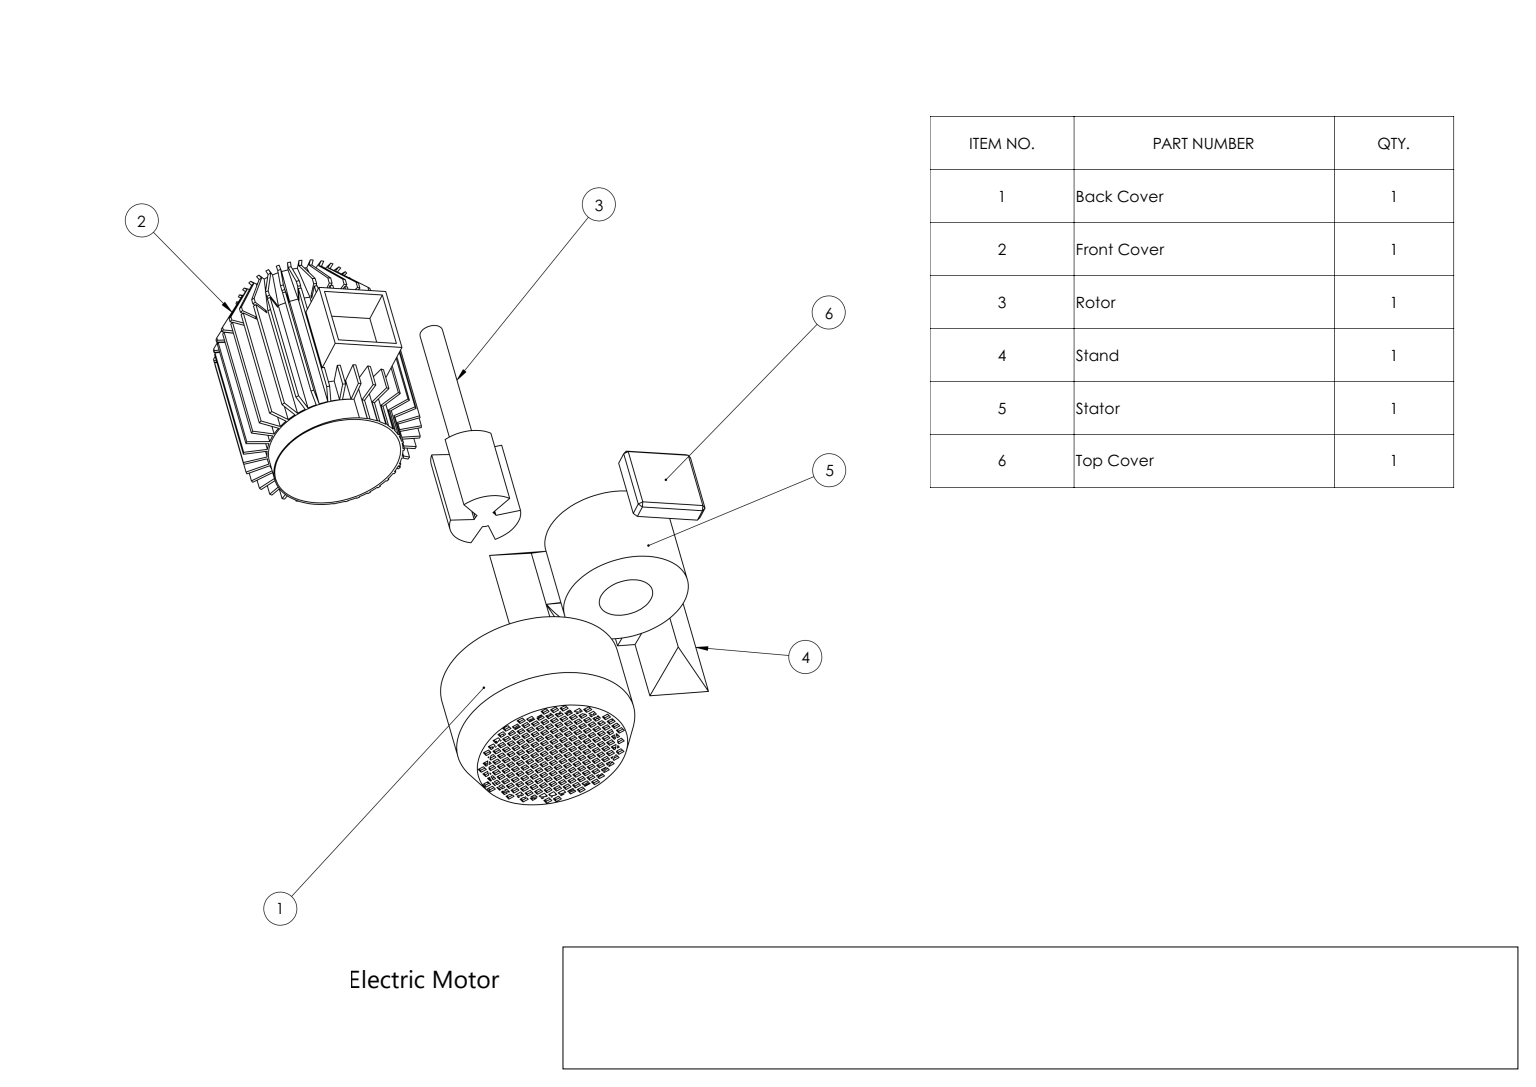
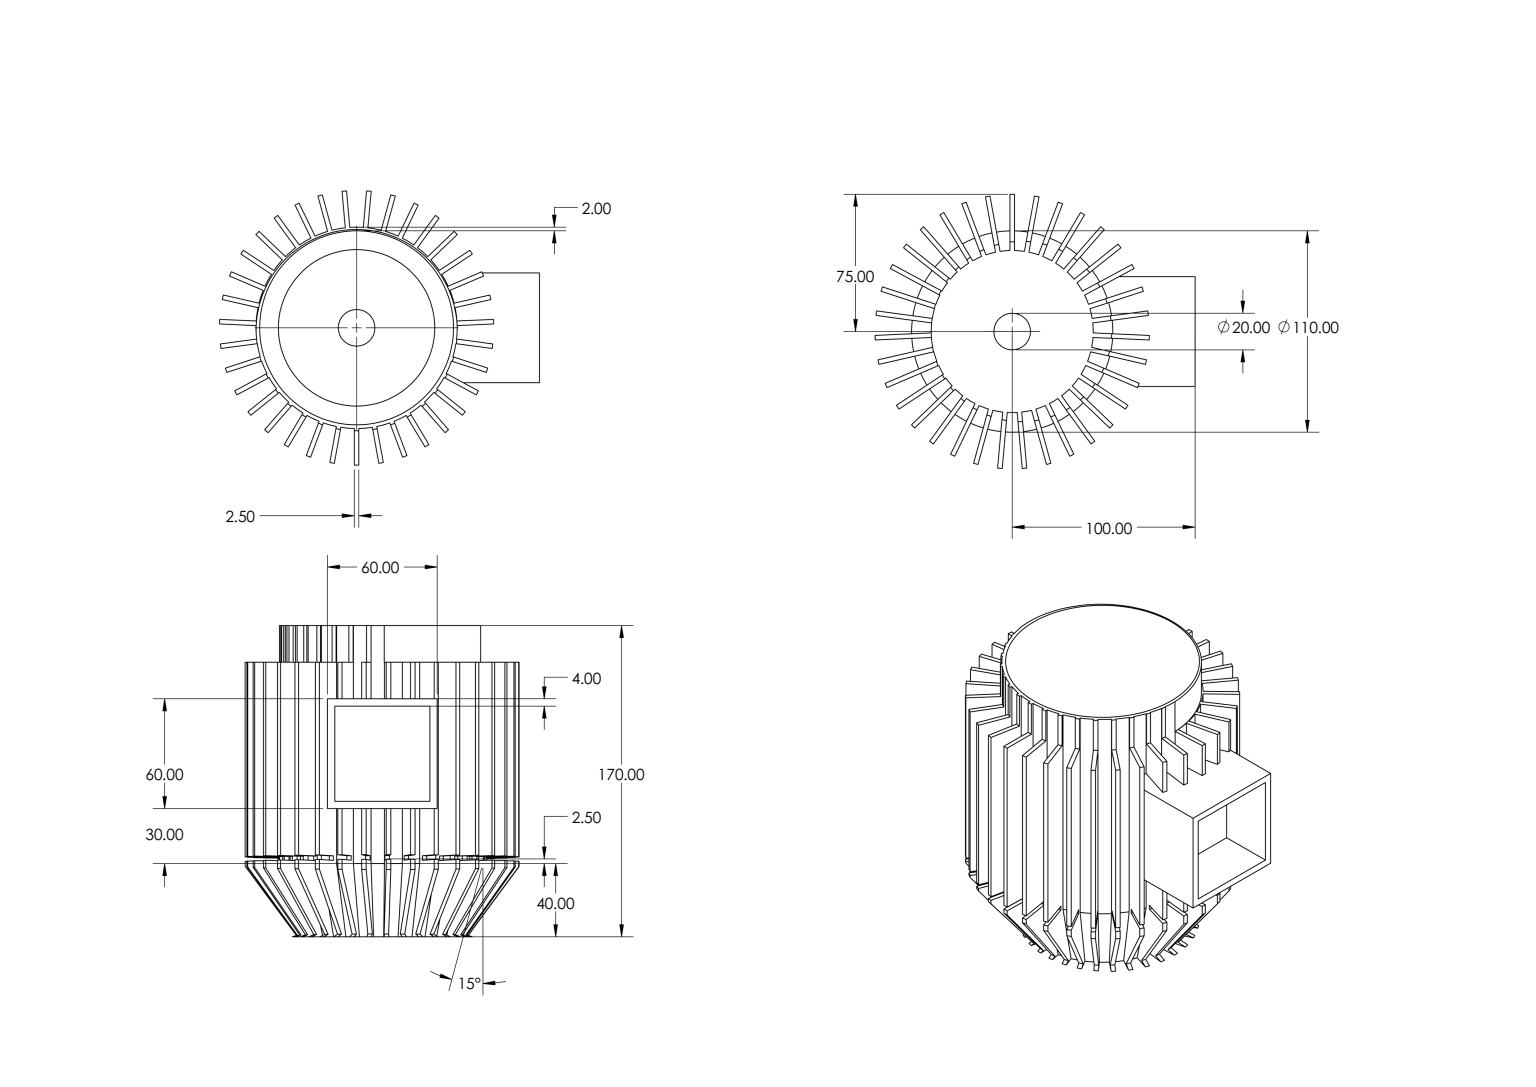
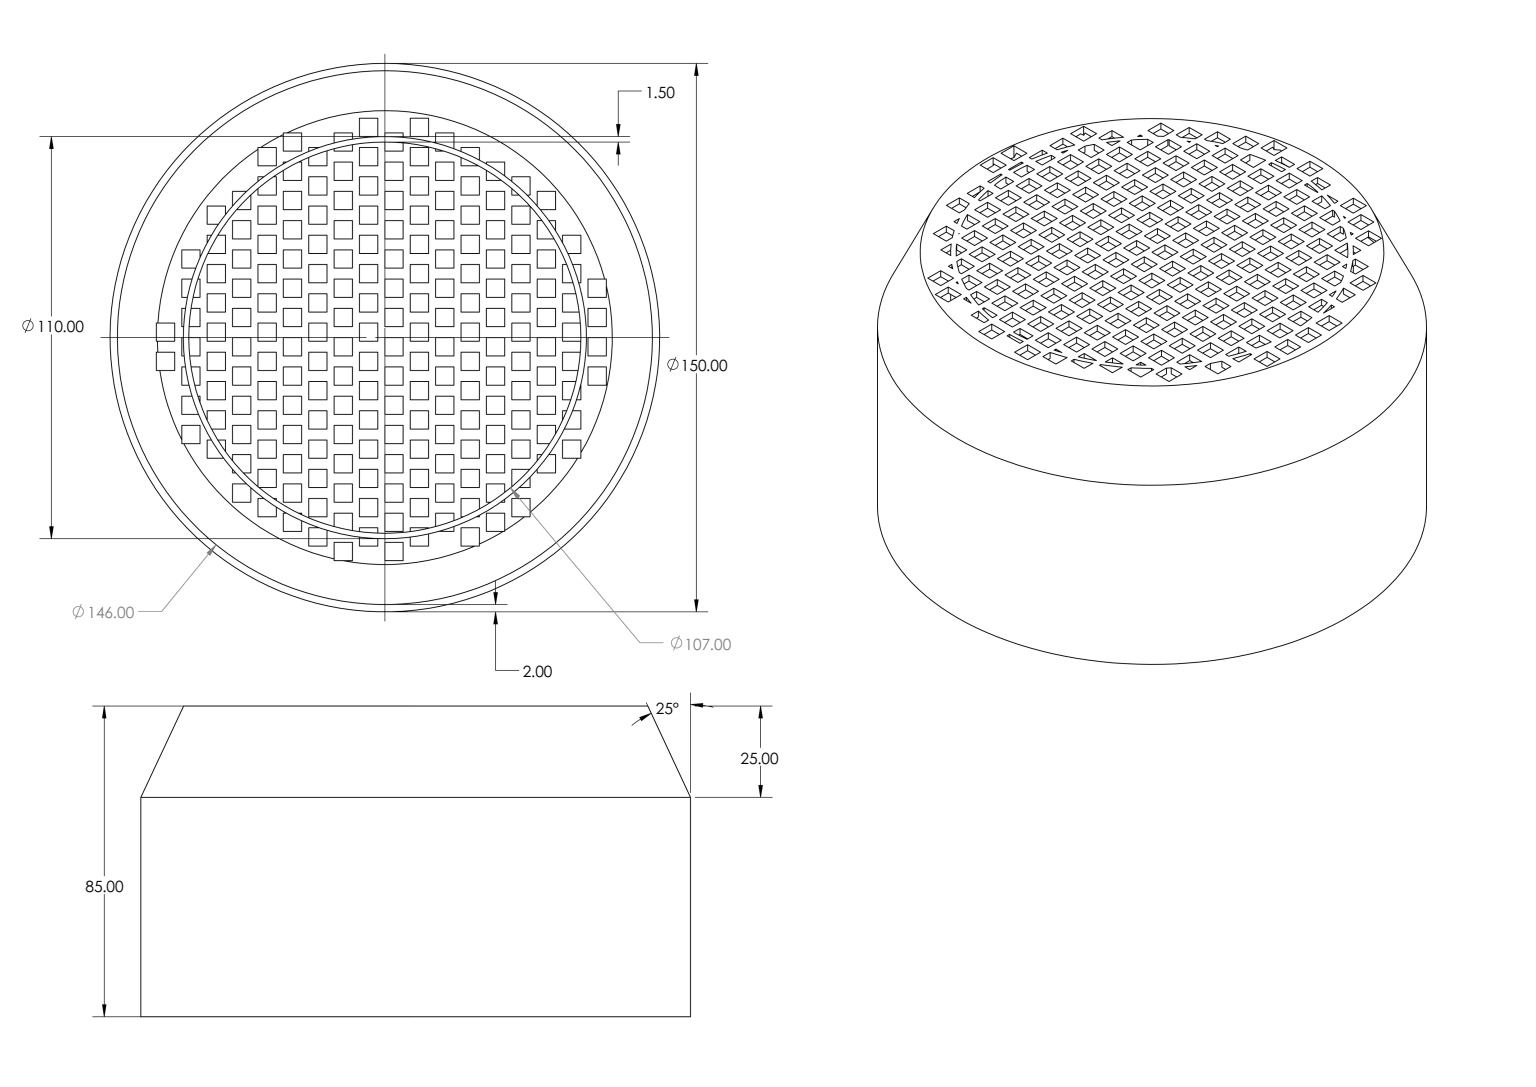
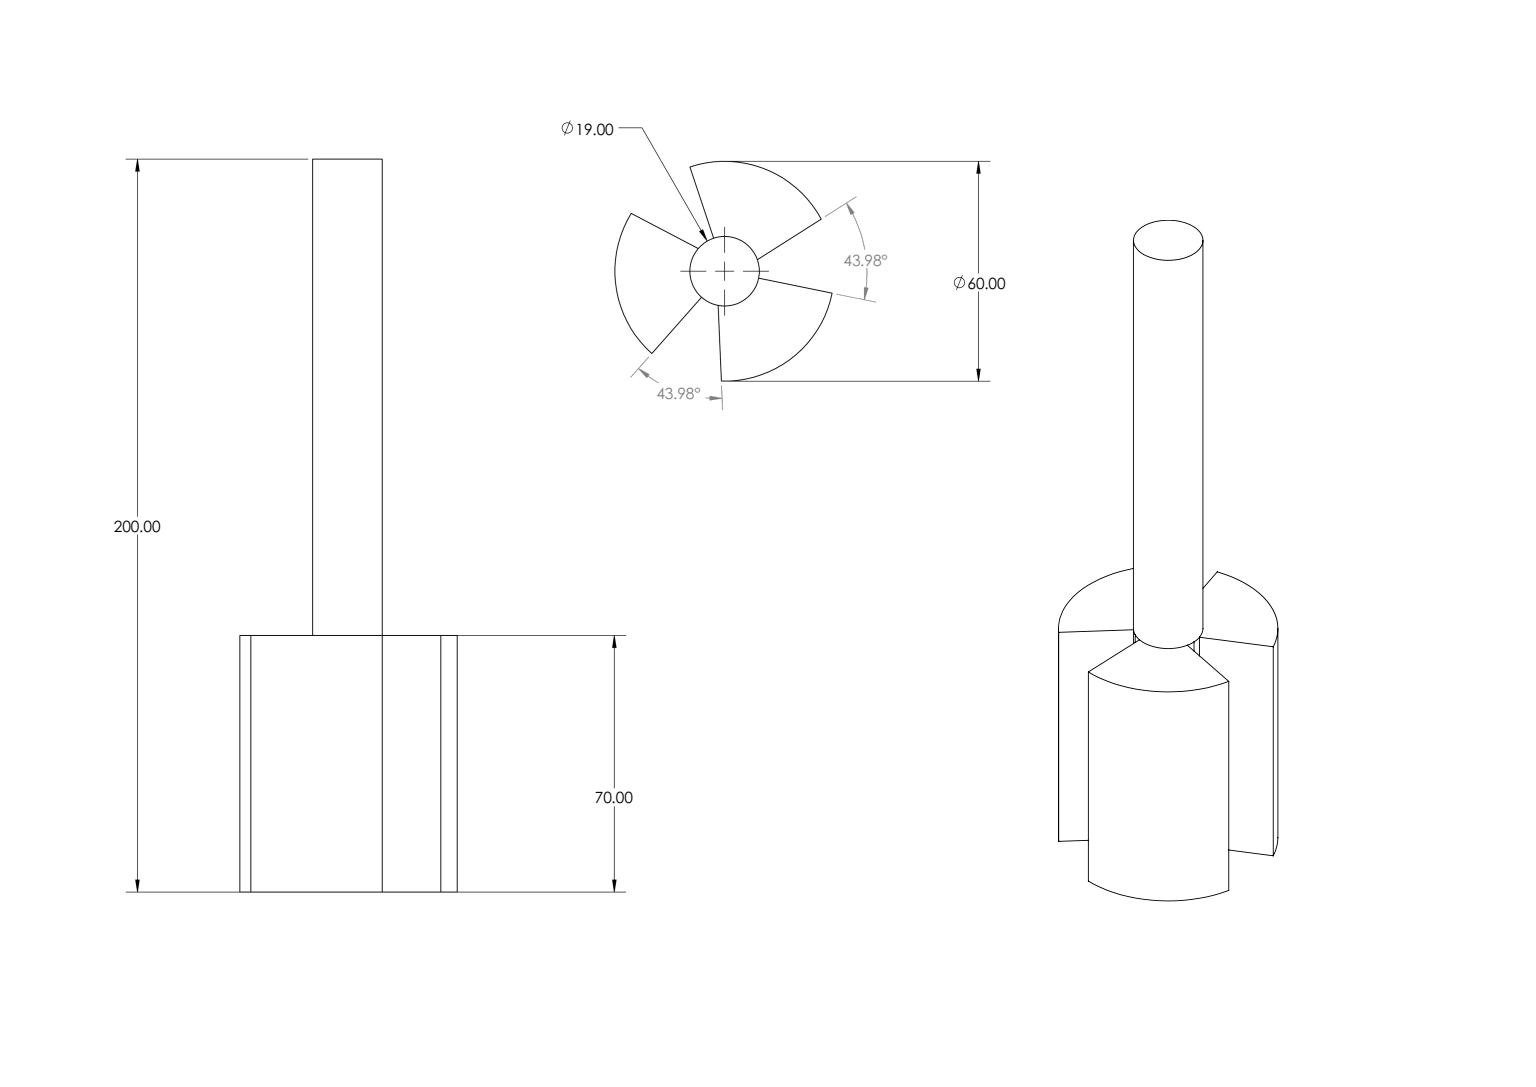
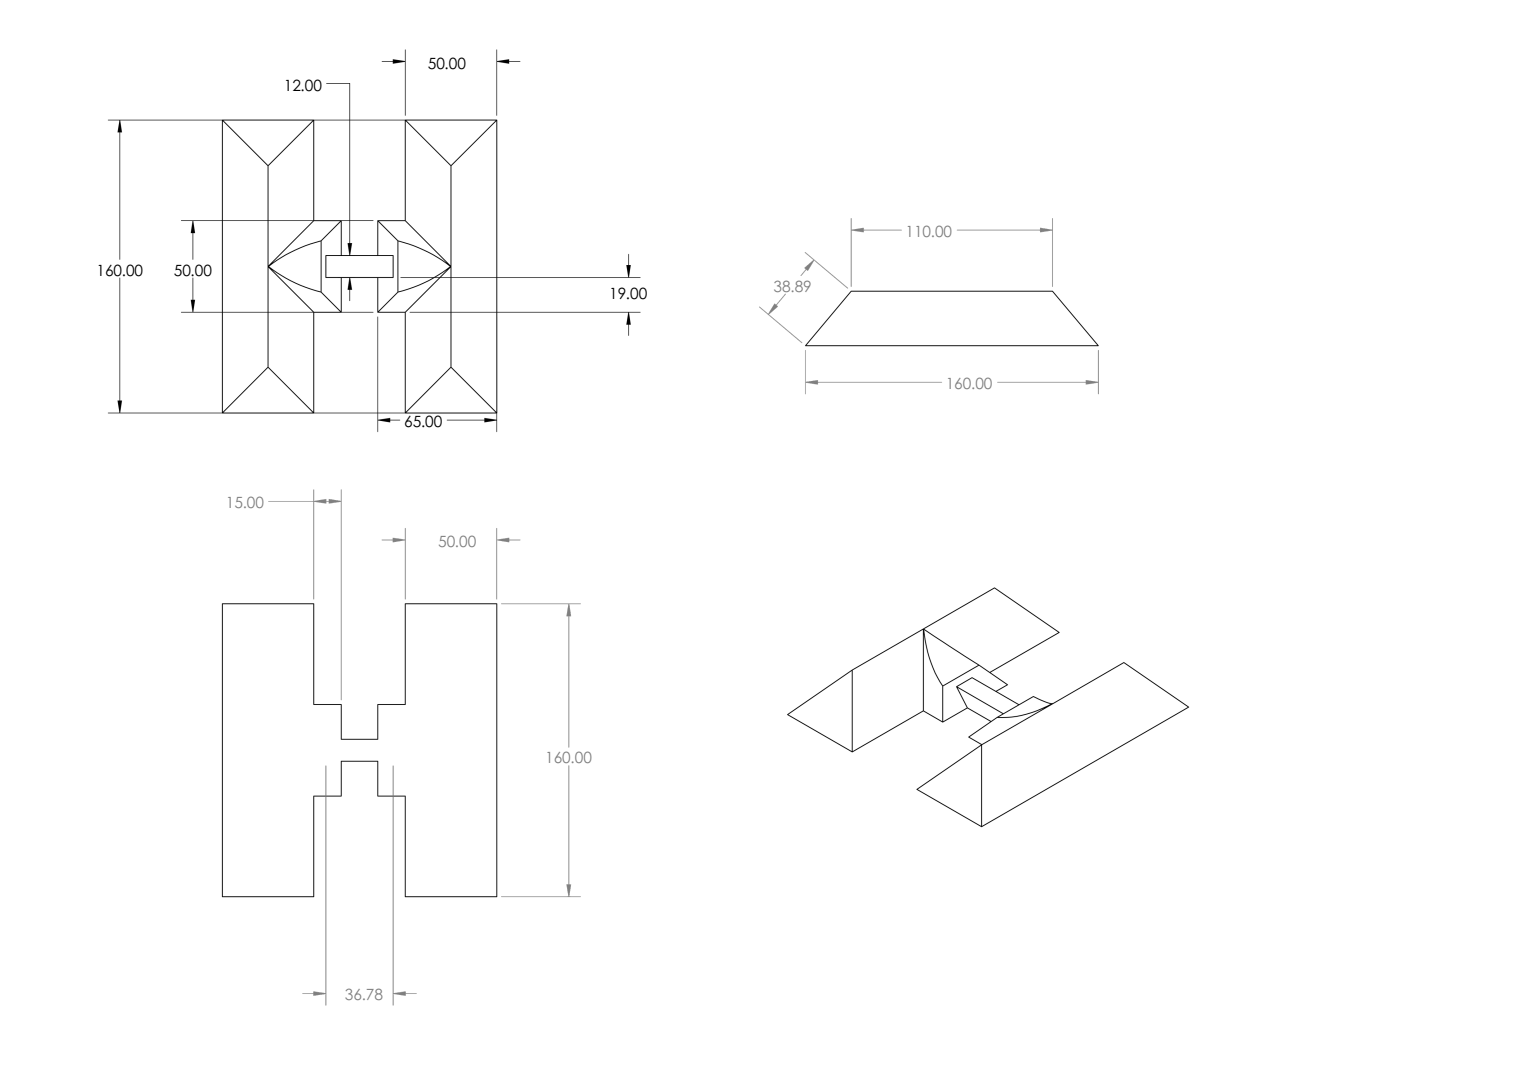
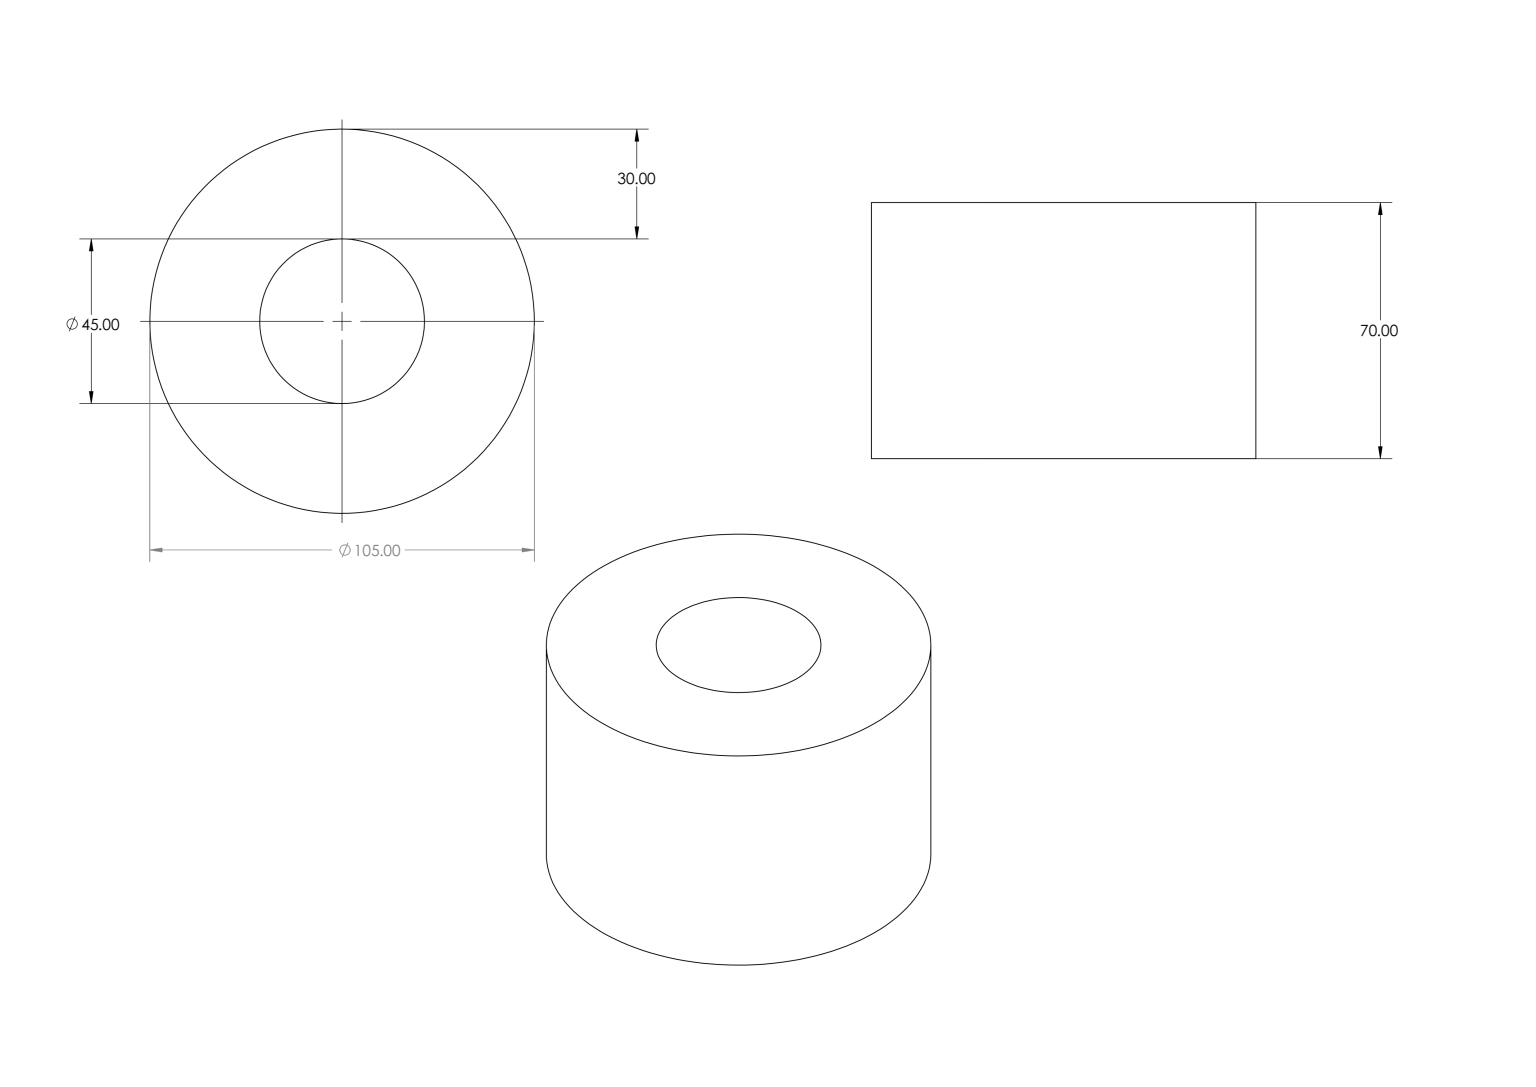
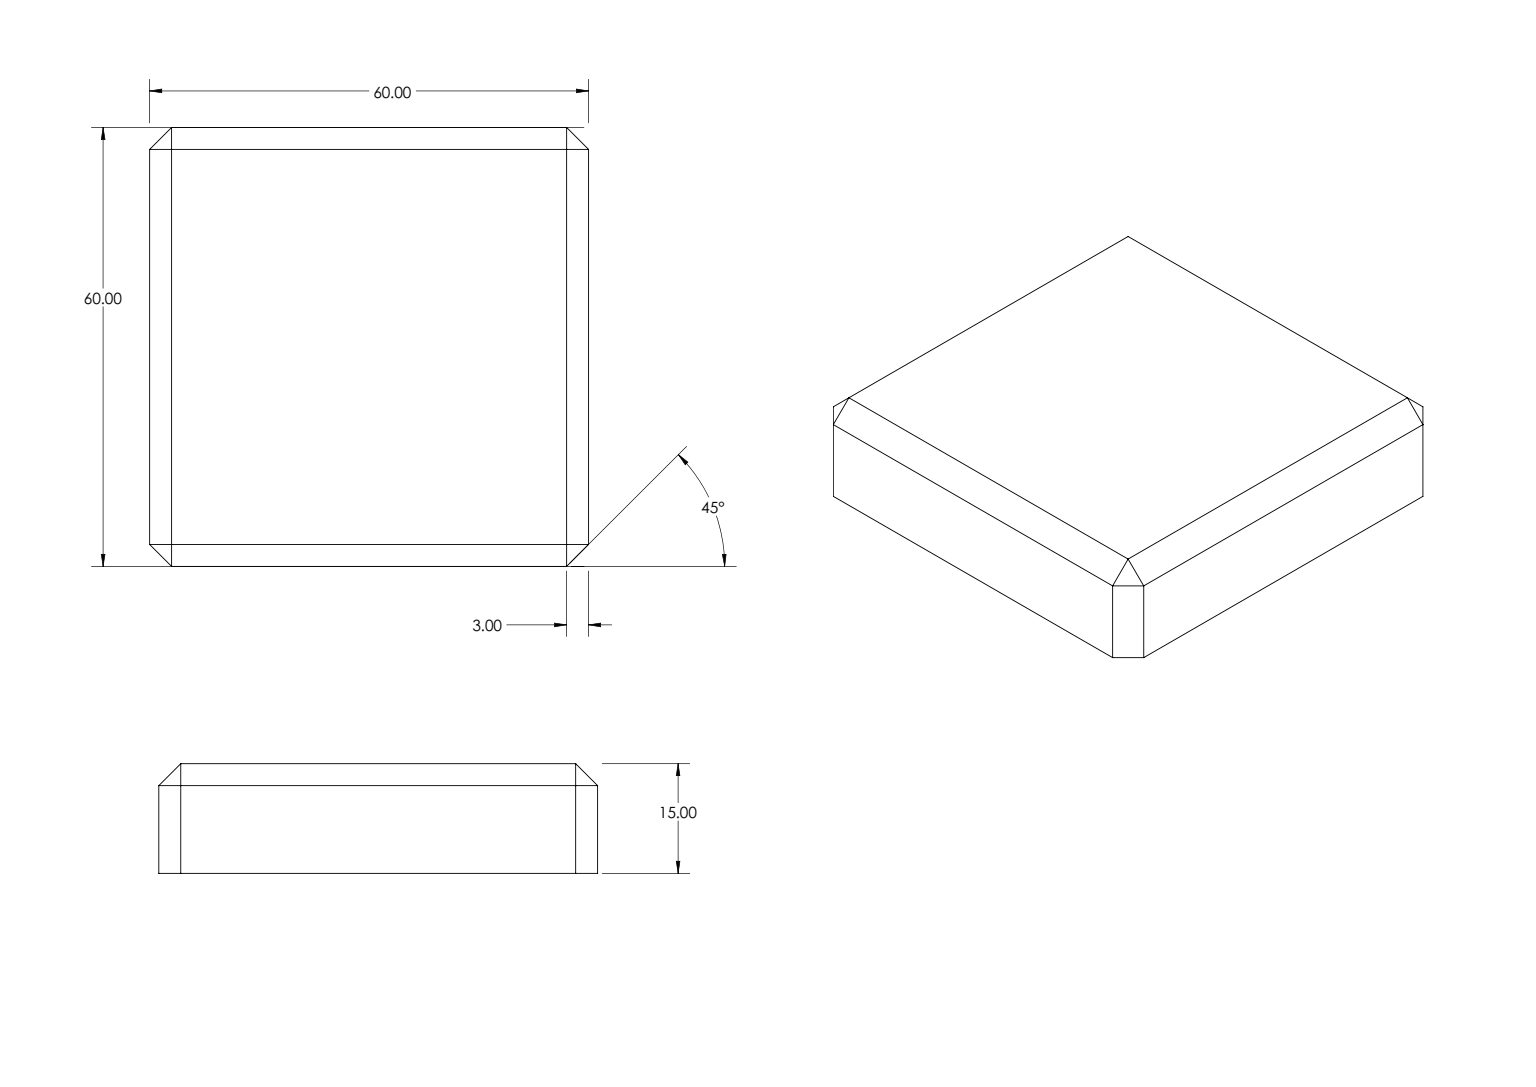
ISO-10303-21;
HEADER;
FILE_DESCRIPTION (('STEP AP214'),
    '1' );
FILE_NAME ('MAT-026',
    '2026-10-24T11:32:06',
    ( '' ),
    ( '' ),
    'SwSTEP 2.0',
    'SolidWorks 2025',
    '' );
FILE_SCHEMA (( 'AUTOMOTIVE_DESIGN' ));
ENDSEC;

DATA;
#1 = ORIENTED_EDGE ( 'NONE', *, *, #41545, .F. ) ;
#2 = DIRECTION ( 'NONE',  ( -0.000000000000000000, 1.000000000000000000, -0.000000000000000000 ) ) ;
#3 = DIRECTION ( 'NONE',  ( 0.5508969814521065267, -1.160734090543304660E-16, -0.8345732537212999791 ) ) ;
#4 = ORIENTED_EDGE ( 'NONE', *, *, #46916, .F. ) ;
#5 = FACE_OUTER_BOUND ( 'NONE', #37922, .T. ) ;
#6 = EDGE_CURVE ( 'NONE', #44322, #24123, #48534, .T. ) ;
#7 = EDGE_CURVE ( 'NONE', #12139, #21915, #4265, .T. ) ;
#8 = ORIENTED_EDGE ( 'NONE', *, *, #4272, .T. ) ;
#9 = ORIENTED_EDGE ( 'NONE', *, *, #40098, .F. ) ;
#10 = APPLICATION_PROTOCOL_DEFINITION ( 'draft international standard', 'automotive_design', 1998, #14403 ) ;
#11 = EDGE_CURVE ( 'NONE', #30195, #20299, #27750, .T. ) ;
#12 = EDGE_LOOP ( 'NONE', ( #15734, #18361, #15608, #13795, #3369 ) ) ;
#13 = LINE ( 'NONE', #35645, #41620 ) ;
#14 = AXIS2_PLACEMENT_3D ( 'NONE', #39527, #281, #16034 ) ;
#15 = LINE ( 'NONE', #8019, #14262 ) ;
#16 = VECTOR ( 'NONE', #2889, 39.37007874015748143 ) ;
#17 = DIRECTION ( 'NONE',  ( -1.000000000000000000, 0.000000000000000000, -0.000000000000000000 ) ) ;
#18 = CARTESIAN_POINT ( 'NONE',  ( -1.221295136473707243, 0.000000000000000000, 1.323086612934683215 ) ) ;
#19 = ORIENTED_EDGE ( 'NONE', *, *, #43886, .F. ) ;
#20 = ORIENTED_EDGE ( 'NONE', *, *, #36805, .T. ) ;
#21 = CARTESIAN_POINT ( 'NONE',  ( -1.985260859929297572, 0.000000000000000000, 0.9448818897637749625 ) ) ;
#22 = PLANE ( 'NONE',  #45699 ) ;
#23 = AXIS2_PLACEMENT_3D ( 'NONE', #45636, #18051, #42046 ) ;
#24 = VERTEX_POINT ( 'NONE', #23123 ) ;
#25 = CARTESIAN_POINT ( 'NONE',  ( 0.2727639067037610499, 0.000000000000000000, 1.417322834645662777 ) ) ;
#26 = DIRECTION ( 'NONE',  ( 1.000000000000000000, -0.000000000000000000, 0.000000000000000000 ) ) ;
#27 = EDGE_CURVE ( 'NONE', #10700, #41467, #27241, .T. ) ;
#28 = LINE ( 'NONE', #15774, #16810 ) ;
#29 = DIRECTION ( 'NONE',  ( 1.000000000000000000, 0.000000000000000000, 0.000000000000000000 ) ) ;
#30 = CARTESIAN_POINT ( 'NONE',  ( -1.091055626815042645, 3.346456692913386100, 1.889763779527550147 ) ) ;
#31 = ORIENTED_EDGE ( 'NONE', *, *, #29718, .F. ) ;
#32 = DIRECTION ( 'NONE',  ( -0.9998717552508122886, -0.01601477604151185785, 0.000000000000000000 ) ) ;
#34 = EDGE_CURVE ( 'NONE', #42119, #2129, #11002, .T. ) ;
#33 = DIRECTION ( 'NONE',  ( -0.2660368455666687892, 1.119010597708915320E-16, -0.9639628606958549062 ) ) ;
#35 = EDGE_CURVE ( 'NONE', #20944, #31120, #9767, .T. ) ;
#36 = EDGE_LOOP ( 'NONE', ( #12424, #14869, #12144, #2059, #5425, #21039 ) ) ;
#37 = ORIENTED_EDGE ( 'NONE', *, *, #50660, .F. ) ;
#38 = CARTESIAN_POINT ( 'NONE',  ( -0.3486774197067339376, 0.000000000000000000, 2.204724409448808764 ) ) ;
#39 = FACE_OUTER_BOUND ( 'NONE', #43225, .T. ) ;
#40 = DIRECTION ( 'NONE',  ( 0.8090169943749422332, -6.825848574540668760E-17, 0.5877852522924802425 ) ) ;
#41 = ORIENTED_EDGE ( 'NONE', *, *, #32145, .F. ) ;
#42 = VERTEX_POINT ( 'NONE', #46835 ) ;
#43 = FACE_OUTER_BOUND ( 'NONE', #749, .T. ) ;
#44 = ORIENTED_EDGE ( 'NONE', *, *, #47362, .F. ) ;
#45 = FACE_OUTER_BOUND ( 'NONE', #8156, .T. ) ;
#46 = ORIENTED_EDGE ( 'NONE', *, *, #11822, .F. ) ;
#47 = VECTOR ( 'NONE', #45929, 39.37007874015748143 ) ;
#48 = CARTESIAN_POINT ( 'NONE',  ( 0.08139965876239094178, 1.610780518492231694, 0.000000000000000000 ) ) ;
#49 = PLANE ( 'NONE',  #39583 ) ;
#50 = DIRECTION ( 'NONE',  ( 1.734723475976806848E-16, -0.000000000000000000, 1.000000000000000000 ) ) ;
#51 = VECTOR ( 'NONE', #38671, 39.37007874015748143 ) ;
#52 = ORIENTED_EDGE ( 'NONE', *, *, #36287, .T. ) ;
#53 = DIMENSIONAL_EXPONENTS ( 1.000000000000000000, 0.000000000000000000, 0.000000000000000000, 0.000000000000000000, 0.000000000000000000, 0.000000000000000000, 0.000000000000000000 ) ;
#54 = VERTEX_POINT ( 'NONE', #23369 ) ;
#55 = ORIENTED_EDGE ( 'NONE', *, *, #40975, .F. ) ;
#56 = DIRECTION ( 'NONE',  ( -6.104789737168205836E-17, 1.000000000000000000, 1.134460028949762747E-16 ) ) ;
#57 = PLANE ( 'NONE',  #9017 ) ;
#58 = VERTEX_POINT ( 'NONE', #22875 ) ;
#59 = EDGE_LOOP ( 'NONE', ( #42044, #32903, #33887, #36079 ) ) ;
#60 = CARTESIAN_POINT ( 'NONE',  ( 1.091055626815043311, 3.346456692913386100, 1.801691980386208591 ) ) ;
#61 = DIRECTION ( 'NONE',  ( 1.000000000000000000, 0.000000000000000000, 0.000000000000000000 ) ) ;
#62 = AXIS2_PLACEMENT_3D ( 'NONE', #50431, #10999, #38625 ) ;
#63 = DIRECTION ( 'NONE',  ( -0.01601477604151182663, 0.9998717552508123996, -0.000000000000000000 ) ) ;
#64 = ORIENTED_EDGE ( 'NONE', *, *, #33322, .T. ) ;
#65 = VERTEX_POINT ( 'NONE', #11508 ) ;
#66 = DIRECTION ( 'NONE',  ( -0.01601477604151182663, 0.9998717552508123996, -0.000000000000000000 ) ) ;
#67 = LINE ( 'NONE', #23560, #12596 ) ;
#68 = DIRECTION ( 'NONE',  ( 1.734723475976806848E-16, -0.000000000000000000, 1.000000000000000000 ) ) ;
#69 = ORIENTED_EDGE ( 'NONE', *, *, #18487, .T. ) ;
#70 = CARTESIAN_POINT ( 'NONE',  ( -1.775400203342670347, 1.691590761327236958, -2.359903268218729089 ) ) ;
#71 = CARTESIAN_POINT ( 'NONE',  ( -1.684292108503798069, 6.692913385826772199, 1.406123411605399331 ) ) ;
#72 = EDGE_CURVE ( 'NONE', #49919, #13698, #39123, .T. ) ;
#73 = ORIENTED_EDGE ( 'NONE', *, *, #20191, .T. ) ;
#74 = EDGE_CURVE ( 'NONE', #40300, #35551, #37050, .T. ) ;
#75 = LINE ( 'NONE', #35456, #37348 ) ;
#76 = ORIENTED_EDGE ( 'NONE', *, *, #46509, .T. ) ;
#77 = ORIENTED_EDGE ( 'NONE', *, *, #24929, .F. ) ;
#78 = LINE ( 'NONE', #47286, #4826 ) ;
#79 = EDGE_CURVE ( 'NONE', #50716, #12064, #21041, .T. ) ;
#80 = CARTESIAN_POINT ( 'NONE',  ( -1.723687301221637380, 0.000000000000000000, -1.311649477509825745 ) ) ;
#81 = CARTESIAN_POINT ( 'NONE',  ( -0.8942052331142547050, 3.346456692913386100, 0.3149606299212580063 ) ) ;
#82 = EDGE_CURVE ( 'NONE', #36271, #42094, #44767, .T. ) ;
#83 = CARTESIAN_POINT ( 'NONE',  ( -2.952069331832154919, 2.755905511811027164, 1.181102362204724088 ) ) ;
#84 = ORIENTED_EDGE ( 'NONE', *, *, #20132, .T. ) ;
#85 = ORIENTED_EDGE ( 'NONE', *, *, #1655, .T. ) ;
#86 = ORIENTED_EDGE ( 'NONE', *, *, #35024, .F. ) ;
#87 = CARTESIAN_POINT ( 'NONE',  ( -2.454875160333845674, 0.000000000000000000, -0.3543307086614173040 ) ) ;
#88 = DIRECTION ( 'NONE',  ( -0.9362348706397368714, 0.000000000000000000, -0.3513748240813434620 ) ) ;
#89 = VECTOR ( 'NONE', #24437, 39.37007874015748143 ) ;
#90 = AXIS2_PLACEMENT_3D ( 'NONE', #4084, #31446, #43558 ) ;
#91 = ADVANCED_FACE ( 'NONE', ( #40920 ), #12786, .F. ) ;
#92 = DIRECTION ( 'NONE',  ( 0.000000000000000000, 0.000000000000000000, 1.000000000000000000 ) ) ;
#93 = LINE ( 'NONE', #12233, #1484 ) ;
#94 = ORIENTED_EDGE ( 'NONE', *, *, #13556, .F. ) ;
#95 = DIRECTION ( 'NONE',  ( 0.000000000000000000, 0.000000000000000000, -1.000000000000000000 ) ) ;
#96 = EDGE_CURVE ( 'NONE', #18423, #30154, #5544, .T. ) ;
#97 = VECTOR ( 'NONE', #41859, 39.37007874015748143 ) ;
#98 = CARTESIAN_POINT ( 'NONE',  ( 0.8182917201112819283, 0.000000000000000000, -0.6692913385826764205 ) ) ;
#99 = EDGE_LOOP ( 'NONE', ( #34506, #24501, #26752, #36610 ) ) ;
#100 = AXIS2_PLACEMENT_3D ( 'NONE', #33022, #17513, #29384 ) ;
#101 = LINE ( 'NONE', #15846, #7552 ) ;
#102 = CARTESIAN_POINT ( 'NONE',  ( -0.8182917201112819283, 3.267716535433071279, -1.417322834645664331 ) ) ;
#103 = PLANE ( 'NONE',  #37876 ) ;
#104 = EDGE_CURVE ( 'NONE', #46852, #34665, #24146, .T. ) ;
#105 = ORIENTED_EDGE ( 'NONE', *, *, #7025, .F. ) ;
#106 = PLANE ( 'NONE',  #20146 ) ;
#107 = CARTESIAN_POINT ( 'NONE',  ( 1.636583440222563857, 3.267716535433071279, -2.839019714148966584E-16 ) ) ;
#108 = CARTESIAN_POINT ( 'NONE',  ( 2.576863348864710801, 1.456480680773285741, 1.442554885838449596 ) ) ;
#109 = ORIENTED_EDGE ( 'NONE', *, *, #48882, .F. ) ;
#110 = LINE ( 'NONE', #16120, #44470 ) ;
#111 = ORIENTED_EDGE ( 'NONE', *, *, #20916, .T. ) ;
#112 = CARTESIAN_POINT ( 'NONE',  ( -1.312623452344869657, 1.205361022782829114E-17, 1.722945714930904648 ) ) ;
#113 = EDGE_CURVE ( 'NONE', #26527, #41000, #12273, .T. ) ;
#114 = FACE_OUTER_BOUND ( 'NONE', #41587, .T. ) ;
#115 = B_SPLINE_CURVE_WITH_KNOTS ( 'NONE', 3,
 ( #45279, #2696, #10703, #6825 ),
 .UNSPECIFIED., .F., .F.,
 ( 4, 4 ),
 ( 0.0008439222489648032970, 0.003344231527576960444 ),
 .UNSPECIFIED. ) ;
#116 = DIRECTION ( 'NONE',  ( -0.9959742939952384022, 1.288287287306305283E-16, -0.08963930890344089242 ) ) ;
#117 = DIRECTION ( 'NONE',  ( -1.000000000000000000, 0.000000000000000000, 1.734723475976806848E-16 ) ) ;
#118 = ORIENTED_EDGE ( 'NONE', *, *, #20637, .F. ) ;
#119 = ORIENTED_EDGE ( 'NONE', *, *, #43992, .F. ) ;
#120 = FACE_OUTER_BOUND ( 'NONE', #11448, .T. ) ;
#121 = DIRECTION ( 'NONE',  ( -1.000000000000000000, -0.000000000000000000, -0.000000000000000000 ) ) ;
#122 = VERTEX_POINT ( 'NONE', #36283 ) ;
#123 = DIRECTION ( 'NONE',  ( 1.000000000000000000, 0.000000000000000000, -3.469446951953613696E-16 ) ) ;
#124 = LINE ( 'NONE', #20773, #45818 ) ;
#125 = CARTESIAN_POINT ( 'NONE',  ( 0.000000000000000000, 1.574803149606302854, 0.000000000000000000 ) ) ;
#126 = VECTOR ( 'NONE', #40753, 39.37007874015748143 ) ;
#127 = FACE_OUTER_BOUND ( 'NONE', #15551, .T. ) ;
#128 = AXIS2_PLACEMENT_3D ( 'NONE', #50687, #394, #43496 ) ;
#129 = VERTEX_POINT ( 'NONE', #32937 ) ;
#130 = ORIENTED_EDGE ( 'NONE', *, *, #3262, .F. ) ;
#131 = FACE_OUTER_BOUND ( 'NONE', #28949, .T. ) ;
#132 = CARTESIAN_POINT ( 'NONE',  ( 0.2727639067037604392, 3.267716535433071279, -4.731699523581607276E-17 ) ) ;
#133 = DIRECTION ( 'NONE',  ( -0.000000000000000000, 1.000000000000000000, -0.000000000000000000 ) ) ;
#134 = CIRCLE ( 'NONE', #18276, 2.106299212598425008 ) ;
#135 = ORIENTED_EDGE ( 'NONE', *, *, #12667, .T. ) ;
#136 = DIRECTION ( 'NONE',  ( -1.000000000000000000, 0.000000000000000000, 0.000000000000000000 ) ) ;
#137 = ORIENTED_EDGE ( 'NONE', *, *, #4680, .F. ) ;
#138 = ORIENTED_EDGE ( 'NONE', *, *, #50267, .T. ) ;
#139 = DIRECTION ( 'NONE',  ( 1.000000000000000000, -0.000000000000000000, 0.000000000000000000 ) ) ;
#140 = EDGE_CURVE ( 'NONE', #9076, #17493, #4524, .T. ) ;
#141 = CIRCLE ( 'NONE', #36418, 2.164630168518208109 ) ;
#142 = EDGE_CURVE ( 'NONE', #28374, #48689, #28779, .T. ) ;
#143 = ORIENTED_EDGE ( 'NONE', *, *, #7966, .T. ) ;
#144 = ORIENTED_EDGE ( 'NONE', *, *, #45478, .T. ) ;
#145 = CARTESIAN_POINT ( 'NONE',  ( 1.773598097765477277, 1.637884173412089250, 1.477342561509449759 ) ) ;
#146 = EDGE_CURVE ( 'NONE', #16314, #49284, #20780, .T. ) ;
#147 = ORIENTED_EDGE ( 'NONE', *, *, #31440, .T. ) ;
#148 = CARTESIAN_POINT ( 'NONE',  ( -1.439733046521776583, 0.000000000000000000, -0.6299212598425177889 ) ) ;
#149 = CARTESIAN_POINT ( 'NONE',  ( 0.4139892466755871747, 1.013814418196932632, 2.556881760885583610 ) ) ;
#150 = CARTESIAN_POINT ( 'NONE',  ( -1.613247378701003099, 1.616446044927785097, -1.474335889616294581 ) ) ;
#151 = CARTESIAN_POINT ( 'NONE',  ( -0.2480359799030329715, -0.6299212598425202314, 0.2799391584775194342 ) ) ;
#152 = CARTESIAN_POINT ( 'NONE',  ( -0.3486774197067339376, 0.000000000000000000, 0.3149606299212577287 ) ) ;
#153 = CARTESIAN_POINT ( 'NONE',  ( 1.363819533518803251, 3.346456692913386100, -0.4724409448818889246 ) ) ;
#154 = ORIENTED_EDGE ( 'NONE', *, *, #33358, .F. ) ;
#155 = FACE_OUTER_BOUND ( 'NONE', #42021, .T. ) ;
#156 = CARTESIAN_POINT ( 'NONE',  ( 1.560669927219590747, 0.000000000000000000, 0.1574803149606283648 ) ) ;
#157 = CARTESIAN_POINT ( 'NONE',  ( 0.04921259842519689481, 0.01913872127211492871, 1.877530537165238655 ) ) ;
#158 = ORIENTED_EDGE ( 'NONE', *, *, #45905, .F. ) ;
#159 = VECTOR ( 'NONE', #591, 39.37007874015748143 ) ;
#160 = DIRECTION ( 'NONE',  ( 1.000000000000000000, 0.000000000000000000, -3.469446951953613696E-16 ) ) ;
#161 = CARTESIAN_POINT ( 'NONE',  ( -2.006180841960468086, 1.679905088511975952, -1.383235759546366461 ) ) ;
#162 = VERTEX_POINT ( 'NONE', #12522 ) ;
#163 = PLANE ( 'NONE',  #50112 ) ;
#164 = EDGE_CURVE ( 'NONE', #49397, #27417, #48360, .T. ) ;
#165 = CARTESIAN_POINT ( 'NONE',  ( -0.8942052331142547050, 0.000000000000000000, 1.574803149606291974 ) ) ;
#166 = B_SPLINE_CURVE_WITH_KNOTS ( 'NONE', 3,
 ( #38483, #29261, #29524, #7238 ),
 .UNSPECIFIED., .F., .F.,
 ( 4, 4 ),
 ( 0.01106655392343035803, 0.03073596134458069645 ),
 .UNSPECIFIED. ) ;
#167 = DIRECTION ( 'NONE',  ( -0.000000000000000000, -1.000000000000000000, -0.000000000000000000 ) ) ;
#168 = VECTOR ( 'NONE', #49245, 39.37007874015748143 ) ;
#169 = VECTOR ( 'NONE', #37058, 39.37007874015748143 ) ;
#170 = DIRECTION ( 'NONE',  ( -0.9998717552508121775, -0.01601477604151182663, 0.000000000000000000 ) ) ;
#171 = ORIENTED_EDGE ( 'NONE', *, *, #24690, .T. ) ;
#172 = CARTESIAN_POINT ( 'NONE',  ( -1.636583440222564301, 0.000000000000000000, -1.259842519685034468 ) ) ;
#173 = ADVANCED_FACE ( 'NONE', ( #43745 ), #44519, .F. ) ;
#174 = DIRECTION ( 'NONE',  ( -0.000000000000000000, -1.000000000000000000, -0.000000000000000000 ) ) ;
#175 = VECTOR ( 'NONE', #24706, 39.37007874015748143 ) ;
#176 = DIRECTION ( 'NONE',  ( -3.469446951953613696E-16, 0.000000000000000000, -1.000000000000000000 ) ) ;
#177 = CARTESIAN_POINT ( 'NONE',  ( 1.363819533518803029, 0.000000000000000000, -1.102362204724405714 ) ) ;
#178 = ORIENTED_EDGE ( 'NONE', *, *, #35535, .T. ) ;
#179 = EDGE_CURVE ( 'NONE', #37571, #48901, #4780, .T. ) ;
#180 = VERTEX_POINT ( 'NONE', #28260 ) ;
#181 = ORIENTED_EDGE ( 'NONE', *, *, #30395, .F. ) ;
#182 = DIRECTION ( 'NONE',  ( -1.000000000000000000, 0.000000000000000000, 0.000000000000000000 ) ) ;
#183 = VERTEX_POINT ( 'NONE', #20529 ) ;
#184 = EDGE_CURVE ( 'NONE', #12327, #2318, #1159, .T. ) ;
#185 = DIRECTION ( 'NONE',  ( -3.986037398843765983E-20, -1.000000000000000000, -1.160734090543304660E-16 ) ) ;
#186 = FACE_OUTER_BOUND ( 'NONE', #12865, .T. ) ;
#187 = VERTEX_POINT ( 'NONE', #32677 ) ;
#188 = EDGE_CURVE ( 'NONE', #9810, #3944, #698, .T. ) ;
#189 = DIRECTION ( 'NONE',  ( 0.9749279121818259508, 0.000000000000000000, -0.2225209339563041788 ) ) ;
#190 = ORIENTED_EDGE ( 'NONE', *, *, #20504, .F. ) ;
#191 = DIRECTION ( 'NONE',  ( 1.000000000000000000, 0.000000000000000000, -0.000000000000000000 ) ) ;
#192 = CARTESIAN_POINT ( 'NONE',  ( 1.560669927219590303, 3.186757942779276043, -1.929133858267710666 ) ) ;
#193 = ORIENTED_EDGE ( 'NONE', *, *, #27839, .T. ) ;
#194 = ORIENTED_EDGE ( 'NONE', *, *, #36175, .F. ) ;
#195 = LINE ( 'NONE', #42802, #49556 ) ;
#196 = VERTEX_POINT ( 'NONE', #24912 ) ;
#197 = EDGE_CURVE ( 'NONE', #41904, #49094, #20264, .T. ) ;
#198 = VECTOR ( 'NONE', #32810, 39.37007874015748854 ) ;
#199 = CARTESIAN_POINT ( 'NONE',  ( 0.7423782071083092626, 3.346456692913386100, 1.259842519685033357 ) ) ;
#200 = B_SPLINE_CURVE_WITH_KNOTS ( 'NONE', 3,
 ( #50656, #15354, #2476, #30092 ),
 .UNSPECIFIED., .F., .F.,
 ( 4, 4 ),
 ( 0.001007621139641426671, 0.003507930418253497190 ),
 .UNSPECIFIED. ) ;
#201 = ORIENTED_EDGE ( 'NONE', *, *, #10126, .T. ) ;
#202 = ORIENTED_EDGE ( 'NONE', *, *, #12575, .F. ) ;
#203 = ADVANCED_FACE ( 'NONE', ( #47849 ), #44006, .F. ) ;
#204 = DIRECTION ( 'NONE',  ( -0.000000000000000000, -1.000000000000000000, -0.000000000000000000 ) ) ;
#205 = CARTESIAN_POINT ( 'NONE',  ( -0.04921259842519695726, 0.5249316497054296038, 1.883403453826241192 ) ) ;
#206 = ORIENTED_EDGE ( 'NONE', *, *, #20888, .T. ) ;
#207 = AXIS2_PLACEMENT_3D ( 'NONE', #10792, #6422, #49732 ) ;
#208 = CARTESIAN_POINT ( 'NONE',  ( 0.4696143004045476577, 3.346456692913386100, -2.053280005709960054 ) ) ;
#209 = VERTEX_POINT ( 'NONE', #2440 ) ;
#210 = DIRECTION ( 'NONE',  ( 1.734723475976806848E-16, -0.000000000000000000, 1.000000000000000000 ) ) ;
#211 = VECTOR ( 'NONE', #28730, 39.37007874015748143 ) ;
#212 = VECTOR ( 'NONE', #8799, 39.37007874015748143 ) ;
#213 = LINE ( 'NONE', #20347, #9362 ) ;
#214 = LINE ( 'NONE', #28342, #18968 ) ;
#215 = ORIENTED_EDGE ( 'NONE', *, *, #9595, .F. ) ;
#216 = VERTEX_POINT ( 'NONE', #10437 ) ;
#217 = CARTESIAN_POINT ( 'NONE',  ( -2.182111253630085734, 3.267716535433070391, -1.099868863272876141 ) ) ;
#218 = DIRECTION ( 'NONE',  ( -1.000000000000000000, 0.000000000000000000, -0.000000000000000000 ) ) ;
#219 = DIRECTION ( 'NONE',  ( -0.9998717552508121775, -0.01601477604151182663, 0.000000000000000000 ) ) ;
#220 = CARTESIAN_POINT ( 'NONE',  ( -0.8942052331142547050, 3.346456692913386100, 0.3149606299212580063 ) ) ;
#221 = CARTESIAN_POINT ( 'NONE',  ( -2.612298101585049714, 1.674454801174855234, -0.6467181869387608195 ) ) ;
#222 = CARTESIAN_POINT ( 'NONE',  ( -1.172858943013145749, 6.692913385826772199, 1.867085387823100850 ) ) ;
#223 = ORIENTED_EDGE ( 'NONE', *, *, #26199, .T. ) ;
#224 = EDGE_CURVE ( 'NONE', #15315, #8682, #2410, .T. ) ;
#225 = CARTESIAN_POINT ( 'NONE',  ( -0.7381027496704858359, 0.000000000000000000, -2.859439394060923512 ) ) ;
#226 = ORIENTED_EDGE ( 'NONE', *, *, #21083, .T. ) ;
#227 = CARTESIAN_POINT ( 'NONE',  ( 0.8067290215917978236, 6.692913385826772199, 2.009464521518182334 ) ) ;
#228 = ORIENTED_EDGE ( 'NONE', *, *, #16699, .T. ) ;
#229 = DIRECTION ( 'NONE',  ( -0.01601477604151182663, 0.9998717552508123996, -0.000000000000000000 ) ) ;
#230 = CARTESIAN_POINT ( 'NONE',  ( -1.330011864698828816, 1.686599376747761614, -1.746878811320646152 ) ) ;
#231 = EDGE_CURVE ( 'NONE', #1621, #46197, #37830, .T. ) ;
#232 = CARTESIAN_POINT ( 'NONE',  ( -0.5455278134075214336, 3.346456692913386100, 2.095509194042718182 ) ) ;
#233 = ORIENTED_EDGE ( 'NONE', *, *, #15254, .F. ) ;
#234 = ADVANCED_FACE ( 'NONE', ( #37814 ), #18182, .F. ) ;
#235 = EDGE_CURVE ( 'NONE', #22970, #35146, #10690, .T. ) ;
#236 = VECTOR ( 'NONE', #4525, 39.37007874015748143 ) ;
#237 = CARTESIAN_POINT ( 'NONE',  ( 1.091055626815042645, 3.346456692913386100, 1.062992125984246083 ) ) ;
#238 = EDGE_LOOP ( 'NONE', ( #10056, #19126, #49833, #39898 ) ) ;
#239 = CARTESIAN_POINT ( 'NONE',  ( 2.623503965249849301, 1.455362298632098428, 1.355882097269874187 ) ) ;
#240 = ORIENTED_EDGE ( 'NONE', *, *, #12188, .T. ) ;
#241 = VECTOR ( 'NONE', #21691, 39.37007874015748143 ) ;
#242 = VECTOR ( 'NONE', #7716, 39.37007874015748143 ) ;
#243 = DIRECTION ( 'NONE',  ( 1.000000000000000000, 0.000000000000000000, 0.000000000000000000 ) ) ;
#244 = DIRECTION ( 'NONE',  ( -0.9998717552508122886, -0.01601477604151185785, 0.000000000000000000 ) ) ;
#245 = EDGE_LOOP ( 'NONE', ( #3861, #29192, #10688, #26365 ) ) ;
#246 = AXIS2_PLACEMENT_3D ( 'NONE', #45801, #41451, #45296 ) ;
#247 = LINE ( 'NONE', #16001, #16461 ) ;
#248 = ORIENTED_EDGE ( 'NONE', *, *, #20841, .F. ) ;
#249 = ORIENTED_EDGE ( 'NONE', *, *, #14890, .F. ) ;
#250 = CARTESIAN_POINT ( 'NONE',  ( -0.3937007874015748254, 0.3937007874015748254, -0.7480314960629921295 ) ) ;
#251 = CARTESIAN_POINT ( 'NONE',  ( -0.3486774197067339376, 3.267716535433071279, -8.878505979408855953E-16 ) ) ;
#252 = PLANE ( 'NONE',  #20266 ) ;
#253 = ADVANCED_FACE ( 'NONE', ( #6050 ), #49625, .F. ) ;
#254 = ORIENTED_EDGE ( 'NONE', *, *, #23636, .F. ) ;
#255 = EDGE_CURVE ( 'NONE', #10831, #25675, #41179, .T. ) ;
#256 = DIRECTION ( 'NONE',  ( -0.000000000000000000, 1.000000000000000000, -0.000000000000000000 ) ) ;
#257 = DIRECTION ( 'NONE',  ( 0.000000000000000000, 0.000000000000000000, 1.000000000000000000 ) ) ;
#258 = ORIENTED_EDGE ( 'NONE', *, *, #35570, .T. ) ;
#259 = EDGE_CURVE ( 'NONE', #12398, #42413, #45266, .T. ) ;
#260 = B_SPLINE_CURVE_WITH_KNOTS ( 'NONE', 3,
 ( #27101, #11365, #15998, #46699 ),
 .UNSPECIFIED., .F., .F.,
 ( 4, 4 ),
 ( 0.1211775127643062860, 0.1625894504277921315 ),
 .UNSPECIFIED. ) ;
#261 = CARTESIAN_POINT ( 'NONE',  ( -1.909347346926324462, 3.267716535433071279, 3.312189666507127188E-16 ) ) ;
#262 = EDGE_CURVE ( 'NONE', #25798, #30055, #28914, .T. ) ;
#263 = EDGE_CURVE ( 'NONE', #7287, #17531, #25669, .T. ) ;
#264 = ORIENTED_EDGE ( 'NONE', *, *, #41294, .T. ) ;
#265 = ORIENTED_EDGE ( 'NONE', *, *, #24485, .F. ) ;
#266 = APPLICATION_PROTOCOL_DEFINITION ( 'draft international standard', 'automotive_design', 1998, #17053 ) ;
#267 = ORIENTED_EDGE ( 'NONE', *, *, #44788, .T. ) ;
#268 = CARTESIAN_POINT ( 'NONE',  ( 0.000000000000000000, 3.346456692913386100, 0.000000000000000000 ) ) ;
#269 = CARTESIAN_POINT ( 'NONE',  ( 1.325491792074624309, 5.905511811023623991, -2.638988599164732385 ) ) ;
#270 = LINE ( 'NONE', #11643, #31070 ) ;
#271 = CARTESIAN_POINT ( 'NONE',  ( -1.909347346926324906, 3.346456692913386100, 1.417322834645662333 ) ) ;
#272 = VERTEX_POINT ( 'NONE', #25412 ) ;
#273 = ORIENTED_EDGE ( 'NONE', *, *, #29883, .F. ) ;
#274 = AXIS2_PLACEMENT_3D ( 'NONE', #47978, #16530, #257 ) ;
#275 =( NAMED_UNIT ( * ) PLANE_ANGLE_UNIT ( ) SI_UNIT ( $, .RADIAN. ) );
#276 = CARTESIAN_POINT ( 'NONE',  ( 0.2727639067037604947, 0.000000000000000000, -1.102362204724405714 ) ) ;
#277 = CIRCLE ( 'NONE', #14412, 2.244934639244525076 ) ;
#278 = ORIENTED_EDGE ( 'NONE', *, *, #17127, .T. ) ;
#279 = CARTESIAN_POINT ( 'NONE',  ( -0.8942052331142547050, 3.267716535433071279, 0.6299212598425164567 ) ) ;
#280 = AXIS2_PLACEMENT_3D ( 'NONE', #27743, #19741, #35252 ) ;
#281 = DIRECTION ( 'NONE',  ( 1.000000000000000000, 0.000000000000000000, -3.469446951953613696E-16 ) ) ;
#282 = AXIS2_PLACEMENT_3D ( 'NONE', #22647, #6901, #3030 ) ;
#283 = CARTESIAN_POINT ( 'NONE',  ( 1.636583440222563635, 3.346456692913386100, -1.259842519685035800 ) ) ;
#284 = CARTESIAN_POINT ( 'NONE',  ( -1.363819533518803473, 3.346456692913386100, -1.102362204724405270 ) ) ;
#285 = VECTOR ( 'NONE', #30019, 39.37007874015748143 ) ;
#286 = VERTEX_POINT ( 'NONE', #38322 ) ;
#287 = LINE ( 'NONE', #43396, #2001 ) ;
#288 = CARTESIAN_POINT ( 'NONE',  ( 1.726519710923990480, 1.205361022782829114E-17, -1.198633063221572481 ) ) ;
#289 = B_SPLINE_CURVE_WITH_KNOTS ( 'NONE', 3,
 ( #15906, #43522, #47625, #4294 ),
 .UNSPECIFIED., .F., .F.,
 ( 4, 4 ),
 ( 2.219256376020187195E-07, 0.002500750338221284681 ),
 .UNSPECIFIED. ) ;
#290 = ORIENTED_EDGE ( 'NONE', *, *, #42530, .T. ) ;
#291 = ORIENTED_EDGE ( 'NONE', *, *, #20423, .T. ) ;
#292 = DIRECTION ( 'NONE',  ( 0.000000000000000000, 0.000000000000000000, -1.000000000000000000 ) ) ;
#293 = DIRECTION ( 'NONE',  ( 1.000000000000000000, -0.000000000000000000, 0.000000000000000000 ) ) ;
#294 = CARTESIAN_POINT ( 'NONE',  ( 1.560669927219591191, 3.267716535433071279, -5.414661521997678257E-16 ) ) ;
#295 = EDGE_CURVE ( 'NONE', #22386, #50303, #6570, .T. ) ;
#296 = ORIENTED_EDGE ( 'NONE', *, *, #48148, .F. ) ;
#297 = ADVANCED_FACE ( 'NONE', ( #22313 ), #38067, .T. ) ;
#298 = EDGE_CURVE ( 'NONE', #1486, #10637, #29549, .T. ) ;
#299 = ORIENTED_EDGE ( 'NONE', *, *, #46894, .F. ) ;
#300 = DIRECTION ( 'NONE',  ( -1.000000000000000000, 0.000000000000000000, -0.000000000000000000 ) ) ;
#301 = ORIENTED_EDGE ( 'NONE', *, *, #1688, .T. ) ;
#302 = DIRECTION ( 'NONE',  ( 1.000000000000000000, -0.000000000000000000, 0.000000000000000000 ) ) ;
#303 = ADVANCED_FACE ( 'NONE', ( #34191 ), #6812, .T. ) ;
#304 = ORIENTED_EDGE ( 'NONE', *, *, #42340, .F. ) ;
#305 = DIRECTION ( 'NONE',  ( 0.000000000000000000, 0.000000000000000000, -1.000000000000000000 ) ) ;
#306 = DIRECTION ( 'NONE',  ( 1.734723475976806848E-16, 0.000000000000000000, 1.000000000000000000 ) ) ;
#307 = CARTESIAN_POINT ( 'NONE',  ( 1.511286805986086890, 0.000000000000000000, 0.8691436966267173103 ) ) ;
#308 = ORIENTED_EDGE ( 'NONE', *, *, #49146, .F. ) ;
#309 = AXIS2_PLACEMENT_3D ( 'NONE', #1939, #49889, #41689 ) ;
#310 = ORIENTED_EDGE ( 'NONE', *, *, #37633, .T. ) ;
#311 = ORIENTED_EDGE ( 'NONE', *, *, #28876, .T. ) ;
#312 = CARTESIAN_POINT ( 'NONE',  ( 2.064489077472676737, 1.642543324816299277, 1.055063358597729595 ) ) ;
#313 = FACE_OUTER_BOUND ( 'NONE', #47009, .T. ) ;
#314 = AXIS2_PLACEMENT_3D ( 'NONE', #49649, #33963, #9444 ) ;
#315 = ORIENTED_EDGE ( 'NONE', *, *, #38294, .T. ) ;
#316 = ORIENTED_EDGE ( 'NONE', *, *, #43835, .F. ) ;
#317 = AXIS2_PLACEMENT_3D ( 'NONE', #5899, #45371, #26286 ) ;
#318 = PLANE ( 'NONE',  #29771 ) ;
#319 = CARTESIAN_POINT ( 'NONE',  ( -0.8182917201112819283, 3.346456692913386100, -1.102362204724405492 ) ) ;
#320 = LINE ( 'NONE', #16074, #3866 ) ;
#321 = EDGE_CURVE ( 'NONE', #39685, #37024, #31709, .T. ) ;
#322 = AXIS2_PLACEMENT_3D ( 'NONE', #49852, #14794, #14539 ) ;
#323 = AXIS2_PLACEMENT_3D ( 'NONE', #40043, #1313, #12678 ) ;
#324 = ORIENTED_EDGE ( 'NONE', *, *, #37835, .F. ) ;
#325 = EDGE_CURVE ( 'NONE', #49197, #2752, #37560, .T. ) ;
#326 = FACE_OUTER_BOUND ( 'NONE', #46204, .T. ) ;
#327 = LINE ( 'NONE', #24338, #15105 ) ;
#328 = CARTESIAN_POINT ( 'NONE',  ( 0.5455278134075211005, 3.267716535433071279, -9.463399047163218249E-17 ) ) ;
#329 = VERTEX_POINT ( 'NONE', #17676 ) ;
#330 = DIRECTION ( 'NONE',  ( -1.000000000000000000, 0.000000000000000000, 1.734723475976806848E-16 ) ) ;
#331 = CARTESIAN_POINT ( 'NONE',  ( -1.636583440222563635, 0.000000000000000000, -4.780733988912460139E-16 ) ) ;
#332 = VECTOR ( 'NONE', #35923, 39.37007874015748143 ) ;
#333 = ORIENTED_EDGE ( 'NONE', *, *, #14896, .T. ) ;
#334 = EDGE_CURVE ( 'NONE', #5779, #3769, #41676, .T. ) ;
#335 = DIRECTION ( 'NONE',  ( 0.08963930890344089242, 0.000000000000000000, -0.9959742939952384022 ) ) ;
#336 = EDGE_LOOP ( 'NONE', ( #16852, #9231, #42778, #18516 ) ) ;
#337 = VERTEX_POINT ( 'NONE', #19683 ) ;
#338 = DIRECTION ( 'NONE',  ( -1.000000000000000000, 0.000000000000000000, 0.000000000000000000 ) ) ;
#339 = DIRECTION ( 'NONE',  ( -0.000000000000000000, -0.000000000000000000, 1.000000000000000000 ) ) ;
#340 = DIRECTION ( 'NONE',  ( -0.01601477604151182663, 0.9998717552508123996, -0.000000000000000000 ) ) ;
#341 = LINE ( 'NONE', #32361, #28589 ) ;
#342 = DIRECTION ( 'NONE',  ( -3.469446951953613696E-16, 0.000000000000000000, -1.000000000000000000 ) ) ;
#343 = ORIENTED_EDGE ( 'NONE', *, *, #20618, .T. ) ;
#344 = VERTEX_POINT ( 'NONE', #8074 ) ;
#345 = ORIENTED_EDGE ( 'NONE', *, *, #38896, .F. ) ;
#346 = LINE ( 'NONE', #44226, #45050 ) ;
#347 = DIRECTION ( 'NONE',  ( 0.9998717552508121775, 0.01601477604151182663, 0.000000000000000000 ) ) ;
#348 = AXIS2_PLACEMENT_3D ( 'NONE', #34135, #23251, #10638 ) ;
#349 = DIRECTION ( 'NONE',  ( 1.000000000000000000, 0.000000000000000000, 0.000000000000000000 ) ) ;
#350 = CARTESIAN_POINT ( 'NONE',  ( 2.436294546427499430, 1.753736851973850319, 1.255140413159070212 ) ) ;
#351 = VERTEX_POINT ( 'NONE', #7572 ) ;
#352 = VECTOR ( 'NONE', #28731, 39.37007874015748143 ) ;
#353 = LINE ( 'NONE', #16108, #2771 ) ;
#354 = CONICAL_SURFACE ( 'NONE', #44060, 2.246510896728926010, 0.01601546068027819014 ) ;
#355 = DIRECTION ( 'NONE',  ( 1.086719731106943413E-16, -1.000000000000000000, 4.078527368698718974E-17 ) ) ;
#356 = VECTOR ( 'NONE', #29132, 39.37007874015748143 ) ;
#357 = VECTOR ( 'NONE', #24500, 39.37007874015748143 ) ;
#358 = VERTEX_POINT ( 'NONE', #39314 ) ;
#359 = DIRECTION ( 'NONE',  ( 0.000000000000000000, 0.000000000000000000, -1.000000000000000000 ) ) ;
#361 = CARTESIAN_POINT ( 'NONE',  ( -0.7697287008055467838, 1.707258635520111145, -2.850711186138116915 ) ) ;
#360 = B_SPLINE_CURVE_WITH_KNOTS ( 'NONE', 3,
 ( #10008, #49206, #49453, #37388 ),
 .UNSPECIFIED., .F., .F.,
 ( 4, 4 ),
 ( 4.362154105138019244E-07, 0.04428848116889361891 ),
 .UNSPECIFIED. ) ;
#362 = DIRECTION ( 'NONE',  ( 1.000000000000000000, 0.000000000000000000, 0.000000000000000000 ) ) ;
#363 = ORIENTED_EDGE ( 'NONE', *, *, #32288, .F. ) ;
#364 = CARTESIAN_POINT ( 'NONE',  ( 1.015142113812069091, 0.000000000000000000, -2.047244094488181343 ) ) ;
#365 = LINE ( 'NONE', #8117, #25832 ) ;
#366 = DIRECTION ( 'NONE',  ( -1.000000000000000000, 0.000000000000000000, 1.734723475976806848E-16 ) ) ;
#367 = EDGE_CURVE ( 'NONE', #7137, #11612, #17764, .T. ) ;
#368 = CIRCLE ( 'NONE', #15223, 2.164630168518208109 ) ;
#369 = EDGE_CURVE ( 'NONE', #14478, #12822, #50374, .T. ) ;
#370 = VERTEX_POINT ( 'NONE', #15572 ) ;
#371 = CARTESIAN_POINT ( 'NONE',  ( 1.091055626815042423, 3.346456692913386100, -1.456692913385822630 ) ) ;
#372 = DIRECTION ( 'NONE',  ( 0.000000000000000000, 0.000000000000000000, 1.000000000000000000 ) ) ;
#373 = VERTEX_POINT ( 'NONE', #11444 ) ;
#374 = DIRECTION ( 'NONE',  ( -3.469446951953613696E-16, 0.000000000000000000, -1.000000000000000000 ) ) ;
#375 = ADVANCED_FACE ( 'NONE', ( #11193 ), #27181, .T. ) ;
#376 = PLANE ( 'NONE',  #43282 ) ;
#377 = DIRECTION ( 'NONE',  ( -1.000000000000000000, 0.000000000000000000, -0.000000000000000000 ) ) ;
#378 = DIRECTION ( 'NONE',  ( 0.000000000000000000, -1.000000000000000000, 0.000000000000000000 ) ) ;
#379 = ORIENTED_EDGE ( 'NONE', *, *, #9138, .F. ) ;
#380 = VERTEX_POINT ( 'NONE', #23559 ) ;
#381 = LINE ( 'NONE', #27740, #4269 ) ;
#382 = CARTESIAN_POINT ( 'NONE',  ( -2.009899395340762673, 3.267716535433071279, 0.6299212598425164567 ) ) ;
#383 = VERTEX_POINT ( 'NONE', #23307 ) ;
#384 = CARTESIAN_POINT ( 'NONE',  ( -2.014664160120487768, 1.577208220393157223, -0.8075893616760145832 ) ) ;
#385 = CARTESIAN_POINT ( 'NONE',  ( 0.4696143004045478797, 0.000000000000000000, 0.2755905511810994302 ) ) ;
#386 = CARTESIAN_POINT ( 'NONE',  ( 0.2508718039770792552, 1.711920121901901348, -2.238407143905190910 ) ) ;
#387 = DIRECTION ( 'NONE',  ( 0.000000000000000000, 0.000000000000000000, 1.000000000000000000 ) ) ;
#388 = VERTEX_POINT ( 'NONE', #31573 ) ;
#389 = ORIENTED_EDGE ( 'NONE', *, *, #38733, .T. ) ;
#390 = EDGE_CURVE ( 'NONE', #6874, #23296, #47017, .T. ) ;
#391 = ORIENTED_EDGE ( 'NONE', *, *, #26902, .T. ) ;
#392 = CARTESIAN_POINT ( 'NONE',  ( 0.000000000000000000, 3.267716535433071279, -0.4724409448818889246 ) ) ;
#393 = CARTESIAN_POINT ( 'NONE',  ( 0.8182917201112824834, 0.000000000000000000, 1.732283464566921172 ) ) ;
#394 = DIRECTION ( 'NONE',  ( 1.000000000000000000, 0.000000000000000000, -3.469446951953613696E-16 ) ) ;
#395 = FACE_BOUND ( 'NONE', #50997, .T. ) ;
#396 = CIRCLE ( 'NONE', #47377, 2.165354330708661568 ) ;
#397 = ORIENTED_EDGE ( 'NONE', *, *, #11216, .T. ) ;
#398 = EDGE_CURVE ( 'NONE', #40889, #2346, #29466, .T. ) ;
#399 = DIRECTION ( 'NONE',  ( 0.9998717552508121775, 0.01601477604151182663, 0.000000000000000000 ) ) ;
#400 = VECTOR ( 'NONE', #34966, 39.37007874015748143 ) ;
#401 = EDGE_LOOP ( 'NONE', ( #7876, #18097, #6204, #3333 ) ) ;
#402 = ORIENTED_EDGE ( 'NONE', *, *, #35422, .F. ) ;
#403 = PLANE ( 'NONE',  #14331 ) ;
#404 = VECTOR ( 'NONE', #48657, 39.37007874015748143 ) ;
#405 = ORIENTED_EDGE ( 'NONE', *, *, #35866, .F. ) ;
#406 = ORIENTED_EDGE ( 'NONE', *, *, #2601, .T. ) ;
#407 = CARTESIAN_POINT ( 'NONE',  ( -1.236813753895213308, 0.000000000000000000, -2.681693691597581974 ) ) ;
#408 = ORIENTED_EDGE ( 'NONE', *, *, #14418, .T. ) ;
#409 = VECTOR ( 'NONE', #23768, 39.37007874015748143 ) ;
#410 = DIRECTION ( 'NONE',  ( 1.734723475976806848E-16, 0.000000000000000000, 1.000000000000000000 ) ) ;
#411 = ADVANCED_FACE ( 'NONE', ( #39062 ), #43172, .T. ) ;
#412 = FACE_OUTER_BOUND ( 'NONE', #31135, .T. ) ;
#413 = CARTESIAN_POINT ( 'NONE',  ( 1.542217245295272932, 0.05262109711011796892, 1.166931937029544564 ) ) ;
#414 = DIRECTION ( 'NONE',  ( 1.000000000000000000, 0.000000000000000000, 0.000000000000000000 ) ) ;
#415 = CARTESIAN_POINT ( 'NONE',  ( 1.398572223930554026, 1.205361022782829114E-17, 1.525996566212370231 ) ) ;
#416 = CARTESIAN_POINT ( 'NONE',  ( 2.168245791271197209, 0.000000000000000000, -2.004968704497248400 ) ) ;
#417 = EDGE_LOOP ( 'NONE', ( #37334, #24980, #11182, #19337 ) ) ;
#418 = PLANE ( 'NONE',  #6868 ) ;
#419 = CARTESIAN_POINT ( 'NONE',  ( -2.919426793319806368, 1.205361022782829114E-17, 0.4451252810446393315 ) ) ;
#420 = CARTESIAN_POINT ( 'NONE',  ( -1.083598637574820334, 1.702374950942735499, 2.747180975113330259 ) ) ;
#421 = VERTEX_POINT ( 'NONE', #7821 ) ;
#422 = LINE ( 'NONE', #4054, #41329 ) ;
#423 = CARTESIAN_POINT ( 'NONE',  ( 0.000000000000000000, 6.692913385826772199, 0.000000000000000000 ) ) ;
#424 = ORIENTED_EDGE ( 'NONE', *, *, #34956, .T. ) ;
#425 = CARTESIAN_POINT ( 'NONE',  ( -1.439733046521776139, 3.346456692913386100, 1.259842519685033357 ) ) ;
#426 = DIRECTION ( 'NONE',  ( -0.9465353838348410376, -0.000000000000000000, -0.3226000110797114795 ) ) ;
#427 = B_SPLINE_CURVE_WITH_KNOTS ( 'NONE', 3,
 ( #1566, #12410, #24028, #20147 ),
 .UNSPECIFIED., .F., .F.,
 ( 4, 4 ),
 ( 5.996436511574133413E-07, 0.0002691799533657123085 ),
 .UNSPECIFIED. ) ;
#428 = CARTESIAN_POINT ( 'NONE',  ( 0.08119777152254364916, 1.623385212329073957, 0.000000000000000000 ) ) ;
#429 = AXIS2_PLACEMENT_3D ( 'NONE', #42019, #14139, #38655 ) ;
#430 = EDGE_CURVE ( 'NONE', #5602, #43368, #11459, .T. ) ;
#431 = CIRCLE ( 'NONE', #50675, 0.3740157480314960647 ) ;
#432 = AXIS2_PLACEMENT_3D ( 'NONE', #48202, #5126, #12360 ) ;
#433 = CARTESIAN_POINT ( 'NONE',  ( -1.503492009532958695, 1.205361022782829114E-17, -0.9334790059352082725 ) ) ;
#434 = EDGE_LOOP ( 'NONE', ( #15887, #17893, #8935, #4099 ) ) ;
#435 = DIRECTION ( 'NONE',  ( -1.000000000000000000, -0.000000000000000000, -0.000000000000000000 ) ) ;
#436 = AXIS2_PLACEMENT_3D ( 'NONE', #1333, #41343, #17090 ) ;
#437 = EDGE_CURVE ( 'NONE', #38725, #38735, #18864, .T. ) ;
#438 = CARTESIAN_POINT ( 'NONE',  ( 1.130720258286322499, 1.729608259214892918, -2.234541341810120763 ) ) ;
#439 = LINE ( 'NONE', #16192, #44064 ) ;
#441 = EDGE_CURVE ( 'NONE', #1296, #33691, #46526, .T. ) ;
#440 = LINE ( 'NONE', #7428, #31738 ) ;
#442 = ORIENTED_EDGE ( 'NONE', *, *, #24074, .F. ) ;
#443 = EDGE_CURVE ( 'NONE', #43528, #17266, #27682, .T. ) ;
#444 = VECTOR ( 'NONE', #22863, 39.37007874015748143 ) ;
#445 = ORIENTED_EDGE ( 'NONE', *, *, #47952, .T. ) ;
#446 = ORIENTED_EDGE ( 'NONE', *, *, #13837, .F. ) ;
#447 = CARTESIAN_POINT ( 'NONE',  ( 1.091055626815042423, 3.267716535433071279, -1.889763779527552368 ) ) ;
#448 = VERTEX_POINT ( 'NONE', #34443 ) ;
#449 = CARTESIAN_POINT ( 'NONE',  ( 2.823445274216730638, 1.205361022782829114E-17, 0.8656477926280680135 ) ) ;
#450 = ORIENTED_EDGE ( 'NONE', *, *, #27909, .T. ) ;
#451 = LINE ( 'NONE', #47138, #47795 ) ;
#452 = EDGE_CURVE ( 'NONE', #19346, #17026, #50131, .T. ) ;
#453 = ORIENTED_EDGE ( 'NONE', *, *, #12794, .F. ) ;
#454 = LINE ( 'NONE', #12073, #27390 ) ;
#455 = CARTESIAN_POINT ( 'NONE',  ( 2.168245791271197209, 1.654581109258766558, -2.004968704497248400 ) ) ;
#456 = VERTEX_POINT ( 'NONE', #30563 ) ;
#457 = EDGE_CURVE ( 'NONE', #27808, #46201, #7070, .T. ) ;
#458 = DIRECTION ( 'NONE',  ( -0.9998717552508122886, -0.01601477604151181275, 0.000000000000000000 ) ) ;
#459 = EDGE_LOOP ( 'NONE', ( #26037, #28525, #7680, #34312 ) ) ;
#460 = LINE ( 'NONE', #199, #37825 ) ;
#461 = B_SPLINE_CURVE_WITH_KNOTS ( 'NONE', 3,
 ( #45919, #19073, #50764, #19573 ),
 .UNSPECIFIED., .F., .F.,
 ( 4, 4 ),
 ( 0.1211873102087489551, 0.1625992483279400380 ),
 .UNSPECIFIED. ) ;
#462 = EDGE_CURVE ( 'NONE', #25931, #40389, #3190, .T. ) ;
#463 = ORIENTED_EDGE ( 'NONE', *, *, #32379, .T. ) ;
#464 = ORIENTED_EDGE ( 'NONE', *, *, #28101, .F. ) ;
#465 = CARTESIAN_POINT ( 'NONE',  ( -1.299838092272570966, 1.592662749112851772, 2.079612685669299577 ) ) ;
#466 = AXIS2_PLACEMENT_3D ( 'NONE', #49592, #32189, #4812 ) ;
#467 = LINE ( 'NONE', #17436, #12190 ) ;
#468 = VECTOR ( 'NONE', #49916, 39.37007874015748143 ) ;
#469 = ORIENTED_EDGE ( 'NONE', *, *, #20201, .F. ) ;
#470 = CARTESIAN_POINT ( 'NONE',  ( -0.3486774197067340486, 3.346456692913386100, 0.1181102362204703021 ) ) ;
#471 = ADVANCED_FACE ( 'NONE', ( #7325 ), #23067, .F. ) ;
#472 = VERTEX_POINT ( 'NONE', #15316 ) ;
#473 = DIRECTION ( 'NONE',  ( -0.9998717552508122886, -0.01601477604151182316, 0.000000000000000000 ) ) ;
#474 = DIRECTION ( 'NONE',  ( -3.986037398843765983E-20, -1.000000000000000000, -1.160734090543304660E-16 ) ) ;
#475 = VECTOR ( 'NONE', #44694, 39.37007874015748143 ) ;
#476 = CARTESIAN_POINT ( 'NONE',  ( 0.4696143004045478797, 3.267716535433071279, -1.629301903132387260E-16 ) ) ;
#477 = ORIENTED_EDGE ( 'NONE', *, *, #24701, .F. ) ;
#478 = ORIENTED_EDGE ( 'NONE', *, *, #43095, .F. ) ;
#479 = VECTOR ( 'NONE', #29669, 39.37007874015748143 ) ;
#480 = CARTESIAN_POINT ( 'NONE',  ( -0.4788131938641533303, 1.613355999311305133, 2.914091152102185944 ) ) ;
#481 = DIRECTION ( 'NONE',  ( -0.000000000000000000, 1.000000000000000000, -0.000000000000000000 ) ) ;
#482 = CARTESIAN_POINT ( 'NONE',  ( 2.576863348864710801, 1.759415398959654819, 1.442554885838449819 ) ) ;
#483 = EDGE_CURVE ( 'NONE', #34071, #17239, #28961, .T. ) ;
#484 = CARTESIAN_POINT ( 'NONE',  ( 0.5455278134075214336, 3.267716535433071279, -9.463399047163224412E-17 ) ) ;
#485 = ADVANCED_FACE ( 'NONE', ( #1346 ), #4459, .F. ) ;
#486 = DIRECTION ( 'NONE',  ( -0.5508969814520945363, 1.288287287306305530E-16, -0.8345732537213079727 ) ) ;
#487 = DIRECTION ( 'NONE',  ( -1.206139481778042838E-16, 1.000000000000000000, 4.526717189434675613E-17 ) ) ;
#488 = ORIENTED_EDGE ( 'NONE', *, *, #2043, .T. ) ;
#489 = CARTESIAN_POINT ( 'NONE',  ( 0.7423782071083085965, 3.267716535433071279, -2.575641807848709701E-16 ) ) ;
#490 = ORIENTED_EDGE ( 'NONE', *, *, #3167, .F. ) ;
#491 = DIRECTION ( 'NONE',  ( -1.000000000000000000, 0.000000000000000000, 1.734723475976806848E-16 ) ) ;
#492 = ORIENTED_EDGE ( 'NONE', *, *, #14114, .F. ) ;
#493 = B_SPLINE_CURVE_WITH_KNOTS ( 'NONE', 3,
 ( #15313, #46275, #23061, #11190 ),
 .UNSPECIFIED., .F., .F.,
 ( 4, 4 ),
 ( 0.001811265126449798602, 0.04538071868018288962 ),
 .UNSPECIFIED. ) ;
#494 = EDGE_CURVE ( 'NONE', #22056, #26109, #32094, .T. ) ;
#495 = CARTESIAN_POINT ( 'NONE',  ( 1.091055626815042423, 0.000000000000000000, -1.771653543307081691 ) ) ;
#496 = CARTESIAN_POINT ( 'NONE',  ( -2.182111253630085290, 3.346456692913386100, -0.5118110236220464460 ) ) ;
#497 = CARTESIAN_POINT ( 'NONE',  ( 2.951990591674675368, 2.755905511811027164, -0.08331184815398351429 ) ) ;
#498 = ORIENTED_EDGE ( 'NONE', *, *, #40681, .F. ) ;
#499 = VECTOR ( 'NONE', #35723, 39.37007874015748143 ) ;
#500 = ADVANCED_FACE ( 'NONE', ( #586 ), #24337, .T. ) ;
#501 = ADVANCED_FACE ( 'NONE', ( #36470 ), #20194, .F. ) ;
#502 = AXIS2_PLACEMENT_3D ( 'NONE', #14889, #10510, #7397 ) ;
#503 = CARTESIAN_POINT ( 'NONE',  ( 0.000000000000000000, 1.574803149606302854, 0.000000000000000000 ) ) ;
#504 = VECTOR ( 'NONE', #27260, 39.37007874015748143 ) ;
#505 = ORIENTED_EDGE ( 'NONE', *, *, #14114, .T. ) ;
#506 = PLANE ( 'NONE',  #7292 ) ;
#507 = AXIS2_PLACEMENT_3D ( 'NONE', #24841, #32864, #13735 ) ;
#508 = VERTEX_POINT ( 'NONE', #40596 ) ;
#509 = FACE_OUTER_BOUND ( 'NONE', #36357, .T. ) ;
#510 = DIRECTION ( 'NONE',  ( 1.734723475976806848E-16, -0.000000000000000000, 1.000000000000000000 ) ) ;
#511 = VECTOR ( 'NONE', #44704, 39.37007874015748143 ) ;
#512 = CIRCLE ( 'NONE', #29375, 1.743387098533651480 ) ;
#513 = DIRECTION ( 'NONE',  ( 0.000000000000000000, -1.000000000000000000, 0.000000000000000000 ) ) ;
#514 = VERTEX_POINT ( 'NONE', #17105 ) ;
#515 = EDGE_LOOP ( 'NONE', ( #4866, #26370, #10701, #21871 ) ) ;
#516 = DIRECTION ( 'NONE',  ( 0.000000000000000000, 1.000000000000000000, 0.000000000000000000 ) ) ;
#517 = FACE_OUTER_BOUND ( 'NONE', #33825, .T. ) ;
#518 = FACE_BOUND ( 'NONE', #10209, .T. ) ;
#519 = CARTESIAN_POINT ( 'NONE',  ( -1.091055626815042645, 0.000000000000000000, -1.141732283464563569 ) ) ;
#520 = CARTESIAN_POINT ( 'NONE',  ( -0.2727639067037608278, 3.346456692913386100, -0.3543307086614175816 ) ) ;
#521 = EDGE_CURVE ( 'NONE', #50302, #42898, #4716, .T. ) ;
#522 = ORIENTED_EDGE ( 'NONE', *, *, #13187, .F. ) ;
#523 = B_SPLINE_CURVE_WITH_KNOTS ( 'NONE', 3,
 ( #40639, #632, #12248, #8379 ),
 .UNSPECIFIED., .F., .F.,
 ( 4, 4 ),
 ( 2.008317238951771178E-07, 0.002500501625894326844 ),
 .UNSPECIFIED. ) ;
#524 = LINE ( 'NONE', #261, #38940 ) ;
#525 = ORIENTED_EDGE ( 'NONE', *, *, #1312, .T. ) ;
#526 = ORIENTED_EDGE ( 'NONE', *, *, #1137, .T. ) ;
#527 = EDGE_CURVE ( 'NONE', #43386, #26232, #48549, .T. ) ;
#528 = VERTEX_POINT ( 'NONE', #4968 ) ;
#529 = CARTESIAN_POINT ( 'NONE',  ( 2.016369045219287948, 1.641772594434526278, 1.140940039539855677 ) ) ;
#530 = CARTESIAN_POINT ( 'NONE',  ( 1.636583440222563857, 3.267716535433071279, 1.062992125984245639 ) ) ;
#531 = EDGE_CURVE ( 'NONE', #42180, #16004, #35958, .T. ) ;
#532 = EDGE_CURVE ( 'NONE', #19885, #12012, #8584, .T. ) ;
#534 = CARTESIAN_POINT ( 'NONE',  ( 1.363819533518803251, 3.267716535433071279, -0.9842519685039348154 ) ) ;
#533 = CIRCLE ( 'NONE', #35177, 2.165354330708661568 ) ;
#535 = CARTESIAN_POINT ( 'NONE',  ( -0.3486774197067339376, 0.000000000000000000, -1.574803149606293529 ) ) ;
#536 = VERTEX_POINT ( 'NONE', #16595 ) ;
#537 = EDGE_LOOP ( 'NONE', ( #46849, #11263, #38337, #299, #6692, #44475, #50981, #44812, #28640, #30920, #31824, #49047, #11727 ) ) ;
#539 = VECTOR ( 'NONE', #22638, 39.37007874015748143 ) ;
#538 = CARTESIAN_POINT ( 'NONE',  ( 2.105931235793975009, 3.346456692913386100, -0.03937007874015936021 ) ) ;
#540 = DIRECTION ( 'NONE',  ( -1.000000000000000000, 0.000000000000000000, 0.000000000000000000 ) ) ;
#541 = VECTOR ( 'NONE', #22838, 39.37007874015748143 ) ;
#542 = DIRECTION ( 'NONE',  ( 1.734723475976806848E-16, -0.000000000000000000, 1.000000000000000000 ) ) ;
#543 = EDGE_LOOP ( 'NONE', ( #45689, #18327, #18038, #46018 ) ) ;
#544 = CARTESIAN_POINT ( 'NONE',  ( 0.2727639067037604392, 3.346456692913386100, 0.5905511811023579360 ) ) ;
#545 = DIRECTION ( 'NONE',  ( -1.000000000000000000, 0.000000000000000000, 0.000000000000000000 ) ) ;
#546 = DIRECTION ( 'NONE',  ( -0.000000000000000000, 1.000000000000000000, -0.000000000000000000 ) ) ;
#547 = AXIS2_PLACEMENT_3D ( 'NONE', #36809, #1941, #6065 ) ;
#548 = EDGE_CURVE ( 'NONE', #767, #17945, #12977, .T. ) ;
#549 = DIRECTION ( 'NONE',  ( -1.000000000000000000, 0.000000000000000000, 1.734723475976806848E-16 ) ) ;
#550 = CARTESIAN_POINT ( 'NONE',  ( 1.281152772984937682, 0.000000000000000000, -2.660341145381147854 ) ) ;
#551 = VECTOR ( 'NONE', #583, 39.37007874015748143 ) ;
#552 = VERTEX_POINT ( 'NONE', #12717 ) ;
#553 = DIRECTION ( 'NONE',  ( -0.000000000000000000, 1.000000000000000000, -0.000000000000000000 ) ) ;
#554 = DIRECTION ( 'NONE',  ( 0.04486483035051863633, 1.159547425261732707E-16, -0.9989930665413144784 ) ) ;
#555 = ORIENTED_EDGE ( 'NONE', *, *, #24551, .F. ) ;
#557 = ORIENTED_EDGE ( 'NONE', *, *, #2112, .T. ) ;
#556 = EDGE_CURVE ( 'NONE', #30179, #17684, #28446, .T. ) ;
#558 = CARTESIAN_POINT ( 'NONE',  ( -1.997023710742784619, 0.5251151982619056691, -0.8000494717651052134 ) ) ;
#559 = LINE ( 'NONE', #39798, #12175 ) ;
#560 = CARTESIAN_POINT ( 'NONE',  ( 2.160407304981128984, 1.574803149606302854, -0.1462862061266585745 ) ) ;
#561 = ORIENTED_EDGE ( 'NONE', *, *, #22890, .T. ) ;
#562 = ADVANCED_FACE ( 'NONE', ( #47529 ), #16853, .F. ) ;
#563 = EDGE_CURVE ( 'NONE', #34643, #7408, #50346, .T. ) ;
#564 = EDGE_CURVE ( 'NONE', #23735, #472, #44698, .T. ) ;
#565 = ORIENTED_EDGE ( 'NONE', *, *, #39222, .T. ) ;
#566 = CARTESIAN_POINT ( 'NONE',  ( -1.985260859929297794, 3.267716535433071279, -0.1968503937007880511 ) ) ;
#567 = ORIENTED_EDGE ( 'NONE', *, *, #25329, .F. ) ;
#568 = DIRECTION ( 'NONE',  ( -0.01601477604151182663, 0.9998717552508123996, -0.000000000000000000 ) ) ;
#569 = EDGE_LOOP ( 'NONE', ( #16128, #15928, #15236, #39581 ) ) ;
#570 = CARTESIAN_POINT ( 'NONE',  ( 0.6504488014449565370, 1.685511682479523099, -2.171864155587596379 ) ) ;
#571 = CARTESIAN_POINT ( 'NONE',  ( -2.076656781855024114, 1.674640491952791077, 0.6230015025396302697 ) ) ;
#572 = DIRECTION ( 'NONE',  ( -3.469446951953613696E-16, 0.000000000000000000, -1.000000000000000000 ) ) ;
#573 = AXIS2_PLACEMENT_3D ( 'NONE', #35731, #27978, #16888 ) ;
#574 = ORIENTED_EDGE ( 'NONE', *, *, #10396, .F. ) ;
#575 = VERTEX_POINT ( 'NONE', #19929 ) ;
#576 = ORIENTED_EDGE ( 'NONE', *, *, #30302, .T. ) ;
#577 = CARTESIAN_POINT ( 'NONE',  ( -0.8952071785065484066, 0.000000000000000000, 1.972340328593134906 ) ) ;
#578 = DIRECTION ( 'NONE',  ( 0.000000000000000000, 0.000000000000000000, -1.000000000000000000 ) ) ;
#579 = ORIENTED_EDGE ( 'NONE', *, *, #21790, .T. ) ;
#580 = ORIENTED_EDGE ( 'NONE', *, *, #12029, .F. ) ;
#581 = DIRECTION ( 'NONE',  ( 0.7227948638273978821, 0.000000000000000000, -0.6910626489868580968 ) ) ;
#582 = FACE_OUTER_BOUND ( 'NONE', #22566, .T. ) ;
#583 = DIRECTION ( 'NONE',  ( 0.000000000000000000, 0.000000000000000000, -1.000000000000000000 ) ) ;
#584 = B_SPLINE_CURVE_WITH_KNOTS ( 'NONE', 3,
 ( #9122, #44230, #350, #4485 ),
 .UNSPECIFIED., .F., .F.,
 ( 4, 4 ),
 ( 0.01454276592102258202, 0.03074978739352322854 ),
 .UNSPECIFIED. ) ;
#585 = ORIENTED_EDGE ( 'NONE', *, *, #50532, .T. ) ;
#586 = FACE_OUTER_BOUND ( 'NONE', #32840, .T. ) ;
#587 = CARTESIAN_POINT ( 'NONE',  ( 1.091055626815042645, 3.267716535433071279, 0.9448818897637746295 ) ) ;
#588 = VECTOR ( 'NONE', #9109, 39.37007874015748143 ) ;
#589 = PLANE ( 'NONE',  #36074 ) ;
#590 = ORIENTED_EDGE ( 'NONE', *, *, #45368, .T. ) ;
#591 = DIRECTION ( 'NONE',  ( -0.000000000000000000, 1.000000000000000000, -0.000000000000000000 ) ) ;
#592 = DIRECTION ( 'NONE',  ( -1.000000000000000000, -0.000000000000000000, -0.000000000000000000 ) ) ;
#593 = ORIENTED_EDGE ( 'NONE', *, *, #32954, .T. ) ;
#594 = CARTESIAN_POINT ( 'NONE',  ( 2.078610245214651098, 0.000000000000000000, -0.4912784290244630592 ) ) ;
#595 = ORIENTED_EDGE ( 'NONE', *, *, #18040, .T. ) ;
#596 = VERTEX_POINT ( 'NONE', #35698 ) ;
#597 = DIRECTION ( 'NONE',  ( 0.000000000000000000, 0.000000000000000000, 1.000000000000000000 ) ) ;
#598 = CARTESIAN_POINT ( 'NONE',  ( -1.909347346926324462, 3.346456692913386100, 0.7874015748031456541 ) ) ;
#599 = DIRECTION ( 'NONE',  ( -1.000000000000000000, 0.000000000000000000, 1.734723475976806848E-16 ) ) ;
#600 = ADVANCED_FACE ( 'NONE', ( #326 ), #16077, .F. ) ;
#601 = DIRECTION ( 'NONE',  ( -1.000000000000000000, 0.000000000000000000, -0.000000000000000000 ) ) ;
#602 = CARTESIAN_POINT ( 'NONE',  ( 0.08139965876239094178, 1.610780518492231694, 0.000000000000000000 ) ) ;
#603 = ORIENTED_EDGE ( 'NONE', *, *, #42287, .T. ) ;
#605 = EDGE_CURVE ( 'NONE', #10001, #15411, #43680, .T. ) ;
#604 = ORIENTED_EDGE ( 'NONE', *, *, #14891, .T. ) ;
#606 = VERTEX_POINT ( 'NONE', #5983 ) ;
#607 = CARTESIAN_POINT ( 'NONE',  ( -0.07591351300297333182, 0.000000000000000000, -0.1574803149606301411 ) ) ;
#608 = DIRECTION ( 'NONE',  ( -0.000000000000000000, 1.000000000000000000, -0.000000000000000000 ) ) ;
#609 = VECTOR ( 'NONE', #21997, 39.37007874015748143 ) ;
#610 = AXIS2_PLACEMENT_3D ( 'NONE', #25837, #13461, #17336 ) ;
#611 = DIRECTION ( 'NONE',  ( -0.000000000000000000, 1.000000000000000000, -0.000000000000000000 ) ) ;
#612 = DIRECTION ( 'NONE',  ( 0.000000000000000000, 0.000000000000000000, -1.000000000000000000 ) ) ;
#613 = FACE_OUTER_BOUND ( 'NONE', #23764, .T. ) ;
#614 = AXIS2_PLACEMENT_3D ( 'NONE', #23088, #14843, #31348 ) ;
#615 = ORIENTED_EDGE ( 'NONE', *, *, #28454, .T. ) ;
#616 = DIRECTION ( 'NONE',  ( 0.9998717552508121775, 0.01601477604151182663, 0.000000000000000000 ) ) ;
#617 = EDGE_CURVE ( 'NONE', #42860, #2302, #45709, .T. ) ;
#618 = CARTESIAN_POINT ( 'NONE',  ( 0.002207914879453961969, 6.692913385826772199, 0.04916304461325451958 ) ) ;
#619 = VERTEX_POINT ( 'NONE', #33625 ) ;
#620 = CARTESIAN_POINT ( 'NONE',  ( 0.2727639067037604947, 0.000000000000000000, 0.4724409448818868706 ) ) ;
#621 = EDGE_CURVE ( 'NONE', #43980, #50349, #21739, .T. ) ;
#622 = PLANE ( 'NONE',  #40169 ) ;
#623 = CARTESIAN_POINT ( 'NONE',  ( 0.000000000000000000, 3.267716535433071279, 0.4330708661417290162 ) ) ;
#624 = ORIENTED_EDGE ( 'NONE', *, *, #34860, .F. ) ;
#625 = CARTESIAN_POINT ( 'NONE',  ( -3.927031490892378253E-16, 0.000000000000000000, -2.204724409448811429 ) ) ;
#626 = CARTESIAN_POINT ( 'NONE',  ( 1.836694934015037806, 1.638894784719147513, 1.401770057403159520 ) ) ;
#627 = EDGE_CURVE ( 'NONE', #37376, #24669, #34123, .T. ) ;
#628 = DIRECTION ( 'NONE',  ( 0.000000000000000000, -1.000000000000000000, 0.000000000000000000 ) ) ;
#629 = EDGE_CURVE ( 'NONE', #27835, #12857, #13991, .T. ) ;
#630 = ORIENTED_EDGE ( 'NONE', *, *, #20994, .T. ) ;
#631 = FACE_OUTER_BOUND ( 'NONE', #6545, .T. ) ;
#632 = CARTESIAN_POINT ( 'NONE',  ( 0.2483449720100243119, 1.624673919087268770, -2.942339427351925440 ) ) ;
#633 = ORIENTED_EDGE ( 'NONE', *, *, #12188, .F. ) ;
#634 = CIRCLE ( 'NONE', #36092, 2.106299212598425008 ) ;
#635 = CARTESIAN_POINT ( 'NONE',  ( -2.633944868634075398, 1.674114007166422002, -0.5507025360789752355 ) ) ;
#636 = DIRECTION ( 'NONE',  ( -1.000000000000000000, 0.000000000000000000, -0.000000000000000000 ) ) ;
#637 = LINE ( 'NONE', #27992, #779 ) ;
#638 = FACE_OUTER_BOUND ( 'NONE', #44764, .T. ) ;
#639 = ORIENTED_EDGE ( 'NONE', *, *, #2477, .F. ) ;
#640 = VERTEX_POINT ( 'NONE', #9609 ) ;
#641 = DIRECTION ( 'NONE',  ( -0.000000000000000000, 0.000000000000000000, 1.000000000000000000 ) ) ;
#642 = DIRECTION ( 'NONE',  ( 0.000000000000000000, 0.000000000000000000, -1.000000000000000000 ) ) ;
#643 = VERTEX_POINT ( 'NONE', #33120 ) ;
#644 = LINE ( 'NONE', #36784, #6080 ) ;
#645 = CARTESIAN_POINT ( 'NONE',  ( 0.5756566573088586214, 1.205361022782829114E-17, 2.896516654582643291 ) ) ;
#646 = CARTESIAN_POINT ( 'NONE',  ( 1.833791099076603537, 6.692913385826772199, -1.151507526013693772 ) ) ;
#647 = LINE ( 'NONE', #5284, #38047 ) ;
#648 = ORIENTED_EDGE ( 'NONE', *, *, #37358, .T. ) ;
#649 = ORIENTED_EDGE ( 'NONE', *, *, #23937, .T. ) ;
#650 = DIRECTION ( 'NONE',  ( 0.000000000000000000, 0.000000000000000000, 1.000000000000000000 ) ) ;
#651 = CARTESIAN_POINT ( 'NONE',  ( 0.1067246931122726866, 0.02962905676920215767, 0.000000000000000000 ) ) ;
#652 = VECTOR ( 'NONE', #39363, 39.37007874015748143 ) ;
#653 = VECTOR ( 'NONE', #28879, 39.37007874015748143 ) ;
#654 = CARTESIAN_POINT ( 'NONE',  ( -0.7381027496704857249, 1.531192278308824539, -2.859439394060923068 ) ) ;
#655 = CARTESIAN_POINT ( 'NONE',  ( 3.937007874015748143, 2.913385826771657250, -1.023622047244094224 ) ) ;
#656 = FACE_BOUND ( 'NONE', #18999, .T. ) ;
#657 = ORIENTED_EDGE ( 'NONE', *, *, #15041, .F. ) ;
#658 = CARTESIAN_POINT ( 'NONE',  ( -2.122484638469143814, 1.673906474958827939, -0.4339650761337435214 ) ) ;
#659 = ORIENTED_EDGE ( 'NONE', *, *, #49999, .F. ) ;
#660 = VERTEX_POINT ( 'NONE', #17606 ) ;
#661 = CYLINDRICAL_SURFACE ( 'NONE', #36600, 2.164630168518208109 ) ;
#662 = ORIENTED_EDGE ( 'NONE', *, *, #5685, .T. ) ;
#663 = ORIENTED_EDGE ( 'NONE', *, *, #6430, .F. ) ;
#664 = PLANE ( 'NONE',  #11276 ) ;
#665 = AXIS2_PLACEMENT_3D ( 'NONE', #3326, #47156, #19067 ) ;
#666 = ORIENTED_EDGE ( 'NONE', *, *, #47141, .F. ) ;
#667 = ADVANCED_FACE ( 'NONE', ( #17359 ), #5675, .T. ) ;
#668 = EDGE_CURVE ( 'NONE', #49945, #20320, #44427, .T. ) ;
#670 = CARTESIAN_POINT ( 'NONE',  ( 2.153610746787201435, 1.643970771453353130, -0.8669779829368272628 ) ) ;
#669 = VECTOR ( 'NONE', #48578, 39.37007874015748143 ) ;
#671 = CARTESIAN_POINT ( 'NONE',  ( -2.164823134740036181, 1.673228346456695492, 0.000000000000000000 ) ) ;
#672 = ADVANCED_FACE ( 'NONE', ( #21483 ), #10651, .T. ) ;
#673 = CARTESIAN_POINT ( 'NONE',  ( -1.363819533518803029, 3.267716535433071279, 0.2755905511810996522 ) ) ;
#674 = LINE ( 'NONE', #20018, #15684 ) ;
#675 = LINE ( 'NONE', #152, #6376 ) ;
#676 = DIRECTION ( 'NONE',  ( -0.7071067811865481278, 0.7071067811865469066, 4.592716591420704405E-16 ) ) ;
#677 = EDGE_LOOP ( 'NONE', ( #44248, #22228, #9359, #47883 ) ) ;
#678 = CARTESIAN_POINT ( 'NONE',  ( 0.000000000000000000, 0.000000000000000000, 0.000000000000000000 ) ) ;
#679 = LINE ( 'NONE', #22028, #24389 ) ;
#680 = CARTESIAN_POINT ( 'NONE',  ( -0.3486774197067334380, 3.346456692913386100, 0.6299212598425164567 ) ) ;
#681 = VERTEX_POINT ( 'NONE', #37751 ) ;
#682 = DIRECTION ( 'NONE',  ( -1.000000000000000000, -0.000000000000000000, -0.000000000000000000 ) ) ;
#683 = ADVANCED_FACE ( 'NONE', ( #25859 ), #33375, .F. ) ;
#684 = EDGE_CURVE ( 'NONE', #20090, #19616, #6245, .T. ) ;
#685 = CARTESIAN_POINT ( 'NONE',  ( -3.927031490892378253E-16, 3.346456692913386100, -1.889763779527552146 ) ) ;
#686 = ORIENTED_EDGE ( 'NONE', *, *, #5220, .F. ) ;
#687 = DIRECTION ( 'NONE',  ( -0.000000000000000000, 1.000000000000000000, -0.000000000000000000 ) ) ;
#688 = VECTOR ( 'NONE', #36333, 39.37007874015748143 ) ;
#689 = PLANE ( 'NONE',  #22633 ) ;
#690 = DIRECTION ( 'NONE',  ( -3.469446951953613696E-16, 0.000000000000000000, -1.000000000000000000 ) ) ;
#691 = EDGE_CURVE ( 'NONE', #38575, #28934, #17862, .T. ) ;
#692 = ORIENTED_EDGE ( 'NONE', *, *, #46921, .F. ) ;
#693 = AXIS2_PLACEMENT_3D ( 'NONE', #4212, #47029, #7581 ) ;
#694 = CARTESIAN_POINT ( 'NONE',  ( -0.2727639067037608278, 3.346456692913386100, -0.03937007874015908959 ) ) ;
#695 = VERTEX_POINT ( 'NONE', #29482 ) ;
#696 = CARTESIAN_POINT ( 'NONE',  ( -0.8182917201112819283, 0.000000000000000000, -2.047244094488181343 ) ) ;
#697 = CARTESIAN_POINT ( 'NONE',  ( 0.000000000000000000, 3.267716535433071279, -1.259842519685035134 ) ) ;
#698 = CIRCLE ( 'NONE', #5637, 1.682967650661292502 ) ;
#699 = VECTOR ( 'NONE', #17087, 39.37007874015748143 ) ;
#700 = CARTESIAN_POINT ( 'NONE',  ( 1.015142113812069757, 3.267716535433071279, -3.521981712565034361E-16 ) ) ;
#701 = LINE ( 'NONE', #16453, #21905 ) ;
#702 = VECTOR ( 'NONE', #26815, 39.37007874015748143 ) ;
#703 = ORIENTED_EDGE ( 'NONE', *, *, #26447, .T. ) ;
#704 = ORIENTED_EDGE ( 'NONE', *, *, #29300, .T. ) ;
#705 = CARTESIAN_POINT ( 'NONE',  ( -0.8182917201112819283, 0.000000000000000000, -0.03937007874015895081 ) ) ;
#706 = VERTEX_POINT ( 'NONE', #45202 ) ;
#707 = VECTOR ( 'NONE', #10273, 39.37007874015748143 ) ;
#708 = CARTESIAN_POINT ( 'NONE',  ( -0.6214413264104945434, 3.267716535433071279, 0.1574803149606285035 ) ) ;
#709 = ADVANCED_FACE ( 'NONE', ( #44955 ), #29989, .F. ) ;
#710 = ORIENTED_EDGE ( 'NONE', *, *, #41702, .F. ) ;
#711 = DIRECTION ( 'NONE',  ( 0.000000000000000000, 1.000000000000000000, 0.000000000000000000 ) ) ;
#712 = AXIS2_PLACEMENT_3D ( 'NONE', #34837, #11341, #39468 ) ;
#713 = VERTEX_POINT ( 'NONE', #41112 ) ;
#714 = DIRECTION ( 'NONE',  ( 1.000000000000000000, 0.000000000000000000, -3.469446951953613696E-16 ) ) ;
#715 = CARTESIAN_POINT ( 'NONE',  ( -2.823445274216742629, 5.905511811023623991, 0.8656477926280273794 ) ) ;
#716 = ORIENTED_EDGE ( 'NONE', *, *, #82, .F. ) ;
#717 = CARTESIAN_POINT ( 'NONE',  ( 0.1968503937007878291, 3.267716535433071279, 2.097080421798980687 ) ) ;
#718 = ORIENTED_EDGE ( 'NONE', *, *, #12741, .F. ) ;
#719 = CARTESIAN_POINT ( 'NONE',  ( -2.823445274216743073, 1.675250974312822105, 0.8656477926280276014 ) ) ;
#720 = AXIS2_PLACEMENT_3D ( 'NONE', #26978, #18743, #30872 ) ;
#721 = VERTEX_POINT ( 'NONE', #45453 ) ;
#722 = EDGE_LOOP ( 'NONE', ( #32212, #14805, #21294, #41586 ) ) ;
#723 = DIRECTION ( 'NONE',  ( 1.000000000000000000, 0.000000000000000000, 0.000000000000000000 ) ) ;
#724 = EDGE_CURVE ( 'NONE', #34623, #508, #49561, .T. ) ;
#725 = CARTESIAN_POINT ( 'NONE',  ( -0.6214413264104939882, 0.000000000000000000, 1.417322834645662777 ) ) ;
#726 = EDGE_LOOP ( 'NONE', ( #49248, #34876, #20386, #6495 ) ) ;
#727 = DIRECTION ( 'NONE',  ( -0.000000000000000000, 0.000000000000000000, 1.000000000000000000 ) ) ;
#728 = VERTEX_POINT ( 'NONE', #22249 ) ;
#729 = CARTESIAN_POINT ( 'NONE',  ( 1.091055626815043311, 0.000000000000000000, 1.574803149606291974 ) ) ;
#730 = EDGE_CURVE ( 'NONE', #2835, #49324, #10628, .T. ) ;
#731 = FACE_OUTER_BOUND ( 'NONE', #28856, .T. ) ;
#732 = AXIS2_PLACEMENT_3D ( 'NONE', #19178, #34942, #50622 ) ;
#733 = VECTOR ( 'NONE', #35619, 39.37007874015748143 ) ;
#734 = EDGE_CURVE ( 'NONE', #39696, #36547, #5477, .T. ) ;
#735 = EDGE_CURVE ( 'NONE', #421, #8195, #12268, .T. ) ;
#736 = CARTESIAN_POINT ( 'NONE',  ( 0.000000000000000000, 2.755905511811023612, 0.000000000000000000 ) ) ;
#737 = MECHANICAL_DESIGN_GEOMETRIC_PRESENTATION_REPRESENTATION (  '', ( #7343 ), #48493 ) ;
#738 = ORIENTED_EDGE ( 'NONE', *, *, #7376, .T. ) ;
#739 = VERTEX_POINT ( 'NONE', #34624 ) ;
#740 = LINE ( 'NONE', #12610, #44243 ) ;
#741 = DIRECTION ( 'NONE',  ( -0.000000000000000000, -1.000000000000000000, 0.000000000000000000 ) ) ;
#742 = DIRECTION ( 'NONE',  ( 0.000000000000000000, 0.000000000000000000, -1.000000000000000000 ) ) ;
#743 = CARTESIAN_POINT ( 'NONE',  ( 1.636583440222563857, 3.346456692913386100, -0.8267716535433055070 ) ) ;
#744 = VECTOR ( 'NONE', #32906, 39.37007874015748143 ) ;
#745 = LINE ( 'NONE', #4613, #42478 ) ;
#746 = CARTESIAN_POINT ( 'NONE',  ( -2.356822886370966152, 1.674349844980132174, -0.5884076361977262914 ) ) ;
#747 = CARTESIAN_POINT ( 'NONE',  ( 2.378961647330872786, 3.346456692913386100, 0.6299212598425161236 ) ) ;
#748 = ADVANCED_FACE ( 'NONE', ( #7753 ), #38752, .T. ) ;
#749 = EDGE_LOOP ( 'NONE', ( #24155, #3982, #6135, #40516 ) ) ;
#750 = DIRECTION ( 'NONE',  ( 0.01601477604151182663, -0.9998717552508123996, 0.000000000000000000 ) ) ;
#751 = ORIENTED_EDGE ( 'NONE', *, *, #2533, .F. ) ;
#752 = CARTESIAN_POINT ( 'NONE',  ( 1.833433833923351353, 3.346456692913386100, 0.6299212598425164567 ) ) ;
#753 = ADVANCED_FACE ( 'NONE', ( #39247 ), #7507, .F. ) ;
#754 = ORIENTED_EDGE ( 'NONE', *, *, #8323, .F. ) ;
#755 = FACE_OUTER_BOUND ( 'NONE', #21219, .T. ) ;
#756 = DIRECTION ( 'NONE',  ( -0.8584487936018655452, 5.956818571996926923E-17, -0.5128992774059071280 ) ) ;
#757 = CARTESIAN_POINT ( 'NONE',  ( -1.363819533518803473, 3.346456692913386100, -0.7874015748031470974 ) ) ;
#758 = CARTESIAN_POINT ( 'NONE',  ( 1.181102362204724532, 0.4724409448818893686, 1.181102362204724088 ) ) ;
#759 = AXIS2_PLACEMENT_3D ( 'NONE', #23299, #32085, #43422 ) ;
#760 = EDGE_LOOP ( 'NONE', ( #34527, #20006, #15993, #48619 ) ) ;
#761 = EDGE_CURVE ( 'NONE', #2304, #42940, #15253, .T. ) ;
#762 = CARTESIAN_POINT ( 'NONE',  ( 0.04921259842519603439, 6.692913385826772199, -2.165433070866142007 ) ) ;
#763 = FACE_BOUND ( 'NONE', #51044, .T. ) ;
#764 = EDGE_LOOP ( 'NONE', ( #27424, #28236, #25997, #41547, #30427 ) ) ;
#765 = CARTESIAN_POINT ( 'NONE',  ( -1.091055626815042645, 3.267716535433071279, -0.1968503937007881899 ) ) ;
#766 = EDGE_CURVE ( 'NONE', #14307, #38168, #3376, .T. ) ;
#767 = VERTEX_POINT ( 'NONE', #19117 ) ;
#768 = VECTOR ( 'NONE', #44218, 39.37007874015748143 ) ;
#769 = DIRECTION ( 'NONE',  ( 0.9998717552508121775, 0.01601477604151182663, 0.000000000000000000 ) ) ;
#770 = PLANE ( 'NONE',  #4978 ) ;
#771 = VECTOR ( 'NONE', #44811, 39.37007874015748143 ) ;
#772 = DIRECTION ( 'NONE',  ( 0.5877852522924802425, 0.000000000000000000, -0.8090169943749422332 ) ) ;
#773 = EDGE_LOOP ( 'NONE', ( #73, #46389, #9582, #33616 ) ) ;
#774 = ORIENTED_EDGE ( 'NONE', *, *, #6256, .F. ) ;
#775 = ADVANCED_FACE ( 'NONE', ( #42612 ), #18880, .F. ) ;
#776 = CARTESIAN_POINT ( 'NONE',  ( 0.000000000000000000, 3.267716535433071279, -0.03937007874015908959 ) ) ;
#777 = CARTESIAN_POINT ( 'NONE',  ( 0.000000000000000000, 3.267716535433071279, -1.732283464566922726 ) ) ;
#778 = FACE_BOUND ( 'NONE', #45683, .T. ) ;
#779 = VECTOR ( 'NONE', #11048, 39.37007874015748143 ) ;
#780 = DIRECTION ( 'NONE',  ( -0.9998717552508121775, -0.01601477604151182316, 0.000000000000000000 ) ) ;
#781 = FACE_OUTER_BOUND ( 'NONE', #19671, .T. ) ;
#782 = VERTEX_POINT ( 'NONE', #38996 ) ;
#783 = LINE ( 'NONE', #9040, #21665 ) ;
#784 = VERTEX_POINT ( 'NONE', #3126 ) ;
#785 = ORIENTED_EDGE ( 'NONE', *, *, #39839, .F. ) ;
#786 = ORIENTED_EDGE ( 'NONE', *, *, #50838, .T. ) ;
#787 = LINE ( 'NONE', #32039, #20183 ) ;
#788 = EDGE_CURVE ( 'NONE', #7202, #3538, #7003, .T. ) ;
#789 = PLANE ( 'NONE',  #29930 ) ;
#790 = VECTOR ( 'NONE', #14937, 39.37007874015748143 ) ;
#791 = CARTESIAN_POINT ( 'NONE',  ( -0.6214413264104945434, 0.000000000000000000, -1.732283464566922726 ) ) ;
#792 = EDGE_CURVE ( 'NONE', #30522, #28465, #1468, .T. ) ;
#793 = LINE ( 'NONE', #16546, #46934 ) ;
#794 = EDGE_LOOP ( 'NONE', ( #25554, #27544, #44506, #46711 ) ) ;
#795 = VERTEX_POINT ( 'NONE', #46708 ) ;
#796 = CARTESIAN_POINT ( 'NONE',  ( 0.9836083787002617429, 6.692913385826772199, -1.929060376159698276 ) ) ;
#797 = DIRECTION ( 'NONE',  ( 1.000000000000000000, 0.000000000000000000, -3.469446951953613696E-16 ) ) ;
#798 = B_SPLINE_CURVE_WITH_KNOTS ( 'NONE', 3,
 ( #25877, #2890, #34641, #26132 ),
 .UNSPECIFIED., .F., .F.,
 ( 4, 4 ),
 ( 3.578153648618482699E-07, 0.05018484914549597997 ),
 .UNSPECIFIED. ) ;
#799 = DIRECTION ( 'NONE',  ( 1.734723475976806848E-16, -0.000000000000000000, 1.000000000000000000 ) ) ;
#800 = FACE_OUTER_BOUND ( 'NONE', #7712, .T. ) ;
#801 = CARTESIAN_POINT ( 'NONE',  ( -3.051175669084205122, 2.755905511811027164, 0.7468891277766205317 ) ) ;
#802 = VECTOR ( 'NONE', #23259, 39.37007874015748143 ) ;
#803 = LINE ( 'NONE', #27900, #7797 ) ;
#804 = DIRECTION ( 'NONE',  ( 0.000000000000000000, -1.000000000000000000, 0.000000000000000000 ) ) ;
#805 = LINE ( 'NONE', #8805, #22763 ) ;
#806 = ORIENTED_EDGE ( 'NONE', *, *, #35915, .F. ) ;
#807 = CARTESIAN_POINT ( 'NONE',  ( -1.815926437556002915, 1.042210485784169194, -1.804289983221820437 ) ) ;
#808 = VECTOR ( 'NONE', #46016, 39.37007874015748854 ) ;
#809 = ORIENTED_EDGE ( 'NONE', *, *, #33052, .T. ) ;
#810 = VERTEX_POINT ( 'NONE', #34877 ) ;
#811 = DIRECTION ( 'NONE',  ( 1.734723475976806848E-16, 0.000000000000000000, 1.000000000000000000 ) ) ;
#812 = DIRECTION ( 'NONE',  ( 1.000000000000000000, 0.000000000000000000, -3.469446951953613696E-16 ) ) ;
#813 = DIRECTION ( 'NONE',  ( -0.000000000000000000, 1.000000000000000000, -0.000000000000000000 ) ) ;
#814 = VERTEX_POINT ( 'NONE', #50555 ) ;
#815 = EDGE_CURVE ( 'NONE', #903, #26348, #50808, .T. ) ;
#816 = ORIENTED_EDGE ( 'NONE', *, *, #43057, .F. ) ;
#817 = CARTESIAN_POINT ( 'NONE',  ( -2.009930929872525418, 1.574803149606302854, -0.8055662819784117357 ) ) ;
#818 = ORIENTED_EDGE ( 'NONE', *, *, #10811, .T. ) ;
#819 = CARTESIAN_POINT ( 'NONE',  ( 0.000000000000000000, 3.267716535433071279, 0.000000000000000000 ) ) ;
#820 = EDGE_CURVE ( 'NONE', #12778, #27951, #43105, .T. ) ;
#821 = EDGE_LOOP ( 'NONE', ( #9721, #36977, #33550, #6151 ) ) ;
#822 = DIRECTION ( 'NONE',  ( 0.000000000000000000, -1.000000000000000000, 0.000000000000000000 ) ) ;
#823 = DIRECTION ( 'NONE',  ( -8.032339854997460071E-17, 1.000000000000000000, 1.007223559679395367E-16 ) ) ;
#824 = DIRECTION ( 'NONE',  ( -3.469446951953613696E-16, 0.000000000000000000, -1.000000000000000000 ) ) ;
#825 = ADVANCED_FACE ( 'NONE', ( #2877 ), #3886, .F. ) ;
#826 = EDGE_CURVE ( 'NONE', #4522, #32688, #43268, .T. ) ;
#827 = ORIENTED_EDGE ( 'NONE', *, *, #8146, .T. ) ;
#828 = EDGE_LOOP ( 'NONE', ( #17732, #25689, #7939, #44891 ) ) ;
#829 = ORIENTED_EDGE ( 'NONE', *, *, #43509, .T. ) ;
#830 = CARTESIAN_POINT ( 'NONE',  ( 1.363819533518803251, 3.267716535433071279, 0.5905511811023579360 ) ) ;
#831 = ORIENTED_EDGE ( 'NONE', *, *, #31034, .T. ) ;
#832 = ORIENTED_EDGE ( 'NONE', *, *, #47602, .F. ) ;
#833 = EDGE_CURVE ( 'NONE', #33133, #25081, #27366, .T. ) ;
#834 = CARTESIAN_POINT ( 'NONE',  ( -1.531154912952794378, 0.000000000000000000, 1.532020527533835441 ) ) ;
#835 = LINE ( 'NONE', #8068, #7117 ) ;
#836 = DIRECTION ( 'NONE',  ( 1.734723475976806848E-16, -0.000000000000000000, 1.000000000000000000 ) ) ;
#837 = EDGE_CURVE ( 'NONE', #35448, #18861, #19618, .T. ) ;
#838 = B_SPLINE_CURVE_WITH_KNOTS ( 'NONE', 3,
 ( #20720, #23832, #36481, #8342 ),
 .UNSPECIFIED., .F., .F.,
 ( 4, 4 ),
 ( 0.01198117231230108604, 0.03073747865870201171 ),
 .UNSPECIFIED. ) ;
#839 = AXIS2_PLACEMENT_3D ( 'NONE', #48946, #26007, #44590 ) ;
#840 = ORIENTED_EDGE ( 'NONE', *, *, #5321, .F. ) ;
#841 = CIRCLE ( 'NONE', #18971, 2.165354330708661568 ) ;
#842 = CARTESIAN_POINT ( 'NONE',  ( 0.5455278134075212115, 3.346456692913386100, -0.9448818897637765168 ) ) ;
#843 = CARTESIAN_POINT ( 'NONE',  ( -1.363819533518803695, 3.267716535433071279, 2.365849761790806473E-16 ) ) ;
#844 = CARTESIAN_POINT ( 'NONE',  ( -1.363819533518803473, 3.346456692913386100, -1.417322834645664109 ) ) ;
#845 = ORIENTED_EDGE ( 'NONE', *, *, #50736, .F. ) ;
#846 = CARTESIAN_POINT ( 'NONE',  ( 1.560669927219590303, 3.267716535433071279, -1.732283464566923170 ) ) ;
#847 = DIRECTION ( 'NONE',  ( -0.000000000000000000, 1.000000000000000000, -0.000000000000000000 ) ) ;
#848 = ORIENTED_EDGE ( 'NONE', *, *, #23875, .F. ) ;
#849 = DIRECTION ( 'NONE',  ( 0.000000000000000000, 0.000000000000000000, -1.000000000000000000 ) ) ;
#850 = VERTEX_POINT ( 'NONE', #26860 ) ;
#851 = EDGE_LOOP ( 'NONE', ( #27475, #12376, #37476, #23396 ) ) ;
#852 = AXIS2_PLACEMENT_3D ( 'NONE', #4132, #16256, #19102 ) ;
#853 = CARTESIAN_POINT ( 'NONE',  ( -1.723687301221637380, 5.905511811023623991, -1.311649477509824857 ) ) ;
#854 = EDGE_CURVE ( 'NONE', #21915, #35502, #15750, .T. ) ;
#855 = CARTESIAN_POINT ( 'NONE',  ( 0.000000000000000000, 5.905511811023623991, 0.000000000000000000 ) ) ;
#856 = DIRECTION ( 'NONE',  ( 0.7660444431189771253, 0.6427876096865404731, 2.214792131866782686E-16 ) ) ;
#857 = EDGE_CURVE ( 'NONE', #6398, #2006, #6752, .T. ) ;
#858 = CARTESIAN_POINT ( 'NONE',  ( 0.2727639067037610499, 0.000000000000000000, 1.732283464566921172 ) ) ;
#859 = ORIENTED_EDGE ( 'NONE', *, *, #6195, .T. ) ;
#860 = ORIENTED_EDGE ( 'NONE', *, *, #18754, .F. ) ;
#861 = ADVANCED_FACE ( 'NONE', ( #38506 ), #7260, .F. ) ;
#862 = DIRECTION ( 'NONE',  ( -0.7818314824680309139, 0.000000000000000000, 0.6234898018587318180 ) ) ;
#863 = ORIENTED_EDGE ( 'NONE', *, *, #49296, .T. ) ;
#864 = DIRECTION ( 'NONE',  ( 1.734723475976806848E-16, -0.000000000000000000, 1.000000000000000000 ) ) ;
#865 = LINE ( 'NONE', #28473, #45696 ) ;
#866 = DIRECTION ( 'NONE',  ( 0.8345732537213079727, 0.000000000000000000, -0.5508969814520945363 ) ) ;
#867 = FACE_OUTER_BOUND ( 'NONE', #35638, .T. ) ;
#868 = CARTESIAN_POINT ( 'NONE',  ( 1.942732458483374280, 5.905511811023623991, 2.223636218514625451 ) ) ;
#869 = VERTEX_POINT ( 'NONE', #4392 ) ;
#870 = CARTESIAN_POINT ( 'NONE',  ( 0.000000000000000000, 3.346456692913386100, 0.000000000000000000 ) ) ;
#871 = DIRECTION ( 'NONE',  ( -1.000000000000000000, 0.000000000000000000, -0.000000000000000000 ) ) ;
#872 = VECTOR ( 'NONE', #18718, 39.37007874015748854 ) ;
#873 = ORIENTED_EDGE ( 'NONE', *, *, #33508, .T. ) ;
#874 = DIRECTION ( 'NONE',  ( 1.000000000000000000, -0.000000000000000000, 0.000000000000000000 ) ) ;
#875 = VECTOR ( 'NONE', #46875, 39.37007874015748143 ) ;
#876 = CARTESIAN_POINT ( 'NONE',  ( -0.8329809839909436686, 1.706281419137876565, -2.833254665166566877 ) ) ;
#877 = CARTESIAN_POINT ( 'NONE',  ( -0.3847164040906153049, 0.5249316497054298258, 1.844349136728716143 ) ) ;
#878 = ORIENTED_EDGE ( 'NONE', *, *, #34136, .F. ) ;
#879 = DIRECTION ( 'NONE',  ( 1.734723475976806848E-16, 0.000000000000000000, 1.000000000000000000 ) ) ;
#880 = LINE ( 'NONE', #27725, #20893 ) ;
#881 = PLANE ( 'NONE',  #3640 ) ;
#882 = EDGE_LOOP ( 'NONE', ( #36469, #24723, #16988, #18000 ) ) ;
#883 = DIRECTION ( 'NONE',  ( 1.000000000000000000, -0.000000000000000000, 0.000000000000000000 ) ) ;
#884 = CIRCLE ( 'NONE', #48679, 2.106299212598425008 ) ;
#885 = CARTESIAN_POINT ( 'NONE',  ( 1.928732080931637505, 3.346456692913386100, -0.9842519685039348154 ) ) ;
#886 = ORIENTED_EDGE ( 'NONE', *, *, #33174, .T. ) ;
#887 = CARTESIAN_POINT ( 'NONE',  ( -2.600183657057300923, 0.000000000000000000, 1.399218491554123700 ) ) ;
#888 = DIRECTION ( 'NONE',  ( 0.1342332658176667026, 0.000000000000000000, -0.9909497617679331460 ) ) ;
#889 = LINE ( 'NONE', #16126, #46909 ) ;
#890 = CARTESIAN_POINT ( 'NONE',  ( 0.1067246931122726866, 0.02962905676920215767, 0.000000000000000000 ) ) ;
#891 = ADVANCED_FACE ( 'NONE', ( #4141 ), #28129, .F. ) ;
#892 = ADVANCED_FACE ( 'NONE', ( #27875 ), #4653, .F. ) ;
#893 = ADVANCED_FACE ( 'NONE', ( #24785 ), #13008, .T. ) ;
#894 = ORIENTED_EDGE ( 'NONE', *, *, #36897, .F. ) ;
#895 = ORIENTED_EDGE ( 'NONE', *, *, #5742, .T. ) ;
#896 = LINE ( 'NONE', #4512, #8403 ) ;
#897 = CARTESIAN_POINT ( 'NONE',  ( 0.5455278134075211005, 3.346456692913386100, -1.456692913385822630 ) ) ;
#898 = ORIENTED_EDGE ( 'NONE', *, *, #47103, .T. ) ;
#899 = DIRECTION ( 'NONE',  ( -3.469446951953613696E-16, 0.000000000000000000, -1.000000000000000000 ) ) ;
#900 = LINE ( 'NONE', #45766, #18611 ) ;
#901 = CARTESIAN_POINT ( 'NONE',  ( 0.2727639067037604392, 0.000000000000000000, -0.03937007874015908959 ) ) ;
#902 = CARTESIAN_POINT ( 'NONE',  ( -0.3486774197067339376, 3.346456692913386100, -1.259842519685035134 ) ) ;
#903 = VERTEX_POINT ( 'NONE', #12391 ) ;
#904 = VERTEX_POINT ( 'NONE', #1287 ) ;
#905 = DIRECTION ( 'NONE',  ( -1.000000000000000000, -0.000000000000000000, -0.000000000000000000 ) ) ;
#906 = CARTESIAN_POINT ( 'NONE',  ( 3.927031490892378253E-16, 3.267716535433071279, 1.692913385826762873 ) ) ;
#907 = FACE_OUTER_BOUND ( 'NONE', #32075, .T. ) ;
#908 = CARTESIAN_POINT ( 'NONE',  ( 1.833433833923351353, 0.000000000000000000, 0.3149606299212576177 ) ) ;
#909 = FACE_BOUND ( 'NONE', #8066, .T. ) ;
#910 = ORIENTED_EDGE ( 'NONE', *, *, #17652, .F. ) ;
#911 = FACE_OUTER_BOUND ( 'NONE', #19718, .T. ) ;
#912 = VERTEX_POINT ( 'NONE', #43619 ) ;
#913 = ORIENTED_EDGE ( 'NONE', *, *, #40482, .F. ) ;
#914 = EDGE_CURVE ( 'NONE', #7908, #34106, #43872, .T. ) ;
#915 = CARTESIAN_POINT ( 'NONE',  ( -0.8942052331142552601, 0.000000000000000000, -1.574803149606293529 ) ) ;
#916 = CIRCLE ( 'NONE', #7504, 2.165354330708661568 ) ;
#917 = EDGE_CURVE ( 'NONE', #7644, #10410, #8521, .T. ) ;
#918 = AXIS2_PLACEMENT_3D ( 'NONE', #12075, #28068, #19806 ) ;
#919 = VERTEX_POINT ( 'NONE', #20648 ) ;
#920 = ORIENTED_EDGE ( 'NONE', *, *, #34296, .F. ) ;
#921 = DIRECTION ( 'NONE',  ( -0.9998717552508122886, -0.01601477604151180928, 0.000000000000000000 ) ) ;
#923 = ADVANCED_FACE ( 'NONE', ( #20390 ), #46792, .T. ) ;
#922 = UNCERTAINTY_MEASURE_WITH_UNIT (LENGTH_MEASURE( 1.000000000000000082E-05 ), #37201, 'distance_accuracy_value', 'NONE');
#924 = VERTEX_POINT ( 'NONE', #17048 ) ;
#925 = ADVANCED_FACE ( 'NONE', ( #27618 ), #19867, .F. ) ;
#926 = VECTOR ( 'NONE', #47714, 39.37007874015748143 ) ;
#927 = PLANE ( 'NONE',  #48454 ) ;
#928 = CARTESIAN_POINT ( 'NONE',  ( 0.5455278134075208785, 0.000000000000000000, -1.771653543307081025 ) ) ;
#929 = PLANE ( 'NONE',  #10245 ) ;
#930 = LINE ( 'NONE', #35533, #39603 ) ;
#931 = DIRECTION ( 'NONE',  ( -1.000000000000000000, -0.000000000000000000, -0.000000000000000000 ) ) ;
#932 = DIRECTION ( 'NONE',  ( -1.000000000000000000, -0.000000000000000000, -0.000000000000000000 ) ) ;
#933 = ORIENTED_EDGE ( 'NONE', *, *, #40776, .F. ) ;
#934 = LINE ( 'NONE', #1444, #9330 ) ;
#935 = PLANE ( 'NONE',  #45777 ) ;
#936 = DIRECTION ( 'NONE',  ( -3.469446951953613696E-16, 0.000000000000000000, -1.000000000000000000 ) ) ;
#937 = ORIENTED_EDGE ( 'NONE', *, *, #32737, .T. ) ;
#938 = CARTESIAN_POINT ( 'NONE',  ( -1.971834065208965203, 5.905511811023623991, 0.8963217522329905984 ) ) ;
#939 = CARTESIAN_POINT ( 'NONE',  ( 1.325491792074624087, 1.641458297549746037, -2.638988599164732385 ) ) ;
#940 = ORIENTED_EDGE ( 'NONE', *, *, #4163, .T. ) ;
#941 = PLANE ( 'NONE',  #42748 ) ;
#942 = LINE ( 'NONE', #20035, #38229 ) ;
#943 = LINE ( 'NONE', #39931, #45738 ) ;
#944 = PRODUCT_DEFINITION_SHAPE ( 'NONE', 'NONE',  #51056 ) ;
#945 = VERTEX_POINT ( 'NONE', #32805 ) ;
#946 = CARTESIAN_POINT ( 'NONE',  ( 0.01632152774899451458, 0.000000000000000000, 1.931620256131032054 ) ) ;
#947 = EDGE_LOOP ( 'NONE', ( #29123, #50516, #44377, #14679 ) ) ;
#948 = FACE_BOUND ( 'NONE', #13602, .T. ) ;
#949 = LINE ( 'NONE', #1458, #1178 ) ;
#950 = VECTOR ( 'NONE', #42020, 39.37007874015748143 ) ;
#951 = AXIS2_PLACEMENT_3D ( 'NONE', #2689, #38071, #21551 ) ;
#952 = DIRECTION ( 'NONE',  ( 1.734723475976806848E-16, -0.000000000000000000, 1.000000000000000000 ) ) ;
#953 = CARTESIAN_POINT ( 'NONE',  ( -0.3486774197067339376, 0.000000000000000000, -0.3149606299212593941 ) ) ;
#954 = ADVANCED_FACE ( 'NONE', ( #44135 ), #4906, .T. ) ;
#955 = CONICAL_SURFACE ( 'NONE', #38086, 2.246510896728926010, 0.01601546068027819014 ) ;
#956 = ORIENTED_EDGE ( 'NONE', *, *, #17590, .F. ) ;
#957 = ORIENTED_EDGE ( 'NONE', *, *, #40205, .T. ) ;
#958 = EDGE_CURVE ( 'NONE', #11836, #35629, #47977, .T. ) ;
#959 = DIRECTION ( 'NONE',  ( -0.000000000000000000, 1.000000000000000000, -0.000000000000000000 ) ) ;
#960 = ORIENTED_EDGE ( 'NONE', *, *, #36010, .T. ) ;
#961 = VECTOR ( 'NONE', #49944, 39.37007874015748143 ) ;
#962 = DIRECTION ( 'NONE',  ( -3.469446951953613696E-16, 0.000000000000000000, -1.000000000000000000 ) ) ;
#963 = ORIENTED_EDGE ( 'NONE', *, *, #4259, .F. ) ;
#964 = EDGE_CURVE ( 'NONE', #3496, #3427, #24528, .T. ) ;
#965 = CARTESIAN_POINT ( 'NONE',  ( -4.268512490100411402E-16, 3.267716535433071279, -2.401574803149598480 ) ) ;
#966 = VECTOR ( 'NONE', #13773, 39.37007874015748143 ) ;
#967 = ORIENTED_EDGE ( 'NONE', *, *, #27641, .F. ) ;
#968 = CARTESIAN_POINT ( 'NONE',  ( -0.5455278134075213226, 3.267716535433071279, 9.463399047163224412E-17 ) ) ;
#969 = CARTESIAN_POINT ( 'NONE',  ( -0.5455278134075214336, 3.346456692913386100, -1.259842519685035134 ) ) ;
#970 = VERTEX_POINT ( 'NONE', #36406 ) ;
#971 = DIRECTION ( 'NONE',  ( -0.000000000000000000, 1.000000000000000000, -0.000000000000000000 ) ) ;
#972 = VERTEX_POINT ( 'NONE', #1031 ) ;
#973 = DIRECTION ( 'NONE',  ( -3.469446951953613696E-16, 0.000000000000000000, -1.000000000000000000 ) ) ;
#974 = ADVANCED_FACE ( 'NONE', ( #31768 ), #32542, .F. ) ;
#975 = VERTEX_POINT ( 'NONE', #40536 ) ;
#976 = EDGE_LOOP ( 'NONE', ( #38466, #49950, #28747, #13635, #8159, #50892, #23802 ) ) ;
#977 = DIRECTION ( 'NONE',  ( -1.000000000000000000, -0.000000000000000000, -0.000000000000000000 ) ) ;
#978 = EDGE_CURVE ( 'NONE', #35509, #32131, #8266, .T. ) ;
#979 = ORIENTED_EDGE ( 'NONE', *, *, #15372, .T. ) ;
#980 = DIRECTION ( 'NONE',  ( 1.734723475976806848E-16, -0.000000000000000000, 1.000000000000000000 ) ) ;
#981 = ORIENTED_EDGE ( 'NONE', *, *, #8600, .F. ) ;
#982 = CARTESIAN_POINT ( 'NONE',  ( 2.044241703397536192, 6.692913385826772199, -0.7159595814952630644 ) ) ;
#983 = AXIS2_PLACEMENT_3D ( 'NONE', #50342, #14533, #2406 ) ;
#984 = CARTESIAN_POINT ( 'NONE',  ( 2.755905511811024056, 4.960629921259846142, -1.023622047244094224 ) ) ;
#985 = CIRCLE ( 'NONE', #47931, 0.3740157480314960647 ) ;
#986 = LINE ( 'NONE', #4865, #10723 ) ;
#987 = ORIENTED_EDGE ( 'NONE', *, *, #38720, .T. ) ;
#988 = AXIS2_PLACEMENT_3D ( 'NONE', #38689, #38436, #3565 ) ;
#989 = CARTESIAN_POINT ( 'NONE',  ( 1.293618082698028804, 0.000000000000000000, -1.168738992012442246 ) ) ;
#990 = DIRECTION ( 'NONE',  ( -0.000000000000000000, -1.000000000000000000, -0.000000000000000000 ) ) ;
#991 = DIRECTION ( 'NONE',  ( -3.469446951953613696E-16, 0.000000000000000000, -1.000000000000000000 ) ) ;
#992 = CARTESIAN_POINT ( 'NONE',  ( 1.287906020515829919, 3.267716535433071279, -1.771653543307081691 ) ) ;
#993 = VECTOR ( 'NONE', #22067, 39.37007874015748143 ) ;
#994 = FACE_OUTER_BOUND ( 'NONE', #10388, .T. ) ;
#995 = CARTESIAN_POINT ( 'NONE',  ( 1.363819533518803695, 3.346456692913386100, 1.535433070866133898 ) ) ;
#996 = AXIS2_PLACEMENT_3D ( 'NONE', #15783, #27913, #39285 ) ;
#997 = DIRECTION ( 'NONE',  ( 0.000000000000000000, -1.000000000000000000, 0.000000000000000000 ) ) ;
#998 = ORIENTED_EDGE ( 'NONE', *, *, #45478, .F. ) ;
#999 = DIRECTION ( 'NONE',  ( 1.734723475976806848E-16, -0.000000000000000000, 1.000000000000000000 ) ) ;
#1000 = DIRECTION ( 'NONE',  ( -1.000000000000000000, 0.000000000000000000, -0.000000000000000000 ) ) ;
#1001 = EDGE_LOOP ( 'NONE', ( #26786, #37902, #50195, #9710 ) ) ;
#1002 = CARTESIAN_POINT ( 'NONE',  ( 0.000000000000000000, 3.267716535433071279, -1.417322834645664331 ) ) ;
#1003 = ORIENTED_EDGE ( 'NONE', *, *, #17058, .T. ) ;
#1004 = CARTESIAN_POINT ( 'NONE',  ( 1.331808205664952505, 0.000000000000000000, 1.125026879082043685 ) ) ;
#1005 = DIRECTION ( 'NONE',  ( 0.000000000000000000, -1.000000000000000000, 0.000000000000000000 ) ) ;
#1006 = DIRECTION ( 'NONE',  ( 1.734723475976806848E-16, 0.000000000000000000, 1.000000000000000000 ) ) ;
#1007 = CARTESIAN_POINT ( 'NONE',  ( -0.8942052331142552601, 3.346456692913386100, -1.889763779527552146 ) ) ;
#1008 = VERTEX_POINT ( 'NONE', #20909 ) ;
#1009 = DIRECTION ( 'NONE',  ( -1.000000000000000000, 0.000000000000000000, 0.000000000000000000 ) ) ;
#1010 = EDGE_CURVE ( 'NONE', #9489, #2168, #36665, .T. ) ;
#1011 = FACE_BOUND ( 'NONE', #46470, .T. ) ;
#1012 = EDGE_CURVE ( 'NONE', #36186, #15116, #40790, .T. ) ;
#1013 = ORIENTED_EDGE ( 'NONE', *, *, #2786, .T. ) ;
#1014 = CARTESIAN_POINT ( 'NONE',  ( 0.08119777152254364916, 1.623385212329073957, 0.000000000000000000 ) ) ;
#1015 = ORIENTED_EDGE ( 'NONE', *, *, #22221, .T. ) ;
#1016 = EDGE_CURVE ( 'NONE', #50754, #37363, #6363, .T. ) ;
#1017 = DIRECTION ( 'NONE',  ( 0.000000000000000000, 0.000000000000000000, -1.000000000000000000 ) ) ;
#1018 = CARTESIAN_POINT ( 'NONE',  ( -1.363819533518803473, 3.346456692913386100, -0.1574803149606300023 ) ) ;
#1019 = VECTOR ( 'NONE', #7452, 39.37007874015748143 ) ;
#1020 = ADVANCED_FACE ( 'NONE', ( #17300 ), #37945, .F. ) ;
#1021 = VECTOR ( 'NONE', #24147, 39.37007874015748143 ) ;
#1022 = CARTESIAN_POINT ( 'NONE',  ( 1.909347346926324684, 3.346456692913386100, 0.1574803149606280872 ) ) ;
#1023 = VERTEX_POINT ( 'NONE', #37695 ) ;
#1024 = ORIENTED_EDGE ( 'NONE', *, *, #14890, .T. ) ;
#1025 = DIRECTION ( 'NONE',  ( -0.9839295885986296675, -1.160734090543305153E-16, -0.1785568947986370669 ) ) ;
#1027 = DIRECTION ( 'NONE',  ( -8.653332088726061579E-16, 0.7071067811865483499, -0.7071067811865466846 ) ) ;
#1026 = VECTOR ( 'NONE', #49061, 39.37007874015748143 ) ;
#1028 = FACE_BOUND ( 'NONE', #16644, .T. ) ;
#1029 = VECTOR ( 'NONE', #35152, 39.37007874015748143 ) ;
#1030 = VECTOR ( 'NONE', #10332, 39.37007874015748143 ) ;
#1031 = CARTESIAN_POINT ( 'NONE',  ( 1.325491792074623643, 1.485765544018708750, -2.638988599164732385 ) ) ;
#1032 = EDGE_CURVE ( 'NONE', #6504, #4531, #26055, .T. ) ;
#1033 = LINE ( 'NONE', #16790, #43158 ) ;
#1034 = ORIENTED_EDGE ( 'NONE', *, *, #27811, .F. ) ;
#1035 = CARTESIAN_POINT ( 'NONE',  ( -0.4371342596750092402, 2.755905511811024056, -1.309652049997256373 ) ) ;
#1036 = EDGE_CURVE ( 'NONE', #3507, #3351, #25295, .T. ) ;
#1037 = ORIENTED_EDGE ( 'NONE', *, *, #26495, .F. ) ;
#1038 = VERTEX_POINT ( 'NONE', #41052 ) ;
#1039 = VERTEX_POINT ( 'NONE', #49502 ) ;
#1040 = LINE ( 'NONE', #48246, #25143 ) ;
#1041 = LINE ( 'NONE', #48247, #49671 ) ;
#1042 = CARTESIAN_POINT ( 'NONE',  ( 0.2727639067037605503, 3.267716535433071279, -4.731699523581609125E-17 ) ) ;
#1043 = DIRECTION ( 'NONE',  ( 1.734723475976806848E-16, -0.000000000000000000, 1.000000000000000000 ) ) ;
#1044 = ORIENTED_EDGE ( 'NONE', *, *, #5472, .T. ) ;
#1045 = ORIENTED_EDGE ( 'NONE', *, *, #50865, .F. ) ;
#1046 = DIRECTION ( 'NONE',  ( 0.000000000000000000, -1.000000000000000000, 0.000000000000000000 ) ) ;
#1047 = DIRECTION ( 'NONE',  ( -3.469446951953613696E-16, 0.000000000000000000, -1.000000000000000000 ) ) ;
#1048 = DIRECTION ( 'NONE',  ( -1.000000000000000000, -0.000000000000000000, -0.000000000000000000 ) ) ;
#1049 = ADVANCED_FACE ( 'NONE', ( #45395 ), #16313, .T. ) ;
#1050 = CARTESIAN_POINT ( 'NONE',  ( 0.000000000000000000, 3.267716535433071279, -0.1968503937007874405 ) ) ;
#1051 = LINE ( 'NONE', #9314, #18238 ) ;
#1052 = LINE ( 'NONE', #16811, #39981 ) ;
#1053 = DIRECTION ( 'NONE',  ( 1.000000000000000000, 0.000000000000000000, 0.000000000000000000 ) ) ;
#1054 = CARTESIAN_POINT ( 'NONE',  ( 0.4696143004045479352, 3.267716535433071279, -1.102362204724405714 ) ) ;
#1055 = AXIS2_PLACEMENT_3D ( 'NONE', #41927, #46527, #47018 ) ;
#1056 = VERTEX_POINT ( 'NONE', #1547 ) ;
#1057 = DIRECTION ( 'NONE',  ( 1.734723475976806848E-16, -0.000000000000000000, 1.000000000000000000 ) ) ;
#1058 = DIRECTION ( 'NONE',  ( -1.000000000000000000, 0.000000000000000000, -2.891205793294678326E-16 ) ) ;
#1059 = VERTEX_POINT ( 'NONE', #17549 ) ;
#1060 = VECTOR ( 'NONE', #15527, 39.37007874015748143 ) ;
#1061 = ORIENTED_EDGE ( 'NONE', *, *, #30500, .T. ) ;
#1062 = DIRECTION ( 'NONE',  ( -1.000000000000000000, 0.000000000000000000, -0.000000000000000000 ) ) ;
#1063 = CARTESIAN_POINT ( 'NONE',  ( -0.5455278134075214336, 0.000000000000000000, -0.3149606299212593941 ) ) ;
#1064 = DIRECTION ( 'NONE',  ( -1.288287287306305283E-16, 1.000000000000000000, 0.000000000000000000 ) ) ;
#1065 = EDGE_LOOP ( 'NONE', ( #15452, #25045, #35705, #16560 ) ) ;
#1066 = CONICAL_SURFACE ( 'NONE', #21685, 2.165354330708661568, 0.2617993877991570129 ) ;
#1067 = ORIENTED_EDGE ( 'NONE', *, *, #39592, .T. ) ;
#1068 = CARTESIAN_POINT ( 'NONE',  ( -1.712496953225537633, 0.000000000000000000, -0.6692913385826758654 ) ) ;
#1069 = ORIENTED_EDGE ( 'NONE', *, *, #43915, .F. ) ;
#1070 = ORIENTED_EDGE ( 'NONE', *, *, #20041, .F. ) ;
#1071 = EDGE_CURVE ( 'NONE', #19845, #37743, #1798, .T. ) ;
#1072 = CARTESIAN_POINT ( 'NONE',  ( -0.9788642269881570046, 0.000000000000000000, 1.542392924267547594 ) ) ;
#1073 = CARTESIAN_POINT ( 'NONE',  ( 0.000000000000000000, 2.362204724409439294, -2.952755905511811552 ) ) ;
#1074 = CARTESIAN_POINT ( 'NONE',  ( 1.363819533518803251, 0.000000000000000000, 1.102362204724403938 ) ) ;
#1075 = EDGE_CURVE ( 'NONE', #27292, #42794, #48995, .T. ) ;
#1076 = EDGE_CURVE ( 'NONE', #17210, #50226, #17802, .T. ) ;
#1077 = ORIENTED_EDGE ( 'NONE', *, *, #35917, .F. ) ;
#1078 = EDGE_LOOP ( 'NONE', ( #26374, #17593, #10106, #4070 ) ) ;
#1079 = EDGE_LOOP ( 'NONE', ( #23511, #43814, #17866, #31625, #14880, #20227, #36101, #49457, #5457, #21591, #15292 ) ) ;
#1080 = CARTESIAN_POINT ( 'NONE',  ( 0.000000000000000000, 6.692913385826772199, 0.000000000000000000 ) ) ;
#1081 = EDGE_LOOP ( 'NONE', ( #41232, #49198, #10708, #49790, #31537, #35455, #45146 ) ) ;
#1082 = EDGE_LOOP ( 'NONE', ( #41251, #1474, #22226, #42100 ) ) ;
#1083 = CARTESIAN_POINT ( 'NONE',  ( 1.015142113812069313, 3.346456692913386100, 0.2755905511810994302 ) ) ;
#1084 = LINE ( 'NONE', #48035, #43388 ) ;
#1085 = FACE_OUTER_BOUND ( 'NONE', #25070, .T. ) ;
#1086 = ORIENTED_EDGE ( 'NONE', *, *, #15124, .F. ) ;
#1087 = DIRECTION ( 'NONE',  ( -0.000000000000000000, 1.000000000000000000, -0.000000000000000000 ) ) ;
#1088 = CARTESIAN_POINT ( 'NONE',  ( -2.946551303128973842, 1.574890269766889617, -0.1815919737934194866 ) ) ;
#1089 = DIRECTION ( 'NONE',  ( 1.000000000000000000, 0.000000000000000000, -3.469446951953613696E-16 ) ) ;
#1090 = ORIENTED_EDGE ( 'NONE', *, *, #7820, .F. ) ;
#1091 = DIRECTION ( 'NONE',  ( -0.9998717552508121775, -0.01601477604151182663, 0.000000000000000000 ) ) ;
#1092 = VECTOR ( 'NONE', #12393, 39.37007874015748143 ) ;
#1093 = CARTESIAN_POINT ( 'NONE',  ( -0.04921259842519708216, 1.641496925592597966, 2.242214099218965195 ) ) ;
#1094 = PLANE ( 'NONE',  #30734 ) ;
#1095 = ORIENTED_EDGE ( 'NONE', *, *, #45812, .F. ) ;
#1096 = AXIS2_PLACEMENT_3D ( 'NONE', #3994, #7862, #26965 ) ;
#1097 = ORIENTED_EDGE ( 'NONE', *, *, #35685, .T. ) ;
#1098 = DIRECTION ( 'NONE',  ( -0.000000000000000000, 0.000000000000000000, 1.000000000000000000 ) ) ;
#1099 = VECTOR ( 'NONE', #21493, 39.37007874015748143 ) ;
#1100 = CIRCLE ( 'NONE', #19261, 1.850107469027523432 ) ;
#1101 = FACE_OUTER_BOUND ( 'NONE', #13167, .T. ) ;
#1102 = EDGE_CURVE ( 'NONE', #14290, #26003, #10310, .T. ) ;
#1103 = CARTESIAN_POINT ( 'NONE',  ( 1.560669927219590525, 3.267716535433071279, -5.414661521997676285E-16 ) ) ;
#1104 = CARTESIAN_POINT ( 'NONE',  ( 0.4506430153629077950, 0.03513753811042658048, -1.817852439337431569 ) ) ;
#1105 = ORIENTED_EDGE ( 'NONE', *, *, #22057, .T. ) ;
#1106 = EDGE_LOOP ( 'NONE', ( #28845, #3707, #6094, #23795 ) ) ;
#1107 = VECTOR ( 'NONE', #1890, 39.37007874015748854 ) ;
#1108 = CARTESIAN_POINT ( 'NONE',  ( 2.593208359734349600, 1.657742242070020078, 0.8943296607142533494 ) ) ;
#1109 = ORIENTED_EDGE ( 'NONE', *, *, #8111, .F. ) ;
#1110 = DIRECTION ( 'NONE',  ( -1.000000000000000000, 0.000000000000000000, 0.000000000000000000 ) ) ;
#1111 = EDGE_CURVE ( 'NONE', #14945, #25938, #2309, .T. ) ;
#1112 = PLANE ( 'NONE',  #11089 ) ;
#1113 = CARTESIAN_POINT ( 'NONE',  ( 0.000000000000000000, 3.267716535433071279, -0.4724409448818886470 ) ) ;
#1114 = CARTESIAN_POINT ( 'NONE',  ( 2.378961647330872786, 3.267716535433071279, -8.253681236146643855E-16 ) ) ;
#1115 = DIRECTION ( 'NONE',  ( -0.000000000000000000, 1.000000000000000000, -0.000000000000000000 ) ) ;
#1116 = ORIENTED_EDGE ( 'NONE', *, *, #33103, .T. ) ;
#1117 = CARTESIAN_POINT ( 'NONE',  ( -0.8182917201112819283, 0.000000000000000000, -1.417322834645664331 ) ) ;
#1118 = EDGE_CURVE ( 'NONE', #12966, #34448, #33059, .T. ) ;
#1119 = LINE ( 'NONE', #13262, #12517 ) ;
#1120 = EDGE_CURVE ( 'NONE', #13966, #33237, #31590, .T. ) ;
#1121 = ORIENTED_EDGE ( 'NONE', *, *, #19037, .F. ) ;
#1122 = CARTESIAN_POINT ( 'NONE',  ( -0.8182917201112814842, 3.267716535433071279, 0.4724409448818872592 ) ) ;
#1123 = CARTESIAN_POINT ( 'NONE',  ( 1.905060681038603265, 5.905511811023623991, 1.081042454612135773 ) ) ;
#1124 = DIRECTION ( 'NONE',  ( -0.000000000000000000, 1.000000000000000000, -0.000000000000000000 ) ) ;
#1125 = VERTEX_POINT ( 'NONE', #6440 ) ;
#1126 = LINE ( 'NONE', #20233, #44035 ) ;
#1127 = LINE ( 'NONE', #36765, #14295 ) ;
#1128 = CARTESIAN_POINT ( 'NONE',  ( -1.494044303739022972, 0.003989811691878806209, -0.9272426299426647089 ) ) ;
#1129 = AXIS2_PLACEMENT_3D ( 'NONE', #36037, #4536, #16929 ) ;
#1130 = ORIENTED_EDGE ( 'NONE', *, *, #8974, .F. ) ;
#1131 = AXIS2_PLACEMENT_3D ( 'NONE', #16246, #43081, #39223 ) ;
#1132 = FACE_BOUND ( 'NONE', #14256, .T. ) ;
#1133 = LINE ( 'NONE', #16897, #41890 ) ;
#1134 = ORIENTED_EDGE ( 'NONE', *, *, #45624, .T. ) ;
#1135 = PLANE ( 'NONE',  #40235 ) ;
#1136 = VECTOR ( 'NONE', #31899, 39.37007874015748143 ) ;
#1137 = EDGE_CURVE ( 'NONE', #21069, #35652, #9293, .T. ) ;
#1138 = VECTOR ( 'NONE', #5184, 39.37007874015748143 ) ;
#1139 = CARTESIAN_POINT ( 'NONE',  ( -1.091055626815042645, 3.346456692913386100, -1.889763779527552146 ) ) ;
#1140 = LINE ( 'NONE', #32916, #16448 ) ;
#1141 = DIRECTION ( 'NONE',  ( -1.000000000000000000, -0.000000000000000000, -0.000000000000000000 ) ) ;
#1142 = ADVANCED_FACE ( 'NONE', ( #22192 ), #45142, .F. ) ;
#1143 = B_SPLINE_CURVE_WITH_KNOTS ( 'NONE', 3,
 ( #5463, #32852, #20953, #1072 ),
 .UNSPECIFIED., .F., .F.,
 ( 4, 4 ),
 ( 0.001269765538541185778, 0.002242903636894877199 ),
 .UNSPECIFIED. ) ;
#1144 = EDGE_CURVE ( 'NONE', #49145, #50578, #9807, .T. ) ;
#1145 = DIRECTION ( 'NONE',  ( 0.000000000000000000, -1.000000000000000000, 0.000000000000000000 ) ) ;
#1146 = ORIENTED_EDGE ( 'NONE', *, *, #12692, .F. ) ;
#1147 = VERTEX_POINT ( 'NONE', #44639 ) ;
#1148 = DIRECTION ( 'NONE',  ( 0.000000000000000000, 0.000000000000000000, -1.000000000000000000 ) ) ;
#1149 = VECTOR ( 'NONE', #2088, 39.37007874015748143 ) ;
#1150 = ADVANCED_FACE ( 'NONE', ( #9549 ), #14943, .F. ) ;
#1151 = DIRECTION ( 'NONE',  ( -1.000000000000000000, 0.000000000000000000, -0.000000000000000000 ) ) ;
#1152 = VERTEX_POINT ( 'NONE', #14692 ) ;
#1153 = PLANE ( 'NONE',  #23389 ) ;
#1154 = DIRECTION ( 'NONE',  ( -0.000000000000000000, 1.000000000000000000, -0.000000000000000000 ) ) ;
#1155 = FACE_OUTER_BOUND ( 'NONE', #30697, .T. ) ;
#1156 = DIRECTION ( 'NONE',  ( -0.000000000000000000, 1.000000000000000000, -0.000000000000000000 ) ) ;
#1157 = ORIENTED_EDGE ( 'NONE', *, *, #179, .T. ) ;
#1158 = ORIENTED_EDGE ( 'NONE', *, *, #15486, .T. ) ;
#1159 = LINE ( 'NONE', #16915, #43538 ) ;
#1160 = LINE ( 'NONE', #28009, #50491 ) ;
#1161 = CARTESIAN_POINT ( 'NONE',  ( -0.01640406444054503393, 1.620550207048756963, 2.952755905511811108 ) ) ;
#1162 = VERTEX_POINT ( 'NONE', #23435 ) ;
#1163 = DIRECTION ( 'NONE',  ( -0.000000000000000000, 1.000000000000000000, -0.000000000000000000 ) ) ;
#1164 = FACE_BOUND ( 'NONE', #5789, .T. ) ;
#1165 = ORIENTED_EDGE ( 'NONE', *, *, #34224, .F. ) ;
#1166 = DIRECTION ( 'NONE',  ( -0.9998717552508122886, -0.01601477604151181275, 0.000000000000000000 ) ) ;
#1167 = ORIENTED_EDGE ( 'NONE', *, *, #11323, .F. ) ;
#1168 = ORIENTED_EDGE ( 'NONE', *, *, #40374, .T. ) ;
#1169 = DIRECTION ( 'NONE',  ( 0.9639628606958511314, -3.091822751912359432E-17, 0.2660368455666826115 ) ) ;
#1170 = ORIENTED_EDGE ( 'NONE', *, *, #6960, .T. ) ;
#1172 = VERTEX_POINT ( 'NONE', #39190 ) ;
#1171 = EDGE_CURVE ( 'NONE', #33562, #2530, #34816, .T. ) ;
#1173 = CARTESIAN_POINT ( 'NONE',  ( 0.7423782071083091516, 3.267716535433071279, 1.377952755905504256 ) ) ;
#1174 = B_SPLINE_CURVE_WITH_KNOTS ( 'NONE', 3,
 ( #22788, #31038, #30537, #30281 ),
 .UNSPECIFIED., .F., .F.,
 ( 4, 4 ),
 ( 0.0001044316291836491680, 0.0001857920852460473622 ),
 .UNSPECIFIED. ) ;
#1175 = ORIENTED_EDGE ( 'NONE', *, *, #47514, .F. ) ;
#1176 = CARTESIAN_POINT ( 'NONE',  ( 1.990939428460624105, 0.03922503611537826729, 0.3193531217849331916 ) ) ;
#1177 = CIRCLE ( 'NONE', #314, 2.106299212598425008 ) ;
#1178 = VECTOR ( 'NONE', #40202, 39.37007874015748143 ) ;
#1179 = DIRECTION ( 'NONE',  ( -0.000000000000000000, 1.000000000000000000, -0.000000000000000000 ) ) ;
#1180 = DIRECTION ( 'NONE',  ( -0.000000000000000000, 1.000000000000000000, -0.000000000000000000 ) ) ;
#1181 = ADVANCED_FACE ( 'NONE', ( #22943 ), #3071, .F. ) ;
#1182 = CARTESIAN_POINT ( 'NONE',  ( 0.2727639067037604947, 0.000000000000000000, -0.7874015748031473194 ) ) ;
#1183 = VECTOR ( 'NONE', #10683, 39.37007874015748143 ) ;
#1184 = AXIS2_PLACEMENT_3D ( 'NONE', #33536, #45363, #22407 ) ;
#1185 = EDGE_CURVE ( 'NONE', #16476, #20835, #6693, .T. ) ;
#1186 = EDGE_CURVE ( 'NONE', #30118, #10548, #3573, .T. ) ;
#1187 = CARTESIAN_POINT ( 'NONE',  ( 1.108686381432267831, 0.03016422574328766690, -1.609701364138947932 ) ) ;
#1188 = DIRECTION ( 'NONE',  ( -1.000000000000000000, 0.000000000000000000, -0.000000000000000000 ) ) ;
#1189 = CARTESIAN_POINT ( 'NONE',  ( 1.122047244094487750, 0.5314960629921257063, -1.062992125984252079 ) ) ;
#1190 = VECTOR ( 'NONE', #48209, 39.37007874015748143 ) ;
#1191 = EDGE_LOOP ( 'NONE', ( #46329, #19740, #20982, #5370 ) ) ;
#1192 = CARTESIAN_POINT ( 'NONE',  ( -0.07591351300297277671, 3.346456692913386100, 1.732283464566921172 ) ) ;
#1193 = LINE ( 'NONE', #47628, #45436 ) ;
#1194 = ORIENTED_EDGE ( 'NONE', *, *, #13124, .F. ) ;
#1195 = DIRECTION ( 'NONE',  ( -0.000000000000000000, 1.000000000000000000, -0.000000000000000000 ) ) ;
#1196 = DIRECTION ( 'NONE',  ( -0.000000000000000000, 1.000000000000000000, -0.000000000000000000 ) ) ;
#1197 = ORIENTED_EDGE ( 'NONE', *, *, #367, .T. ) ;
#1198 = CARTESIAN_POINT ( 'NONE',  ( 0.5455278134075212115, 3.267716535433071279, -1.259842519685035134 ) ) ;
#1199 = EDGE_CURVE ( 'NONE', #41298, #4851, #40189, .T. ) ;
#1200 = CARTESIAN_POINT ( 'NONE',  ( -1.062992125984252079, 0.4235180831842794702, -1.014069264286642236 ) ) ;
#1201 = DIRECTION ( 'NONE',  ( -3.469446951953613696E-16, 0.000000000000000000, -1.000000000000000000 ) ) ;
#1202 = ORIENTED_EDGE ( 'NONE', *, *, #46352, .T. ) ;
#1203 = CARTESIAN_POINT ( 'NONE',  ( 0.4696143004045479352, 0.000000000000000000, 0.7874015748031454320 ) ) ;
#1204 = ADVANCED_FACE ( 'NONE', ( #15451 ), #15195, .F. ) ;
#1205 = VERTEX_POINT ( 'NONE', #3318 ) ;
#1206 = FACE_BOUND ( 'NONE', #41476, .T. ) ;
#1207 = DIRECTION ( 'NONE',  ( -1.000000000000000000, 0.000000000000000000, 1.734723475976806848E-16 ) ) ;
#1208 = CARTESIAN_POINT ( 'NONE',  ( 1.015142113812069313, 3.346456692913386100, -0.1574803149606301411 ) ) ;
#1209 = CARTESIAN_POINT ( 'NONE',  ( -2.156388021673881994, 3.346456692913386100, -0.1968503937007880511 ) ) ;
#1210 = EDGE_CURVE ( 'NONE', #2485, #3425, #46405, .T. ) ;
#1211 = EDGE_CURVE ( 'NONE', #15158, #32340, #43047, .T. ) ;
#1212 = EDGE_LOOP ( 'NONE', ( #48675, #11331, #11084, #8919 ) ) ;
#1213 = VERTEX_POINT ( 'NONE', #7700 ) ;
#1214 = AXIS2_PLACEMENT_3D ( 'NONE', #28218, #32119, #4738 ) ;
#1215 = LINE ( 'NONE', #28832, #18052 ) ;
#1216 = EDGE_CURVE ( 'NONE', #6110, #3179, #26310, .T. ) ;
#1217 = ORIENTED_EDGE ( 'NONE', *, *, #17495, .F. ) ;
#1218 = CIRCLE ( 'NONE', #30918, 2.165354330708661568 ) ;
#1219 = DIRECTION ( 'NONE',  ( 1.734723475976806848E-16, 0.000000000000000000, 1.000000000000000000 ) ) ;
#1220 = ORIENTED_EDGE ( 'NONE', *, *, #17572, .T. ) ;
#1221 = AXIS2_PLACEMENT_3D ( 'NONE', #12573, #8192, #39683 ) ;
#1222 = VECTOR ( 'NONE', #30351, 39.37007874015748143 ) ;
#1223 = CARTESIAN_POINT ( 'NONE',  ( -1.647545174055839556, 0.001531214329375737114, 0.5870650656849111249 ) ) ;
#1224 = ORIENTED_EDGE ( 'NONE', *, *, #41520, .F. ) ;
#1225 = DIRECTION ( 'NONE',  ( 0.000000000000000000, 0.000000000000000000, 1.000000000000000000 ) ) ;
#1226 = CARTESIAN_POINT ( 'NONE',  ( -0.2646829987305902021, 0.000000000000000000, -2.940868978332400463 ) ) ;
#1227 = VECTOR ( 'NONE', #48658, 39.37007874015748143 ) ;
#1228 = EDGE_LOOP ( 'NONE', ( #6121, #26183, #37911, #48872, #37849, #48926, #785, #4251, #9270, #6248, #19395 ) ) ;
#1229 = CARTESIAN_POINT ( 'NONE',  ( 2.721588343796087717, 1.663187266887471205, -1.145422814533112899 ) ) ;
#1230 = VERTEX_POINT ( 'NONE', #19308 ) ;
#1231 = ORIENTED_EDGE ( 'NONE', *, *, #42981, .T. ) ;
#1232 = ORIENTED_EDGE ( 'NONE', *, *, #23643, .T. ) ;
#1233 = ORIENTED_EDGE ( 'NONE', *, *, #5607, .T. ) ;
#1234 = CARTESIAN_POINT ( 'NONE',  ( -1.483604961240789999, 6.692913385826772199, 1.623324365321668017 ) ) ;
#1235 = ORIENTED_EDGE ( 'NONE', *, *, #21671, .F. ) ;
#1236 = LINE ( 'NONE', #1490, #21314 ) ;
#1237 = ORIENTED_EDGE ( 'NONE', *, *, #11037, .F. ) ;
#1238 = DIRECTION ( 'NONE',  ( -0.9510565162951544194, 0.000000000000000000, 0.3090169943749447312 ) ) ;
#1239 = EDGE_CURVE ( 'NONE', #36543, #39867, #49754, .T. ) ;
#1240 = CARTESIAN_POINT ( 'NONE',  ( -1.166969139818015977, 3.267716535433071279, 4.048737525165546155E-16 ) ) ;
#1241 = B_SPLINE_CURVE_WITH_KNOTS ( 'NONE', 3,
 ( #46633, #50230, #27539, #3293 ),
 .UNSPECIFIED., .F., .F.,
 ( 4, 4 ),
 ( 2.175073874924207950E-07, 0.002500264360679614953 ),
 .UNSPECIFIED. ) ;
#1242 = ORIENTED_EDGE ( 'NONE', *, *, #32021, .F. ) ;
#1243 = EDGE_CURVE ( 'NONE', #25538, #48074, #27054, .T. ) ;
#1244 = LINE ( 'NONE', #13128, #49990 ) ;
#1245 = DIRECTION ( 'NONE',  ( 0.9009688679024154823, -5.039827768864211898E-17, 0.4338837391175656699 ) ) ;
#1246 = VECTOR ( 'NONE', #36949, 39.37007874015748143 ) ;
#1247 = CARTESIAN_POINT ( 'NONE',  ( 1.363819533518803029, 3.346456692913386100, -1.929133858267710666 ) ) ;
#1248 = LINE ( 'NONE', #13380, #46404 ) ;
#1249 = AXIS2_PLACEMENT_3D ( 'NONE', #6719, #22464, #38223 ) ;
#1250 = CYLINDRICAL_SURFACE ( 'NONE', #40010, 2.874015748031496731 ) ;
#1251 = AXIS2_PLACEMENT_3D ( 'NONE', #33743, #49426, #37868 ) ;
#1252 = FACE_OUTER_BOUND ( 'NONE', #35938, .T. ) ;
#1253 = LINE ( 'NONE', #39731, #35886 ) ;
#1254 = ORIENTED_EDGE ( 'NONE', *, *, #45638, .T. ) ;
#1255 = CARTESIAN_POINT ( 'NONE',  ( 1.363819533518803695, 3.267716535433071279, 1.681890501046755748 ) ) ;
#1256 = CARTESIAN_POINT ( 'NONE',  ( 0.002207914879453961969, 6.692913385826772199, 0.04916304461325451958 ) ) ;
#1257 = AXIS2_PLACEMENT_3D ( 'NONE', #44252, #39878, #32398 ) ;
#1258 = ORIENTED_EDGE ( 'NONE', *, *, #49705, .T. ) ;
#1259 = CARTESIAN_POINT ( 'NONE',  ( 1.472219874544873131, 1.482402307789154161, 2.560030851058970214 ) ) ;
#1260 = EDGE_CURVE ( 'NONE', #22883, #35609, #10812, .T. ) ;
#1261 = EDGE_LOOP ( 'NONE', ( #37406, #30893, #37324, #37824 ) ) ;
#1262 = CARTESIAN_POINT ( 'NONE',  ( -2.437180031585919782, 0.000000000000000000, -1.667735833703134274 ) ) ;
#1263 = DIRECTION ( 'NONE',  ( 0.000000000000000000, 0.000000000000000000, 1.000000000000000000 ) ) ;
#1264 = CARTESIAN_POINT ( 'NONE',  ( 1.775400203342704764, 0.000000000000000000, -2.359903268218703332 ) ) ;
#1265 = EDGE_CURVE ( 'NONE', #2673, #22594, #46900, .T. ) ;
#1266 = LINE ( 'NONE', #36129, #46507 ) ;
#1267 = CARTESIAN_POINT ( 'NONE',  ( 2.106197740627111514, 3.267716535433070391, -1.239052911296964155 ) ) ;
#1268 = ORIENTED_EDGE ( 'NONE', *, *, #5447, .F. ) ;
#1269 = CARTESIAN_POINT ( 'NONE',  ( 0.000000000000000000, 3.267716535433071279, 0.1574803149606283648 ) ) ;
#1270 = DIRECTION ( 'NONE',  ( 1.000000000000000000, 0.000000000000000000, -3.469446951953613696E-16 ) ) ;
#1271 = EDGE_CURVE ( 'NONE', #34518, #40355, #50011, .T. ) ;
#1272 = ORIENTED_EDGE ( 'NONE', *, *, #39929, .T. ) ;
#1273 = DIRECTION ( 'NONE',  ( -3.469446951953613696E-16, 0.000000000000000000, -1.000000000000000000 ) ) ;
#1274 = EDGE_CURVE ( 'NONE', #25478, #18496, #10536, .T. ) ;
#1275 = EDGE_LOOP ( 'NONE', ( #31845, #29624, #7999, #48821 ) ) ;
#1276 = CARTESIAN_POINT ( 'NONE',  ( 1.560669927219590747, 3.267716535433071279, -0.4724409448818889246 ) ) ;
#1277 = FACE_OUTER_BOUND ( 'NONE', #3325, .T. ) ;
#1278 = FACE_OUTER_BOUND ( 'NONE', #30664, .T. ) ;
#1279 = VECTOR ( 'NONE', #44855, 39.37007874015748854 ) ;
#1280 = VERTEX_POINT ( 'NONE', #14438 ) ;
#1281 = ORIENTED_EDGE ( 'NONE', *, *, #24917, .F. ) ;
#1282 = AXIS2_PLACEMENT_3D ( 'NONE', #10730, #26466, #26719 ) ;
#1283 = CARTESIAN_POINT ( 'NONE',  ( 0.3382312733057617482, 0.000000000000000000, -2.139420919314966252 ) ) ;
#1284 = LINE ( 'NONE', #36919, #33960 ) ;
#1285 = LINE ( 'NONE', #31765, #43320 ) ;
#1286 = ORIENTED_EDGE ( 'NONE', *, *, #48201, .T. ) ;
#1287 = CARTESIAN_POINT ( 'NONE',  ( -0.07591351300297340121, 3.346456692913386100, 0.2755905511810995412 ) ) ;
#1288 = LINE ( 'NONE', #41552, #16770 ) ;
#1289 = VECTOR ( 'NONE', #34121, 39.37007874015748143 ) ;
#1290 = VERTEX_POINT ( 'NONE', #30186 ) ;
#1291 = CARTESIAN_POINT ( 'NONE',  ( 2.009930929872536964, 5.118110236220475784, -0.8055662819783824258 ) ) ;
#1292 = VECTOR ( 'NONE', #43156, 39.37007874015748143 ) ;
#1293 = PLANE ( 'NONE',  #34468 ) ;
#1294 = ORIENTED_EDGE ( 'NONE', *, *, #28016, .F. ) ;
#1295 = ORIENTED_EDGE ( 'NONE', *, *, #4075, .F. ) ;
#1296 = VERTEX_POINT ( 'NONE', #45903 ) ;
#1297 = CARTESIAN_POINT ( 'NONE',  ( 2.043634885149959057, 2.755905511811027164, 0.7157624142946238388 ) ) ;
#1298 = FACE_OUTER_BOUND ( 'NONE', #33484, .T. ) ;
#1299 = LINE ( 'NONE', #28918, #4446 ) ;
#1300 = DIRECTION ( 'NONE',  ( -3.469446951953613696E-16, 0.000000000000000000, -1.000000000000000000 ) ) ;
#1301 = EDGE_LOOP ( 'NONE', ( #13180, #28397, #49854, #1740 ) ) ;
#1302 = VERTEX_POINT ( 'NONE', #10566 ) ;
#1303 = EDGE_CURVE ( 'NONE', #39809, #31903, #12592, .T. ) ;
#1304 = DIRECTION ( 'NONE',  ( 0.8584487936018655452, 1.288287287306305283E-16, 0.5128992774059071280 ) ) ;
#1305 = SURFACE_SIDE_STYLE ('',( #17320 ) ) ;
#1306 = EDGE_CURVE ( 'NONE', #33691, #7296, #460, .T. ) ;
#1307 = CARTESIAN_POINT ( 'NONE',  ( -1.909347346926324906, 3.346456692913386100, -1.102362204724405492 ) ) ;
#1308 = DIRECTION ( 'NONE',  ( -3.469446951953613696E-16, 0.000000000000000000, -1.000000000000000000 ) ) ;
#1309 = EDGE_CURVE ( 'NONE', #40155, #19068, #35328, .T. ) ;
#1310 = DIRECTION ( 'NONE',  ( 1.734723475976806848E-16, 0.000000000000000000, 1.000000000000000000 ) ) ;
#1311 = LINE ( 'NONE', #12418, #13606 ) ;
#1312 = EDGE_CURVE ( 'NONE', #41751, #18135, #36094, .T. ) ;
#1313 = DIRECTION ( 'NONE',  ( 0.000000000000000000, 1.000000000000000000, 0.000000000000000000 ) ) ;
#1314 = ORIENTED_EDGE ( 'NONE', *, *, #43415, .F. ) ;
#1315 = DIRECTION ( 'NONE',  ( 0.000000000000000000, 0.000000000000000000, -1.000000000000000000 ) ) ;
#1316 = LINE ( 'NONE', #17580, #7907 ) ;
#1317 = VECTOR ( 'NONE', #50449, 39.37007874015748143 ) ;
#1318 = B_SPLINE_CURVE_WITH_KNOTS ( 'NONE', 3,
 ( #4284, #20546, #16940, #48127 ),
 .UNSPECIFIED., .F., .F.,
 ( 4, 4 ),
 ( 0.001216554165443645879, 0.007368042712400780722 ),
 .UNSPECIFIED. ) ;
#1319 = VERTEX_POINT ( 'NONE', #4853 ) ;
#1320 = AXIS2_PLACEMENT_3D ( 'NONE', #11866, #19853, #35621 ) ;
#1321 = EDGE_LOOP ( 'NONE', ( #14358, #29914, #16565, #8986 ) ) ;
#1322 = LINE ( 'NONE', #44929, #7595 ) ;
#1323 = CARTESIAN_POINT ( 'NONE',  ( -1.363819533518803473, 3.232777166330603524, 2.047244094488179567 ) ) ;
#1324 = EDGE_CURVE ( 'NONE', #2307, #6610, #19855, .T. ) ;
#1325 = AXIS2_PLACEMENT_3D ( 'NONE', #17612, #33631, #45208 ) ;
#1326 = EDGE_LOOP ( 'NONE', ( #37731, #21247, #33641, #22836 ) ) ;
#1327 = AXIS2_PLACEMENT_3D ( 'NONE', #15441, #20052, #31187 ) ;
#1328 = EDGE_CURVE ( 'NONE', #49786, #32363, #35580, .T. ) ;
#1329 = VERTEX_POINT ( 'NONE', #4334 ) ;
#1330 = CARTESIAN_POINT ( 'NONE',  ( 2.182111253630085290, 3.267716535433071279, 0.6299212598425161236 ) ) ;
#1331 = EDGE_LOOP ( 'NONE', ( #34243, #8014 ) ) ;
#1332 = ORIENTED_EDGE ( 'NONE', *, *, #7973, .T. ) ;
#1333 = CARTESIAN_POINT ( 'NONE',  ( 0.000000000000000000, 0.000000000000000000, 0.000000000000000000 ) ) ;
#1334 = DIRECTION ( 'NONE',  ( -0.000000000000000000, 1.000000000000000000, -0.000000000000000000 ) ) ;
#1335 = ORIENTED_EDGE ( 'NONE', *, *, #8664, .F. ) ;
#1336 = VERTEX_POINT ( 'NONE', #47919 ) ;
#1337 = EDGE_LOOP ( 'NONE', ( #31562, #18762, #829, #6290 ) ) ;
#1338 = CARTESIAN_POINT ( 'NONE',  ( -0.5455278134075214336, 3.346456692913386100, -0.8267716535433049518 ) ) ;
#1339 = VERTEX_POINT ( 'NONE', #23956 ) ;
#1340 = VERTEX_POINT ( 'NONE', #43815 ) ;
#1341 = DIRECTION ( 'NONE',  ( 1.734723475976806848E-16, -0.000000000000000000, 1.000000000000000000 ) ) ;
#1342 = DIRECTION ( 'NONE',  ( -0.000000000000000000, -1.000000000000000000, -0.000000000000000000 ) ) ;
#1343 = CARTESIAN_POINT ( 'NONE',  ( 1.941690073511757264, 1.644018020651508039, 1.611391439051777397 ) ) ;
#1344 = EDGE_CURVE ( 'NONE', #28139, #15315, #50012, .T. ) ;
#1345 = EDGE_LOOP ( 'NONE', ( #14466, #13105, #2271, #43670 ) ) ;
#1346 = FACE_OUTER_BOUND ( 'NONE', #32458, .T. ) ;
#1347 = CARTESIAN_POINT ( 'NONE',  ( -1.091055626815042645, 3.346456692913386100, -0.8267716535433052849 ) ) ;
#1348 = DIRECTION ( 'NONE',  ( 1.734723475976806848E-16, -0.000000000000000000, 1.000000000000000000 ) ) ;
#1349 = CONICAL_SURFACE ( 'NONE', #24427, 2.165354330708661568, 0.2617993877991570129 ) ;
#1350 = VERTEX_POINT ( 'NONE', #4091 ) ;
#1351 = DIRECTION ( 'NONE',  ( -1.000000000000000000, 0.000000000000000000, -0.000000000000000000 ) ) ;
#1352 = DIRECTION ( 'NONE',  ( -1.000000000000000000, 0.000000000000000000, -0.000000000000000000 ) ) ;
#1353 = AXIS2_PLACEMENT_3D ( 'NONE', #21371, #9494, #21114 ) ;
#1354 = AXIS2_PLACEMENT_3D ( 'NONE', #33462, #21825, #37583 ) ;
#1355 = CYLINDRICAL_SURFACE ( 'NONE', #10134, 2.165354330708661568 ) ;
#1356 = ORIENTED_EDGE ( 'NONE', *, *, #31505, .T. ) ;
#1357 = EDGE_LOOP ( 'NONE', ( #4836, #40485, #13324, #36088 ) ) ;
#1358 = PLANE ( 'NONE',  #28689 ) ;
#1359 = CIRCLE ( 'NONE', #13716, 2.106299212598425008 ) ;
#1360 = DIRECTION ( 'NONE',  ( -0.000000000000000000, 1.000000000000000000, -0.000000000000000000 ) ) ;
#1361 = VECTOR ( 'NONE', #15893, 39.37007874015748143 ) ;
#1362 = CARTESIAN_POINT ( 'NONE',  ( 0.000000000000000000, 3.346456692913386100, 0.000000000000000000 ) ) ;
#1363 = LINE ( 'NONE', #24092, #9840 ) ;
#1364 = ORIENTED_EDGE ( 'NONE', *, *, #483, .T. ) ;
#1365 = VERTEX_POINT ( 'NONE', #12855 ) ;
#1366 = VECTOR ( 'NONE', #23366, 39.37007874015748143 ) ;
#1367 = EDGE_CURVE ( 'NONE', #42304, #46532, #29108, .T. ) ;
#1368 = LINE ( 'NONE', #32626, #40762 ) ;
#1369 = ORIENTED_EDGE ( 'NONE', *, *, #49691, .T. ) ;
#1370 = DIRECTION ( 'NONE',  ( -1.000000000000000000, 0.000000000000000000, 1.734723475976806848E-16 ) ) ;
#1371 = CARTESIAN_POINT ( 'NONE',  ( -0.8182917201112819283, 3.346456692913386100, 1.850393700787391849 ) ) ;
#1372 = EDGE_CURVE ( 'NONE', #32862, #32147, #47663, .T. ) ;
#1373 = EDGE_CURVE ( 'NONE', #37743, #48914, #20594, .T. ) ;
#1374 = EDGE_CURVE ( 'NONE', #23037, #1172, #36966, .T. ) ;
#1375 = PLANE ( 'NONE',  #9364 ) ;
#1376 = CARTESIAN_POINT ( 'NONE',  ( -0.6651440563933165295, 1.049866565067837820, 1.912327269821209486 ) ) ;
#1377 = CARTESIAN_POINT ( 'NONE',  ( 2.044241703397535748, 5.905511811023623991, -0.7159595814952628423 ) ) ;
#1378 = ORIENTED_EDGE ( 'NONE', *, *, #44567, .T. ) ;
#1379 = CARTESIAN_POINT ( 'NONE',  ( -1.651646936617113148, 1.205361022782829114E-17, 0.5883978091303396774 ) ) ;
#1380 = LINE ( 'NONE', #24881, #34779 ) ;
#1381 = ORIENTED_EDGE ( 'NONE', *, *, #45338, .T. ) ;
#1382 = FACE_OUTER_BOUND ( 'NONE', #42254, .T. ) ;
#1383 = CARTESIAN_POINT ( 'NONE',  ( -0.2727639067037607168, 3.267716535433071279, 4.731699523581612206E-17 ) ) ;
#1384 = ADVANCED_FACE ( 'NONE', ( #47408 ), #19561, .F. ) ;
#1385 = CYLINDRICAL_SURFACE ( 'NONE', #23000, 2.165354330708661568 ) ;
#1386 = ORIENTED_EDGE ( 'NONE', *, *, #5098, .F. ) ;
#1387 = VECTOR ( 'NONE', #5887, 39.37007874015748143 ) ;
#1388 = CARTESIAN_POINT ( 'NONE',  ( 2.318778318137675321, 1.461867355335562113, 1.828196727724137549 ) ) ;
#1389 = CARTESIAN_POINT ( 'NONE',  ( 1.015142113812069313, 0.000000000000000000, -1.299212598425193210 ) ) ;
#1390 = VECTOR ( 'NONE', #8484, 39.37007874015748143 ) ;
#1391 = ADVANCED_FACE ( 'NONE', ( #27818 ), #12339, .T. ) ;
#1392 = ORIENTED_EDGE ( 'NONE', *, *, #10069, .T. ) ;
#1393 = CARTESIAN_POINT ( 'NONE',  ( 1.823552992613439505, 0.03751337948320442039, -0.8329433802140283616 ) ) ;
#1394 = LINE ( 'NONE', #16384, #47596 ) ;
#1395 = VERTEX_POINT ( 'NONE', #20068 ) ;
#1396 = PLANE ( 'NONE',  #35293 ) ;
#1397 = PLANE ( 'NONE',  #49846 ) ;
#1398 = PLANE ( 'NONE',  #31292 ) ;
#1399 = CARTESIAN_POINT ( 'NONE',  ( -1.363819533518803473, 3.346456692913386100, -1.732283464566922726 ) ) ;
#1400 = CIRCLE ( 'NONE', #26130, 2.165354330708661568 ) ;
#1401 = ADVANCED_FACE ( 'NONE', ( #41191 ), #15697, .F. ) ;
#1402 = DIRECTION ( 'NONE',  ( -0.2660368455666826115, -1.118798511145731007E-16, 0.9639628606958511314 ) ) ;
#1403 = VECTOR ( 'NONE', #33369, 39.37007874015748143 ) ;
#1404 = EDGE_LOOP ( 'NONE', ( #33045, #20964, #12498, #39924 ) ) ;
#1405 = VERTEX_POINT ( 'NONE', #23697 ) ;
#1406 = LINE ( 'NONE', #1658, #31468 ) ;
#1407 = PLANE ( 'NONE',  #5666 ) ;
#1408 = ORIENTED_EDGE ( 'NONE', *, *, #4605, .T. ) ;
#1409 = FACE_OUTER_BOUND ( 'NONE', #9486, .T. ) ;
#1410 = CARTESIAN_POINT ( 'NONE',  ( -1.052882153225050521, 1.604404232578344303, 2.758709064509768716 ) ) ;
#1411 = DIRECTION ( 'NONE',  ( -3.469446951953613696E-16, 0.000000000000000000, -1.000000000000000000 ) ) ;
#1412 = EDGE_CURVE ( 'NONE', #16466, #39052, #35835, .T. ) ;
#1413 = LINE ( 'NONE', #40154, #1767 ) ;
#1414 = ORIENTED_EDGE ( 'NONE', *, *, #46798, .F. ) ;
#1415 = ORIENTED_EDGE ( 'NONE', *, *, #6430, .T. ) ;
#1416 = CARTESIAN_POINT ( 'NONE',  ( 1.363819533518803029, 0.000000000000000000, -1.929133858267710666 ) ) ;
#1417 = CARTESIAN_POINT ( 'NONE',  ( 0.000000000000000000, 0.3937007874015748254, 0.000000000000000000 ) ) ;
#1418 = LINE ( 'NONE', #33441, #21438 ) ;
#1419 = ORIENTED_EDGE ( 'NONE', *, *, #7625, .T. ) ;
#1420 = DIRECTION ( 'NONE',  ( 0.1342332658176667304, 1.288287287306305530E-16, -0.9909497617679332571 ) ) ;
#1421 = FACE_BOUND ( 'NONE', #15515, .T. ) ;
#1422 = EDGE_LOOP ( 'NONE', ( #48854, #9068, #24586, #5617 ) ) ;
#1423 = EDGE_CURVE ( 'NONE', #14385, #23466, #4592, .T. ) ;
#1424 = CARTESIAN_POINT ( 'NONE',  ( -0.2727639067037602727, 3.267716535433071279, 1.535433070866133898 ) ) ;
#1425 = VERTEX_POINT ( 'NONE', #46288 ) ;
#1426 = VERTEX_POINT ( 'NONE', #10449 ) ;
#1427 = DIRECTION ( 'NONE',  ( 1.734723475976806848E-16, 0.000000000000000000, 1.000000000000000000 ) ) ;
#1428 = ADVANCED_FACE ( 'NONE', ( #10192 ), #10577, .T. ) ;
#1429 = CIRCLE ( 'NONE', #12961, 1.743387098533651480 ) ;
#1430 = VECTOR ( 'NONE', #29772, 39.37007874015748143 ) ;
#1431 = ORIENTED_EDGE ( 'NONE', *, *, #17621, .T. ) ;
#1432 = CARTESIAN_POINT ( 'NONE',  ( 1.712499999125641770, 0.5249316475426859530, -0.7854770528406901375 ) ) ;
#1433 = ORIENTED_EDGE ( 'NONE', *, *, #4896, .T. ) ;
#1434 = AXIS2_PLACEMENT_3D ( 'NONE', #19771, #47873, #28542 ) ;
#1435 = CARTESIAN_POINT ( 'NONE',  ( -1.790681247139289889, 1.679220913509628543, -1.240985722462402352 ) ) ;
#1436 = DIRECTION ( 'NONE',  ( -0.000000000000000000, -1.000000000000000000, -0.000000000000000000 ) ) ;
#1437 = LINE ( 'NONE', #21826, #23418 ) ;
#1438 = EDGE_CURVE ( 'NONE', #4136, #10342, #34202, .T. ) ;
#1439 = CARTESIAN_POINT ( 'NONE',  ( -0.2727639067037602172, 3.346456692913386100, 0.7874015748031456541 ) ) ;
#1440 = EDGE_CURVE ( 'NONE', #20848, #17201, #14828, .T. ) ;
#1441 = CARTESIAN_POINT ( 'NONE',  ( -2.142325647309101022, 3.346456692913386100, -0.3149606299212589500 ) ) ;
#1442 = DIRECTION ( 'NONE',  ( -1.000000000000000000, 0.000000000000000000, 0.000000000000000000 ) ) ;
#1443 = VERTEX_POINT ( 'NONE', #26690 ) ;
#1444 = CARTESIAN_POINT ( 'NONE',  ( 0.000000000000000000, 3.267716535433071279, 1.377952755905504256 ) ) ;
#1445 = CONICAL_SURFACE ( 'NONE', #35355, 3.033577403570480779, 1.554780866114618743 ) ;
#1446 = CARTESIAN_POINT ( 'NONE',  ( -1.363819533518803029, 3.267716535433071279, -0.03937007874015868020 ) ) ;
#1447 = EDGE_LOOP ( 'NONE', ( #36747, #1419, #41092, #39920 ) ) ;
#1448 = CARTESIAN_POINT ( 'NONE',  ( 3.937007874015748143, 5.118110236220475784, -1.181102362204724310 ) ) ;
#1449 = DIRECTION ( 'NONE',  ( -0.000000000000000000, 1.000000000000000000, -0.000000000000000000 ) ) ;
#1450 = ORIENTED_EDGE ( 'NONE', *, *, #40215, .T. ) ;
#1451 = DIRECTION ( 'NONE',  ( 1.000000000000000000, 0.000000000000000000, 0.000000000000000000 ) ) ;
#1452 = DIRECTION ( 'NONE',  ( 1.734723475976806848E-16, -0.000000000000000000, 1.000000000000000000 ) ) ;
#1453 = LINE ( 'NONE', #5838, #41719 ) ;
#1454 = ORIENTED_EDGE ( 'NONE', *, *, #28750, .F. ) ;
#1455 = CARTESIAN_POINT ( 'NONE',  ( -1.985260859929298016, 3.346456692913386100, -0.6299212598425177889 ) ) ;
#1456 = ORIENTED_EDGE ( 'NONE', *, *, #18152, .T. ) ;
#1457 = FACE_BOUND ( 'NONE', #25360, .T. ) ;
#1458 = CARTESIAN_POINT ( 'NONE',  ( -1.166969139818015977, 0.000000000000000000, -1.732283464566922726 ) ) ;
#1459 = LINE ( 'NONE', #49673, #20174 ) ;
#1460 = LINE ( 'NONE', #32465, #21016 ) ;
#1461 = AXIS2_PLACEMENT_3D ( 'NONE', #11426, #8307, #26907 ) ;
#1462 = AXIS2_PLACEMENT_3D ( 'NONE', #47954, #8246, #20103 ) ;
#1463 = EDGE_CURVE ( 'NONE', #9823, #30686, #41688, .T. ) ;
#1464 = VERTEX_POINT ( 'NONE', #45529 ) ;
#1465 = ORIENTED_EDGE ( 'NONE', *, *, #35217, .T. ) ;
#1466 = CARTESIAN_POINT ( 'NONE',  ( 1.312248418042880171, 5.905511811023623991, -1.722429524498088727 ) ) ;
#1467 = ORIENTED_EDGE ( 'NONE', *, *, #35053, .T. ) ;
#1468 = CIRCLE ( 'NONE', #2320, 2.244934639244525076 ) ;
#1469 = LINE ( 'NONE', #41231, #13722 ) ;
#1470 = ORIENTED_EDGE ( 'NONE', *, *, #10486, .F. ) ;
#1471 = EDGE_CURVE ( 'NONE', #50937, #42335, #30310, .T. ) ;
#1472 = LINE ( 'NONE', #48168, #1735 ) ;
#1473 = EDGE_CURVE ( 'NONE', #12064, #14934, #38077, .T. ) ;
#1474 = ORIENTED_EDGE ( 'NONE', *, *, #15341, .T. ) ;
#1475 = CARTESIAN_POINT ( 'NONE',  ( 2.254349126581632667, 1.678392680027759321, -0.5650186692295513513 ) ) ;
#1476 = ADVANCED_FACE ( 'NONE', ( #34453 ), #45784, .F. ) ;
#1477 = AXIS2_PLACEMENT_3D ( 'NONE', #14187, #37188, #5686 ) ;
#1478 = DIRECTION ( 'NONE',  ( 1.000000000000000000, 0.000000000000000000, 0.000000000000000000 ) ) ;
#1479 = ORIENTED_EDGE ( 'NONE', *, *, #12340, .F. ) ;
#1480 = ADVANCED_FACE ( 'NONE', ( #37572 ), #33706, .F. ) ;
#1481 = DIRECTION ( 'NONE',  ( 1.000000000000000000, 0.000000000000000000, 0.000000000000000000 ) ) ;
#1482 = ORIENTED_EDGE ( 'NONE', *, *, #49175, .T. ) ;
#1483 = ORIENTED_EDGE ( 'NONE', *, *, #43029, .F. ) ;
#1484 = VECTOR ( 'NONE', #23849, 39.37007874015748143 ) ;
#1485 = EDGE_LOOP ( 'NONE', ( #11618, #41738, #39037, #40316 ) ) ;
#1486 = VERTEX_POINT ( 'NONE', #26190 ) ;
#1487 = DIRECTION ( 'NONE',  ( -0.000000000000000000, 1.000000000000000000, -0.000000000000000000 ) ) ;
#1488 = LINE ( 'NONE', #43185, #46966 ) ;
#1489 = ORIENTED_EDGE ( 'NONE', *, *, #18040, .F. ) ;
#1490 = CARTESIAN_POINT ( 'NONE',  ( -1.091055626815042645, 3.346456692913386100, -1.889763779527552146 ) ) ;
#1491 = VERTEX_POINT ( 'NONE', #49138 ) ;
#1492 = CARTESIAN_POINT ( 'NONE',  ( -2.823445274216743073, 1.576824725690453954, 0.8656477926280276014 ) ) ;
#1493 = ADVANCED_FACE ( 'NONE', ( #49888 ), #34498, .T. ) ;
#1494 = VECTOR ( 'NONE', #27663, 39.37007874015748143 ) ;
#1495 = CIRCLE ( 'NONE', #19606, 0.8858267716535433989 ) ;
#1496 = FACE_OUTER_BOUND ( 'NONE', #44181, .T. ) ;
#1497 = EDGE_CURVE ( 'NONE', #15782, #13966, #2354, .T. ) ;
#1498 = ORIENTED_EDGE ( 'NONE', *, *, #4933, .F. ) ;
#1499 = CARTESIAN_POINT ( 'NONE',  ( -1.636583440222563635, 3.267716535433071279, 0.3149606299212578953 ) ) ;
#1500 = CARTESIAN_POINT ( 'NONE',  ( -1.210465362316797577, 0.005745789993395570075, 1.310690939022672863 ) ) ;
#1501 = ADVANCED_FACE ( 'NONE', ( #30321 ), #9943, .F. ) ;
#1502 = EDGE_LOOP ( 'NONE', ( #31771, #38803, #42664, #49372 ) ) ;
#1503 = LINE ( 'NONE', #17260, #1060 ) ;
#1504 = CARTESIAN_POINT ( 'NONE',  ( 0.8182917201112819283, 0.000000000000000000, 0.7874015748031454320 ) ) ;
#1505 = CIRCLE ( 'NONE', #22115, 2.106299212598425008 ) ;
#1506 = CARTESIAN_POINT ( 'NONE',  ( 0.7423782071083092626, 3.267716535433071279, 2.204724409448808764 ) ) ;
#1507 = DIRECTION ( 'NONE',  ( 0.000000000000000000, -1.000000000000000000, 0.000000000000000000 ) ) ;
#1508 = CLOSED_SHELL ( 'NONE', ( #28593, #303, #12996, #41709, #31234, #38345, #40645, #40838, #42452, #45401, #8257, #49683, #4822, #954, #35208, #27540, #18593, #49621, #27006, #21376, #42691, #51026 ) ) ;
#1509 = VECTOR ( 'NONE', #3169, 39.37007874015748143 ) ;
#1510 = PLANE ( 'NONE',  #100 ) ;
#1511 = ORIENTED_EDGE ( 'NONE', *, *, #45175, .T. ) ;
#1512 = DIRECTION ( 'NONE',  ( -1.000000000000000000, 0.000000000000000000, -0.000000000000000000 ) ) ;
#1514 = EDGE_CURVE ( 'NONE', #39073, #15435, #17686, .T. ) ;
#1513 = LINE ( 'NONE', #25260, #357 ) ;
#1515 = AXIS2_PLACEMENT_3D ( 'NONE', #11770, #3779, #19010 ) ;
#1516 = VERTEX_POINT ( 'NONE', #6583 ) ;
#1517 = CARTESIAN_POINT ( 'NONE',  ( 0.7145799201508782339, 6.692913385826772199, 2.044048657746659448 ) ) ;
#1518 = VECTOR ( 'NONE', #37521, 39.37007874015748143 ) ;
#1519 = ORIENTED_EDGE ( 'NONE', *, *, #19813, .F. ) ;
#1520 = CARTESIAN_POINT ( 'NONE',  ( 1.588513588560381828, 0.05336261777518135074, -1.107536019441389019 ) ) ;
#1521 = CARTESIAN_POINT ( 'NONE',  ( -2.882374421592805103, 1.674323616330495756, -0.6410571176644951352 ) ) ;
#1522 = DIRECTION ( 'NONE',  ( 1.734723475976806848E-16, -0.000000000000000000, 1.000000000000000000 ) ) ;
#1523 = LINE ( 'NONE', #47955, #33336 ) ;
#1524 = LINE ( 'NONE', #1007, #42561 ) ;
#1525 = ORIENTED_EDGE ( 'NONE', *, *, #27749, .T. ) ;
#1526 = PLANE ( 'NONE',  #10949 ) ;
#1527 = LINE ( 'NONE', #1778, #6484 ) ;
#1528 = VERTEX_POINT ( 'NONE', #30068 ) ;
#1529 = CARTESIAN_POINT ( 'NONE',  ( -0.2156685157583834722, 0.000000000000000000, -2.945280361644576850 ) ) ;
#1530 = ORIENTED_EDGE ( 'NONE', *, *, #41636, .F. ) ;
#1531 = LINE ( 'NONE', #5402, #7913 ) ;
#1532 = LINE ( 'NONE', #13407, #45345 ) ;
#1533 = EDGE_CURVE ( 'NONE', #10313, #9920, #115, .T. ) ;
#1534 = VECTOR ( 'NONE', #39883, 39.37007874015748143 ) ;
#1535 = DIRECTION ( 'NONE',  ( 0.4738686624730094610, 1.288287287306305530E-16, -0.8805955318567322276 ) ) ;
#1536 = ADVANCED_FACE ( 'NONE', ( #25680 ), #6062, .F. ) ;
#1537 = ADVANCED_FACE ( 'NONE', ( #42687 ), #22828, .F. ) ;
#1538 = B_SPLINE_CURVE_WITH_KNOTS ( 'NONE', 3,
 ( #11647, #43124, #23514, #39267 ),
 .UNSPECIFIED., .F., .F.,
 ( 4, 4 ),
 ( 0.01072160763103902591, 0.03073581401287817788 ),
 .UNSPECIFIED. ) ;
#1539 = CARTESIAN_POINT ( 'NONE',  ( -2.734482843737247038, 1.676638068352269029, -1.115254632218712016 ) ) ;
#1540 = ORIENTED_EDGE ( 'NONE', *, *, #13965, .T. ) ;
#1541 = ORIENTED_EDGE ( 'NONE', *, *, #43831, .T. ) ;
#1542 = DIRECTION ( 'NONE',  ( -3.986037398843765983E-20, -1.000000000000000000, -1.160734090543304660E-16 ) ) ;
#1543 = CARTESIAN_POINT ( 'NONE',  ( -2.339241080213612545, 1.564176246289736616, 1.802537235681883843 ) ) ;
#1544 = FACE_BOUND ( 'NONE', #39627, .T. ) ;
#1545 = ORIENTED_EDGE ( 'NONE', *, *, #36924, .T. ) ;
#1546 = AXIS2_PLACEMENT_3D ( 'NONE', #21283, #33427, #17156 ) ;
#1547 = CARTESIAN_POINT ( 'NONE',  ( 1.091055626815042645, 3.346456692913386100, 1.259842519685033357 ) ) ;
#1548 = LINE ( 'NONE', #17803, #48888 ) ;
#1549 = ORIENTED_EDGE ( 'NONE', *, *, #42560, .T. ) ;
#1550 = VECTOR ( 'NONE', #16550, 39.37007874015748143 ) ;
#1551 = CARTESIAN_POINT ( 'NONE',  ( -2.182111253630085290, 3.267716535433071279, 0.9448818897637749625 ) ) ;
#1552 = CARTESIAN_POINT ( 'NONE',  ( -0.07591351300297340121, 0.000000000000000000, -0.6692913385826758654 ) ) ;
#1553 = VERTEX_POINT ( 'NONE', #7833 ) ;
#1554 = ORIENTED_EDGE ( 'NONE', *, *, #36695, .T. ) ;
#1555 = EDGE_CURVE ( 'NONE', #37961, #7571, #46783, .T. ) ;
#1556 = VECTOR ( 'NONE', #7667, 39.37007874015748143 ) ;
#1557 = ORIENTED_EDGE ( 'NONE', *, *, #18332, .T. ) ;
#1558 = CARTESIAN_POINT ( 'NONE',  ( 4.268512490100411402E-16, 0.000000000000000000, 1.259842519685033357 ) ) ;
#1559 = CARTESIAN_POINT ( 'NONE',  ( 0.8329809839909850799, 1.732245219823249638, -2.833254665166554442 ) ) ;
#1560 = ADVANCED_FACE ( 'NONE', ( #38827 ), #34700, .T. ) ;
#1561 = LINE ( 'NONE', #24539, #31653 ) ;
#1562 = FACE_OUTER_BOUND ( 'NONE', #9879, .T. ) ;
#1563 = EDGE_CURVE ( 'NONE', #20663, #2264, #50884, .T. ) ;
#1564 = ORIENTED_EDGE ( 'NONE', *, *, #13652, .T. ) ;
#1565 = ORIENTED_EDGE ( 'NONE', *, *, #37179, .T. ) ;
#1566 = CARTESIAN_POINT ( 'NONE',  ( -1.531732224425391253, 1.205361022782829114E-17, 0.8801458454442117052 ) ) ;
#1567 = CARTESIAN_POINT ( 'NONE',  ( -2.878724150143177507, 0.000000000000000000, -0.6570500018395228903 ) ) ;
#1568 = EDGE_CURVE ( 'NONE', #14018, #21172, #31081, .T. ) ;
#1569 = LINE ( 'NONE', #21447, #24143 ) ;
#1570 = DIRECTION ( 'NONE',  ( -0.5128992774058949156, 0.000000000000000000, -0.8584487936018728726 ) ) ;
#1571 = CARTESIAN_POINT ( 'NONE',  ( 1.363819533518803251, 0.000000000000000000, -0.3543307086614178592 ) ) ;
#1572 = CARTESIAN_POINT ( 'NONE',  ( 0.1067246931122726866, 0.02962905676920215767, 0.000000000000000000 ) ) ;
#1573 = VECTOR ( 'NONE', #27421, 39.37007874015748143 ) ;
#1574 = LINE ( 'NONE', #41080, #47272 ) ;
#1575 = ORIENTED_EDGE ( 'NONE', *, *, #47162, .T. ) ;
#1576 = CARTESIAN_POINT ( 'NONE',  ( -1.091055626815042201, 0.000000000000000000, 1.377952755905504256 ) ) ;
#1577 = DIRECTION ( 'NONE',  ( 0.000000000000000000, 0.000000000000000000, -1.000000000000000000 ) ) ;
#1578 = VERTEX_POINT ( 'NONE', #35709 ) ;
#1579 = ORIENTED_EDGE ( 'NONE', *, *, #15201, .F. ) ;
#1580 = VECTOR ( 'NONE', #29287, 39.37007874015748143 ) ;
#1582 = FACE_OUTER_BOUND ( 'NONE', #36479, .T. ) ;
#1581 = AXIS2_PLACEMENT_3D ( 'NONE', #2961, #22331, #45285 ) ;
#1583 = PLANE ( 'NONE',  #13002 ) ;
#1584 = VERTEX_POINT ( 'NONE', #50386 ) ;
#1585 = AXIS2_PLACEMENT_3D ( 'NONE', #26722, #41973, #14607 ) ;
#1586 = ORIENTED_EDGE ( 'NONE', *, *, #43598, .F. ) ;
#1587 = DIRECTION ( 'NONE',  ( -0.000000000000000000, 1.000000000000000000, -0.000000000000000000 ) ) ;
#1588 = VECTOR ( 'NONE', #4753, 39.37007874015748143 ) ;
#1589 = EDGE_LOOP ( 'NONE', ( #50913, #7896, #28381, #9176, #15019 ) ) ;
#1590 = CARTESIAN_POINT ( 'NONE',  ( -1.909347346926324906, 0.000000000000000000, 1.220472440944875059 ) ) ;
#1591 = CARTESIAN_POINT ( 'NONE',  ( -0.3486774197067334935, 3.346456692913386100, 1.062992125984246083 ) ) ;
#1592 = ORIENTED_EDGE ( 'NONE', *, *, #8241, .F. ) ;
#1593 = EDGE_CURVE ( 'NONE', #20677, #16212, #43533, .T. ) ;
#1594 = EDGE_LOOP ( 'NONE', ( #7957, #25281, #38663, #22736 ) ) ;
#1595 = ORIENTED_EDGE ( 'NONE', *, *, #15115, .T. ) ;
#1596 = LINE ( 'NONE', #40340, #9833 ) ;
#1597 = EDGE_CURVE ( 'NONE', #26915, #40703, #29559, .T. ) ;
#1598 = ORIENTED_EDGE ( 'NONE', *, *, #35690, .T. ) ;
#1599 = VERTEX_POINT ( 'NONE', #39075 ) ;
#1600 = LINE ( 'NONE', #18365, #23163 ) ;
#1601 = CARTESIAN_POINT ( 'NONE',  ( 0.8182917201112819283, 3.267716535433071279, -0.3543307086614175816 ) ) ;
#1602 = CARTESIAN_POINT ( 'NONE',  ( -1.166969139818015755, 3.346456692913386100, 1.220472440944875281 ) ) ;
#1603 = EDGE_CURVE ( 'NONE', #50064, #21920, #50634, .T. ) ;
#1604 = VERTEX_POINT ( 'NONE', #15328 ) ;
#1605 = DIRECTION ( 'NONE',  ( -3.469446951953613696E-16, 0.000000000000000000, -1.000000000000000000 ) ) ;
#1606 = DIRECTION ( 'NONE',  ( 1.000000000000000000, 0.000000000000000000, 0.000000000000000000 ) ) ;
#1607 = CONICAL_SURFACE ( 'NONE', #30470, 2.165354330708661568, 0.2617993877991570129 ) ;
#1608 = CARTESIAN_POINT ( 'NONE',  ( 2.011572120637293626, 1.747067225219576247, -1.855173337549795187 ) ) ;
#1609 = ORIENTED_EDGE ( 'NONE', *, *, #38867, .T. ) ;
#1610 = CARTESIAN_POINT ( 'NONE',  ( 3.927031490892378253E-16, 3.267716535433071279, 1.062992125984246083 ) ) ;
#1611 = DIRECTION ( 'NONE',  ( 0.000000000000000000, -1.000000000000000000, 0.000000000000000000 ) ) ;
#1612 = DIRECTION ( 'NONE',  ( 1.000000000000000000, 0.000000000000000000, 0.000000000000000000 ) ) ;
#1613 = ORIENTED_EDGE ( 'NONE', *, *, #5854, .F. ) ;
#1614 = EDGE_LOOP ( 'NONE', ( #22471, #18066, #13906, #37039 ) ) ;
#1615 = VECTOR ( 'NONE', #32821, 39.37007874015748143 ) ;
#1616 = CARTESIAN_POINT ( 'NONE',  ( -0.07591351300297340121, 0.000000000000000000, -0.9842519685039344823 ) ) ;
#1617 = EDGE_CURVE ( 'NONE', #31137, #15706, #11703, .T. ) ;
#1618 = CARTESIAN_POINT ( 'NONE',  ( -1.133754555558240673, 0.009760511380980992774, 1.372484652545675532 ) ) ;
#1619 = DIRECTION ( 'NONE',  ( -0.000000000000000000, 1.000000000000000000, -0.000000000000000000 ) ) ;
#1620 = B_SPLINE_CURVE_WITH_KNOTS ( 'NONE', 3,
 ( #24104, #15413, #31156, #46864 ),
 .UNSPECIFIED., .F., .F.,
 ( 4, 4 ),
 ( 0.001733726700897485554, 0.004233787427253475795 ),
 .UNSPECIFIED. ) ;
#1621 = VERTEX_POINT ( 'NONE', #15824 ) ;
#1622 = VERTEX_POINT ( 'NONE', #3453 ) ;
#1623 = EDGE_CURVE ( 'NONE', #6479, #17812, #34954, .T. ) ;
#1624 = DIRECTION ( 'NONE',  ( -8.021399753802198224E-17, -1.000000000000000000, 8.389726389140549123E-17 ) ) ;
#1625 = AXIS2_PLACEMENT_3D ( 'NONE', #18800, #12252, #34552 ) ;
#1626 = VERTEX_POINT ( 'NONE', #16088 ) ;
#1627 = DIRECTION ( 'NONE',  ( 1.734723475976806848E-16, -0.000000000000000000, 1.000000000000000000 ) ) ;
#1628 = CARTESIAN_POINT ( 'NONE',  ( -0.6214413264104945434, 3.267716535433071279, -0.4724409448818886470 ) ) ;
#1629 = DIRECTION ( 'NONE',  ( -1.000000000000000000, 0.000000000000000000, 1.734723475976806848E-16 ) ) ;
#1630 = DIRECTION ( 'NONE',  ( -3.469446951953613696E-16, 0.000000000000000000, -1.000000000000000000 ) ) ;
#1631 = LINE ( 'NONE', #45228, #6467 ) ;
#1632 = ORIENTED_EDGE ( 'NONE', *, *, #21926, .T. ) ;
#1633 = CARTESIAN_POINT ( 'NONE',  ( 1.556712866041120247, 1.645058926882370542, 2.509548638715870084 ) ) ;
#1634 = CARTESIAN_POINT ( 'NONE',  ( 1.091055626815043311, 3.346456692913386100, 1.692913385826762873 ) ) ;
#1635 = ORIENTED_EDGE ( 'NONE', *, *, #24237, .F. ) ;
#1636 = DIRECTION ( 'NONE',  ( -0.000000000000000000, 0.000000000000000000, 1.000000000000000000 ) ) ;
#1637 = FACE_OUTER_BOUND ( 'NONE', #29391, .T. ) ;
#1638 = FACE_OUTER_BOUND ( 'NONE', #3691, .T. ) ;
#1639 = VECTOR ( 'NONE', #38324, 39.37007874015748143 ) ;
#1640 = VERTEX_POINT ( 'NONE', #7082 ) ;
#1641 = LINE ( 'NONE', #34358, #40692 ) ;
#1642 = LINE ( 'NONE', #41399, #24250 ) ;
#1643 = B_SPLINE_CURVE_WITH_KNOTS ( 'NONE', 3,
 ( #17921, #45508, #10929, #2676 ),
 .UNSPECIFIED., .F., .F.,
 ( 4, 4 ),
 ( 0.1211873102087489551, 0.1625992483279400380 ),
 .UNSPECIFIED. ) ;
#1644 = VERTEX_POINT ( 'NONE', #27442 ) ;
#1645 = CARTESIAN_POINT ( 'NONE',  ( -1.181102362204724310, 0.4724409448818890911, -1.062992125984252079 ) ) ;
#1646 = DIRECTION ( 'NONE',  ( 0.000000000000000000, -1.000000000000000000, 0.000000000000000000 ) ) ;
#1647 = EDGE_LOOP ( 'NONE', ( #27290, #42930, #46936, #29764 ) ) ;
#1648 = CARTESIAN_POINT ( 'NONE',  ( 0.8182917201112818173, 3.267716535433071279, -1.419509857074483292E-16 ) ) ;
#1649 = AXIS2_PLACEMENT_3D ( 'NONE', #34585, #15464, #50270 ) ;
#1650 = CARTESIAN_POINT ( 'NONE',  ( 0.002207914879453961969, 6.692913385826772199, 0.04916304461325451958 ) ) ;
#1651 = CARTESIAN_POINT ( 'NONE',  ( 2.951990591674676256, 1.447429260878886348, -0.08331184815398369470 ) ) ;
#1652 = DIRECTION ( 'NONE',  ( -1.000000000000000000, 0.000000000000000000, -0.000000000000000000 ) ) ;
#1653 = AXIS2_PLACEMENT_3D ( 'NONE', #8598, #40608, #16607 ) ;
#1654 = LINE ( 'NONE', #9919, #37011 ) ;
#1655 = EDGE_CURVE ( 'NONE', #26751, #21978, #78, .T. ) ;
#1656 = EDGE_LOOP ( 'NONE', ( #12447, #32100, #28299, #8685, #10616, #25805, #37861, #14269, #42208, #17936, #12091, #47471, #21734 ) ) ;
#1657 = ORIENTED_EDGE ( 'NONE', *, *, #42499, .F. ) ;
#1658 = CARTESIAN_POINT ( 'NONE',  ( -1.377952755905510918, 0.000000000000000000, -4.133858267716536083 ) ) ;
#1659 = LINE ( 'NONE', #17410, #31240 ) ;
#1660 = ADVANCED_FACE ( 'NONE', ( #30830 ), #27871, .T. ) ;
#1661 = EDGE_LOOP ( 'NONE', ( #33119, #48791, #28504, #6328 ) ) ;
#1662 = LINE ( 'NONE', #14296, #39914 ) ;
#1663 = LINE ( 'NONE', #25160, #17034 ) ;
#1664 = AXIS2_PLACEMENT_3D ( 'NONE', #17091, #44942, #28694 ) ;
#1665 = CARTESIAN_POINT ( 'NONE',  ( 2.459496094709723302, 1.652223989028923867, -0.6118421259957096403 ) ) ;
#1666 = EDGE_CURVE ( 'NONE', #11390, #7825, #23318, .T. ) ;
#1667 = DIRECTION ( 'NONE',  ( -0.9998717552508121775, -0.01601477604151182316, 0.000000000000000000 ) ) ;
#1668 = EDGE_LOOP ( 'NONE', ( #22130, #30241, #19115, #25345 ) ) ;
#1669 = ORIENTED_EDGE ( 'NONE', *, *, #12384, .T. ) ;
#1670 = EDGE_CURVE ( 'NONE', #44829, #1816, #12215, .T. ) ;
#1671 = CARTESIAN_POINT ( 'NONE',  ( -0.2430652128771638720, 6.692913385826772199, -2.151668812760861194 ) ) ;
#1672 = LINE ( 'NONE', #45024, #35703 ) ;
#1673 = DIRECTION ( 'NONE',  ( -0.000000000000000000, 1.000000000000000000, -0.000000000000000000 ) ) ;
#1674 = ADVANCED_FACE ( 'NONE', ( #11206 ), #38579, .F. ) ;
#1675 = VERTEX_POINT ( 'NONE', #7336 ) ;
#1676 = LINE ( 'NONE', #22319, #43793 ) ;
#1677 = FACE_BOUND ( 'NONE', #2315, .T. ) ;
#1678 = VERTEX_POINT ( 'NONE', #23079 ) ;
#1679 = CARTESIAN_POINT ( 'NONE',  ( 2.277873973731426194, 1.754757658573260048, 1.879489153247668076 ) ) ;
#1680 = EDGE_LOOP ( 'NONE', ( #9632, #27406, #21404, #44753 ) ) ;
#1681 = VERTEX_POINT ( 'NONE', #8341 ) ;
#1682 = DIRECTION ( 'NONE',  ( 1.000000000000000000, 0.000000000000000000, -3.469446951953613696E-16 ) ) ;
#1683 = EDGE_CURVE ( 'NONE', #28119, #24628, #44465, .T. ) ;
#1684 = ORIENTED_EDGE ( 'NONE', *, *, #36213, .T. ) ;
#1685 = CARTESIAN_POINT ( 'NONE',  ( 2.100227814008711835, 1.751990118145921649, -2.076109931251913565 ) ) ;
#1686 = DIRECTION ( 'NONE',  ( 1.156482317317871478E-16, 0.000000000000000000, 1.000000000000000000 ) ) ;
#1687 = ORIENTED_EDGE ( 'NONE', *, *, #19498, .T. ) ;
#1688 = EDGE_CURVE ( 'NONE', #40324, #7249, #40096, .T. ) ;
#1689 = PLANE ( 'NONE',  #49156 ) ;
#1690 = DIRECTION ( 'NONE',  ( 1.734723475976806848E-16, -0.000000000000000000, 1.000000000000000000 ) ) ;
#1691 = VECTOR ( 'NONE', #12297, 39.37007874015748143 ) ;
#1692 = AXIS2_PLACEMENT_3D ( 'NONE', #10784, #6664, #49473 ) ;
#1693 = EDGE_CURVE ( 'NONE', #39686, #6600, #20983, .T. ) ;
#1694 = CARTESIAN_POINT ( 'NONE',  ( -1.909347346926324906, 3.346456692913386100, -0.4724409448818884805 ) ) ;
#1695 = B_SPLINE_CURVE_WITH_KNOTS ( 'NONE', 3,
 ( #11503, #46583, #23624, #18992 ),
 .UNSPECIFIED., .F., .F.,
 ( 4, 4 ),
 ( 0.0002252789032484298071, 0.002725386641250519913 ),
 .UNSPECIFIED. ) ;
#1696 = CARTESIAN_POINT ( 'NONE',  ( -0.04921259842519695726, 0.5231837827169103505, 2.213767285547495689 ) ) ;
#1697 = CARTESIAN_POINT ( 'NONE',  ( -1.091055626815042645, 0.000000000000000000, -0.1968503937007881899 ) ) ;
#1698 = EDGE_LOOP ( 'NONE', ( #13563, #37310, #36206, #29821 ) ) ;
#1699 = DIRECTION ( 'NONE',  ( 3.986037398843765983E-20, 1.000000000000000000, 1.160734090543304660E-16 ) ) ;
#1700 = VECTOR ( 'NONE', #46148, 39.37007874015748854 ) ;
#1701 = EDGE_CURVE ( 'NONE', #46418, #14938, #36737, .T. ) ;
#1702 = CARTESIAN_POINT ( 'NONE',  ( -1.166969139818015977, 0.000000000000000000, 2.047244094488179567 ) ) ;
#1703 = ORIENTED_EDGE ( 'NONE', *, *, #563, .T. ) ;
#1704 = DIRECTION ( 'NONE',  ( -0.000000000000000000, 1.000000000000000000, -0.000000000000000000 ) ) ;
#1705 = DIRECTION ( 'NONE',  ( 0.000000000000000000, 1.160734090543304660E-16, -1.000000000000000000 ) ) ;
#1706 = VERTEX_POINT ( 'NONE', #12728 ) ;
#1707 = DIRECTION ( 'NONE',  ( -3.986037398843765983E-20, -1.000000000000000000, -1.160734090543304660E-16 ) ) ;
#1708 = DIRECTION ( 'NONE',  ( -1.000000000000000000, -0.000000000000000000, -0.000000000000000000 ) ) ;
#1709 = CARTESIAN_POINT ( 'NONE',  ( 0.5905511811023621549, 0.000000000000000000, -4.133858267716536083 ) ) ;
#1710 = EDGE_LOOP ( 'NONE', ( #22231, #19484, #9226, #49238 ) ) ;
#1711 = LINE ( 'NONE', #41721, #35410 ) ;
#1712 = ORIENTED_EDGE ( 'NONE', *, *, #9689, .F. ) ;
#1713 = FACE_BOUND ( 'NONE', #5681, .T. ) ;
#1714 = PLANE ( 'NONE',  #46503 ) ;
#1715 = DIRECTION ( 'NONE',  ( -3.469446951953613696E-16, 0.000000000000000000, -1.000000000000000000 ) ) ;
#1716 = CARTESIAN_POINT ( 'NONE',  ( -2.142325647309101022, 3.267716535433071279, 0.3149606299212578953 ) ) ;
#1717 = ORIENTED_EDGE ( 'NONE', *, *, #34571, .T. ) ;
#1718 = EDGE_LOOP ( 'NONE', ( #24085, #45191, #49058, #2610 ) ) ;
#1719 = CARTESIAN_POINT ( 'NONE',  ( 0.8182917201112824834, 3.346456692913386100, 1.940849049717691122 ) ) ;
#1720 = EDGE_LOOP ( 'NONE', ( #15430, #29294, #8810, #43817 ) ) ;
#1721 = CARTESIAN_POINT ( 'NONE',  ( -0.8942052331142552601, 0.000000000000000000, -0.5118110236220467790 ) ) ;
#1722 = EDGE_LOOP ( 'NONE', ( #36845, #4176, #19214, #50603 ) ) ;
#1723 = EDGE_CURVE ( 'NONE', #43780, #14810, #36228, .T. ) ;
#1724 = AXIS2_PLACEMENT_3D ( 'NONE', #17826, #2082, #41078 ) ;
#1725 = DIRECTION ( 'NONE',  ( -1.000000000000000000, 0.000000000000000000, 1.734723475976806848E-16 ) ) ;
#1726 = VECTOR ( 'NONE', #37882, 39.37007874015748143 ) ;
#1727 = EDGE_CURVE ( 'NONE', #31288, #35644, #1505, .T. ) ;
#1728 = EDGE_LOOP ( 'NONE', ( #7265, #35678, #33944, #14815 ) ) ;
#1729 = LINE ( 'NONE', #48922, #40615 ) ;
#1730 = EDGE_CURVE ( 'NONE', #48222, #50396, #16606, .T. ) ;
#1731 = CARTESIAN_POINT ( 'NONE',  ( 1.491455157018016342, 0.000000000000000000, -1.448759626580099713 ) ) ;
#1732 = ORIENTED_EDGE ( 'NONE', *, *, #8597, .F. ) ;
#1733 = CARTESIAN_POINT ( 'NONE',  ( 0.1968503937007870241, 0.000000000000000000, -1.889763779527552146 ) ) ;
#1734 = EDGE_LOOP ( 'NONE', ( #5848, #18849, #49497, #13190 ) ) ;
#1735 = VECTOR ( 'NONE', #32990, 39.37007874015748143 ) ;
#1736 = ORIENTED_EDGE ( 'NONE', *, *, #21469, .T. ) ;
#1737 = ORIENTED_EDGE ( 'NONE', *, *, #27170, .T. ) ;
#1738 = ORIENTED_EDGE ( 'NONE', *, *, #37835, .T. ) ;
#1739 = FACE_OUTER_BOUND ( 'NONE', #27866, .T. ) ;
#1740 = ORIENTED_EDGE ( 'NONE', *, *, #17841, .F. ) ;
#1741 = DIRECTION ( 'NONE',  ( 1.000000000000000000, 0.000000000000000000, -3.469446951953613696E-16 ) ) ;
#1742 = ORIENTED_EDGE ( 'NONE', *, *, #31920, .T. ) ;
#1743 = FACE_OUTER_BOUND ( 'NONE', #34807, .T. ) ;
#1744 = ADVANCED_FACE ( 'NONE', ( #4979 ), #1358, .F. ) ;
#1745 = CARTESIAN_POINT ( 'NONE',  ( -1.152895553066196399, 5.905511811023623991, -1.833672301139088079 ) ) ;
#1746 = VERTEX_POINT ( 'NONE', #4727 ) ;
#1747 = DIRECTION ( 'NONE',  ( -3.469446951953613696E-16, 0.000000000000000000, -1.000000000000000000 ) ) ;
#1748 = FACE_OUTER_BOUND ( 'NONE', #35742, .T. ) ;
#1749 = VERTEX_POINT ( 'NONE', #28970 ) ;
#1750 = FACE_OUTER_BOUND ( 'NONE', #45333, .T. ) ;
#1751 = CARTESIAN_POINT ( 'NONE',  ( 1.198249040959072476, 0.5229268992822183604, 1.909581253797772327 ) ) ;
#1752 = AXIS2_PLACEMENT_3D ( 'NONE', #8218, #27822, #27568 ) ;
#1753 = CARTESIAN_POINT ( 'NONE',  ( -1.195183497228115035E-16, 0.000000000000000000, -0.3149606299212591165 ) ) ;
#1754 = ADVANCED_FACE ( 'NONE', ( #24603 ), #12464, .F. ) ;
#1755 = CARTESIAN_POINT ( 'NONE',  ( 2.755905511811024056, 0.000000000000000000, 0.000000000000000000 ) ) ;
#1756 = VECTOR ( 'NONE', #17200, 39.37007874015748143 ) ;
#1757 = VECTOR ( 'NONE', #29478, 39.37007874015748143 ) ;
#1758 = CARTESIAN_POINT ( 'NONE',  ( 0.000000000000000000, 3.267716535433071279, 1.259842519685033357 ) ) ;
#1759 = VERTEX_POINT ( 'NONE', #20719 ) ;
#1760 = DIRECTION ( 'NONE',  ( -1.000000000000000000, -0.000000000000000000, -0.000000000000000000 ) ) ;
#1761 = EDGE_CURVE ( 'NONE', #2996, #43121, #35297, .T. ) ;
#1762 = DIRECTION ( 'NONE',  ( -0.000000000000000000, -1.000000000000000000, -0.000000000000000000 ) ) ;
#1763 = AXIS2_PLACEMENT_3D ( 'NONE', #9871, #37757, #5743 ) ;
#1764 = ORIENTED_EDGE ( 'NONE', *, *, #34871, .F. ) ;
#1765 = CARTESIAN_POINT ( 'NONE',  ( -0.07591351300297316529, 3.267716535433071279, 2.633779063002562669E-17 ) ) ;
#1766 = EDGE_CURVE ( 'NONE', #38164, #33053, #17116, .T. ) ;
#1767 = VECTOR ( 'NONE', #4520, 39.37007874015748143 ) ;
#1768 = VERTEX_POINT ( 'NONE', #32878 ) ;
#1769 = CARTESIAN_POINT ( 'NONE',  ( 0.1250607540065018508, 1.205361022782829114E-17, -1.938545675207280272 ) ) ;
#1770 = EDGE_CURVE ( 'NONE', #2803, #35147, #32616, .T. ) ;
#1771 = DIRECTION ( 'NONE',  ( -0.000000000000000000, 1.000000000000000000, -0.000000000000000000 ) ) ;
#1772 = VECTOR ( 'NONE', #28811, 39.37007874015748143 ) ;
#1773 = CARTESIAN_POINT ( 'NONE',  ( -1.091055626815042645, 0.000000000000000000, -0.6299212598425177889 ) ) ;
#1774 = CARTESIAN_POINT ( 'NONE',  ( -1.068075307999488244, 6.692913385826772199, 1.883606783264637041 ) ) ;
#1775 = CARTESIAN_POINT ( 'NONE',  ( -3.051175669084205122, 5.118110236220475784, 0.7468891277766208647 ) ) ;
#1776 = EDGE_LOOP ( 'NONE', ( #15327, #17178, #12022, #18609 ) ) ;
#1777 = DIRECTION ( 'NONE',  ( -0.9998717552508122886, -0.01601477604151182316, 0.000000000000000000 ) ) ;
#1778 = CARTESIAN_POINT ( 'NONE',  ( 1.560669927219591413, 3.346456692913386100, 1.732283464566921172 ) ) ;
#1779 = CARTESIAN_POINT ( 'NONE',  ( 1.172646544058803419, 1.004405902117069482, -2.321602171295483519 ) ) ;
#1780 = ORIENTED_EDGE ( 'NONE', *, *, #4806, .F. ) ;
#1781 = FACE_OUTER_BOUND ( 'NONE', #1081, .T. ) ;
#1782 = ORIENTED_EDGE ( 'NONE', *, *, #34505, .T. ) ;
#1783 = EDGE_CURVE ( 'NONE', #40457, #35065, #13244, .T. ) ;
#1784 = CARTESIAN_POINT ( 'NONE',  ( -2.735162923786631950, 5.118110236220475784, -0.4201650439732181885 ) ) ;
#1785 = DIRECTION ( 'NONE',  ( 1.734723475976806848E-16, -0.000000000000000000, 1.000000000000000000 ) ) ;
#1786 = LINE ( 'NONE', #22181, #28170 ) ;
#1787 = ADVANCED_FACE ( 'NONE', ( #27955 ), #39833, .F. ) ;
#1788 = LINE ( 'NONE', #21928, #21403 ) ;
#1789 = EDGE_CURVE ( 'NONE', #26586, #34031, #38975, .T. ) ;
#1790 = ORIENTED_EDGE ( 'NONE', *, *, #32995, .F. ) ;
#1791 = ORIENTED_EDGE ( 'NONE', *, *, #3018, .T. ) ;
#1792 = CARTESIAN_POINT ( 'NONE',  ( 4.097771990496412577E-16, 3.346456692913386100, 2.106299212598425008 ) ) ;
#1793 = CARTESIAN_POINT ( 'NONE',  ( -1.408960544533061299, 0.005352583808700523381, 1.060663264281380025 ) ) ;
#1794 = FACE_BOUND ( 'NONE', #50025, .T. ) ;
#1795 = ORIENTED_EDGE ( 'NONE', *, *, #21839, .F. ) ;
#1796 = AXIS2_PLACEMENT_3D ( 'NONE', #21511, #1892, #40382 ) ;
#1797 = AXIS2_PLACEMENT_3D ( 'NONE', #40161, #32682, #13051 ) ;
#1798 = LINE ( 'NONE', #21425, #50069 ) ;
#1799 = PLANE ( 'NONE',  #32439 ) ;
#1800 = ORIENTED_EDGE ( 'NONE', *, *, #34831, .T. ) ;
#1801 = VERTEX_POINT ( 'NONE', #16251 ) ;
#1802 = CARTESIAN_POINT ( 'NONE',  ( -1.166969139818015977, 3.267716535433071279, 1.732283464566920950 ) ) ;
#1803 = VECTOR ( 'NONE', #44755, 39.37007874015748143 ) ;
#1804 = CARTESIAN_POINT ( 'NONE',  ( -2.168245791271168343, 1.560742704294596495, -2.004968704497279486 ) ) ;
#1805 = VERTEX_POINT ( 'NONE', #15232 ) ;
#1806 = ORIENTED_EDGE ( 'NONE', *, *, #35108, .T. ) ;
#1807 = AXIS2_PLACEMENT_3D ( 'NONE', #36604, #16468, #32221 ) ;
#1808 = ORIENTED_EDGE ( 'NONE', *, *, #48554, .F. ) ;
#1809 = DIRECTION ( 'NONE',  ( 1.734723475976806848E-16, 0.000000000000000000, 1.000000000000000000 ) ) ;
#1810 = VECTOR ( 'NONE', #40053, 39.37007874015748143 ) ;
#1811 = CARTESIAN_POINT ( 'NONE',  ( 0.8584932060599987924, 0.6447981115998615564, -0.5410498576272521065 ) ) ;
#1812 = FACE_OUTER_BOUND ( 'NONE', #1326, .T. ) ;
#1813 = ADVANCED_FACE ( 'NONE', ( #31749 ), #10608, .T. ) ;
#1814 = DIRECTION ( 'NONE',  ( -0.01601477604151182663, 0.9998717552508123996, -0.000000000000000000 ) ) ;
#1815 = ORIENTED_EDGE ( 'NONE', *, *, #33358, .T. ) ;
#1816 = VERTEX_POINT ( 'NONE', #43344 ) ;
#1817 = FACE_OUTER_BOUND ( 'NONE', #50210, .T. ) ;
#1818 = PLANE ( 'NONE',  #7661 ) ;
#1819 = LINE ( 'NONE', #40304, #19353 ) ;
#1820 = EDGE_CURVE ( 'NONE', #13717, #20069, #3359, .T. ) ;
#1821 = CARTESIAN_POINT ( 'NONE',  ( 1.015142113812069091, 3.253856391387305536, -2.229897935479296045 ) ) ;
#1822 = EDGE_CURVE ( 'NONE', #24587, #45327, #31242, .T. ) ;
#1823 = CARTESIAN_POINT ( 'NONE',  ( -1.599172890215280196, 1.205361022782829114E-17, 1.460879300779170498 ) ) ;
#1824 = EDGE_CURVE ( 'NONE', #35318, #22173, #36431, .T. ) ;
#1825 = CARTESIAN_POINT ( 'NONE',  ( -2.061297163897529483, 3.267716535433071279, 0.4330708661417290162 ) ) ;
#1826 = ADVANCED_FACE ( 'NONE', ( #7990 ), #27856, .F. ) ;
#1827 = ORIENTED_EDGE ( 'NONE', *, *, #3133, .T. ) ;
#1828 = CARTESIAN_POINT ( 'NONE',  ( -0.6214413264104939882, 3.267716535433071279, 1.535433070866133898 ) ) ;
#1829 = LINE ( 'NONE', #40563, #10390 ) ;
#1830 = B_SPLINE_CURVE_WITH_KNOTS ( 'NONE', 3,
 ( #8012, #19368, #3634, #11133 ),
 .UNSPECIFIED., .F., .F.,
 ( 4, 4 ),
 ( 2.136331082783953371E-07, 0.01878046567066712566 ),
 .UNSPECIFIED. ) ;
#1831 = VERTEX_POINT ( 'NONE', #46693 ) ;
#1832 = EDGE_LOOP ( 'NONE', ( #27560, #25233, #45645, #15043 ) ) ;
#1833 = CARTESIAN_POINT ( 'NONE',  ( 1.942732458483374502, 0.000000000000000000, 2.223636218514625451 ) ) ;
#1834 = AXIS2_PLACEMENT_3D ( 'NONE', #15753, #31513, #47209 ) ;
#1835 = CARTESIAN_POINT ( 'NONE',  ( 2.391446464649568338, 1.749586706978336847, 0.8287732470519283412 ) ) ;
#1836 = ORIENTED_EDGE ( 'NONE', *, *, #33749, .F. ) ;
#1837 = VECTOR ( 'NONE', #23812, 39.37007874015748143 ) ;
#1838 = ORIENTED_EDGE ( 'NONE', *, *, #44996, .T. ) ;
#1839 = LINE ( 'NONE', #17592, #699 ) ;
#1840 = VECTOR ( 'NONE', #44776, 39.37007874015748143 ) ;
#1841 = EDGE_CURVE ( 'NONE', #33606, #24319, #3868, .T. ) ;
#1842 = EDGE_LOOP ( 'NONE', ( #30346, #11606, #34513, #5960 ) ) ;
#1843 = AXIS2_PLACEMENT_3D ( 'NONE', #16566, #20425, #811 ) ;
#1844 = CARTESIAN_POINT ( 'NONE',  ( -1.195183497228115035E-16, 3.346456692913386100, -0.6299212598425177889 ) ) ;
#1845 = ADVANCED_FACE ( 'NONE', ( #11360 ), #35367, .T. ) ;
#1846 = CARTESIAN_POINT ( 'NONE',  ( 2.106197740627111958, 3.346456692913386100, 0.9055118110236164419 ) ) ;
#1847 = EDGE_CURVE ( 'NONE', #17810, #1039, #27094, .T. ) ;
#1848 = ORIENTED_EDGE ( 'NONE', *, *, #23704, .F. ) ;
#1849 = VERTEX_POINT ( 'NONE', #8250 ) ;
#1850 = CARTESIAN_POINT ( 'NONE',  ( -1.091055626815042645, 0.000000000000000000, -7.512581982576723358E-16 ) ) ;
#1852 = ORIENTED_EDGE ( 'NONE', *, *, #39006, .T. ) ;
#1851 = EDGE_CURVE ( 'NONE', #33493, #44848, #29673, .T. ) ;
#1853 = EDGE_LOOP ( 'NONE', ( #21363, #32081, #38553, #8334 ) ) ;
#1854 = CARTESIAN_POINT ( 'NONE',  ( -2.576863348864732117, 1.679095609600309347, 1.442554885838411849 ) ) ;
#1855 = CARTESIAN_POINT ( 'NONE',  ( -0.8182917201112814842, 3.346456692913386100, 0.2755905511810998187 ) ) ;
#1856 = FACE_OUTER_BOUND ( 'NONE', #10037, .T. ) ;
#1857 = ORIENTED_EDGE ( 'NONE', *, *, #46260, .T. ) ;
#1858 = DIRECTION ( 'NONE',  ( -0.000000000000000000, 1.000000000000000000, -0.000000000000000000 ) ) ;
#1859 = LINE ( 'NONE', #45203, #33289 ) ;
#1860 = DIRECTION ( 'NONE',  ( -3.469446951953613696E-16, 0.000000000000000000, -1.000000000000000000 ) ) ;
#1861 = ORIENTED_EDGE ( 'NONE', *, *, #31742, .T. ) ;
#1862 = CARTESIAN_POINT ( 'NONE',  ( -0.7855418668307149188, 0.000000000000000000, -2.846347029613745416 ) ) ;
#1863 = LINE ( 'NONE', #30253, #34328 ) ;
#1864 = LINE ( 'NONE', #10380, #46254 ) ;
#1865 = VERTEX_POINT ( 'NONE', #39744 ) ;
#1866 = ORIENTED_EDGE ( 'NONE', *, *, #6780, .F. ) ;
#1868 = AXIS2_PLACEMENT_3D ( 'NONE', #9555, #48999, #26061 ) ;
#1867 = CARTESIAN_POINT ( 'NONE',  ( 0.4788131938641111973, 1.628272305554966159, 2.914091152102192162 ) ) ;
#1869 = CARTESIAN_POINT ( 'NONE',  ( 2.947574761915768171, 5.118110236220475784, -0.1816379373804906938 ) ) ;
#1870 = CARTESIAN_POINT ( 'NONE',  ( -2.455254038405515260, 1.680983089212531700, -1.640354883748661008 ) ) ;
#1871 = EDGE_LOOP ( 'NONE', ( #19907, #19633, #9084, #50749 ) ) ;
#1872 = VERTEX_POINT ( 'NONE', #31489 ) ;
#1873 = VECTOR ( 'NONE', #38631, 39.37007874015748143 ) ;
#1874 = CARTESIAN_POINT ( 'NONE',  ( -1.979793062125317471, 1.589971192595758698, 2.191257344206539948 ) ) ;
#1875 = CIRCLE ( 'NONE', #24952, 0.3740157480314960647 ) ;
#1876 = ORIENTED_EDGE ( 'NONE', *, *, #27813, .F. ) ;
#1877 = FACE_OUTER_BOUND ( 'NONE', #19574, .T. ) ;
#1878 = DIRECTION ( 'NONE',  ( -2.582876339026174526E-17, -1.000000000000000000, -1.131632063491654496E-16 ) ) ;
#1879 = VECTOR ( 'NONE', #23022, 39.37007874015748143 ) ;
#1880 = VECTOR ( 'NONE', #44413, 39.37007874015748143 ) ;
#1881 = EDGE_CURVE ( 'NONE', #44810, #17605, #4374, .T. ) ;
#1882 = CARTESIAN_POINT ( 'NONE',  ( -1.574237088929739459, 0.000000000000000000, 0.7912475138866331692 ) ) ;
#1883 = EDGE_CURVE ( 'NONE', #18808, #35441, #39487, .T. ) ;
#1885 = FACE_OUTER_BOUND ( 'NONE', #35656, .T. ) ;
#1884 = APPLICATION_CONTEXT ( 'automotive_design' ) ;
#1886 = CARTESIAN_POINT ( 'NONE',  ( -1.472219874544909768, 1.546549606962118517, 2.560030851058948898 ) ) ;
#1887 = VECTOR ( 'NONE', #39407, 39.37007874015748143 ) ;
#1888 = ORIENTED_EDGE ( 'NONE', *, *, #17950, .T. ) ;
#1889 = ADVANCED_FACE ( 'NONE', ( #43854 ), #23476, .F. ) ;
#1890 = DIRECTION ( 'NONE',  ( 0.9195277725514489076, -4.565640798866420661E-17, 0.3930250316539278810 ) ) ;
#1891 = LINE ( 'NONE', #48139, #6225 ) ;
#1892 = DIRECTION ( 'NONE',  ( -0.000000000000000000, -1.000000000000000000, -0.000000000000000000 ) ) ;
#1893 = EDGE_CURVE ( 'NONE', #49676, #22883, #39228, .T. ) ;
#1894 = ORIENTED_EDGE ( 'NONE', *, *, #43085, .F. ) ;
#1895 = DIRECTION ( 'NONE',  ( -1.000000000000000000, -0.000000000000000000, -0.000000000000000000 ) ) ;
#1896 = PLANE ( 'NONE',  #49188 ) ;
#1897 = CARTESIAN_POINT ( 'NONE',  ( 1.942732458483374502, 0.000000000000000000, 2.223636218514625451 ) ) ;
#1898 = ORIENTED_EDGE ( 'NONE', *, *, #19244, .F. ) ;
#1899 = CARTESIAN_POINT ( 'NONE',  ( -0.3486774197067339376, 3.267716535433071279, 2.137096964226333107 ) ) ;
#1900 = CARTESIAN_POINT ( 'NONE',  ( 2.455248528070247627, 1.458620360574546471, -1.640363231549772260 ) ) ;
#1901 = ORIENTED_EDGE ( 'NONE', *, *, #11412, .F. ) ;
#1902 = CARTESIAN_POINT ( 'NONE',  ( 0.7423782071083084855, 3.267716535433071279, -2.575641807848709208E-16 ) ) ;
#1903 = LINE ( 'NONE', #33920, #25761 ) ;
#1905 = VERTEX_POINT ( 'NONE', #237 ) ;
#1904 = EDGE_CURVE ( 'NONE', #39081, #5779, #4125, .T. ) ;
#1906 = CARTESIAN_POINT ( 'NONE',  ( 1.363819533518803695, 3.346456692913386100, 1.605145679676862835 ) ) ;
#1907 = DIRECTION ( 'NONE',  ( -0.000000000000000000, 1.000000000000000000, -0.000000000000000000 ) ) ;
#1908 = EDGE_CURVE ( 'NONE', #7137, #24825, #37006, .T. ) ;
#1909 = FACE_BOUND ( 'NONE', #41553, .T. ) ;
#1910 = CARTESIAN_POINT ( 'NONE',  ( 0.5455278134075211005, 0.000000000000000000, -0.5118110236220467790 ) ) ;
#1911 = DIRECTION ( 'NONE',  ( 1.086719731106943413E-16, -1.000000000000000000, 4.078527368698718974E-17 ) ) ;
#1912 = VECTOR ( 'NONE', #43681, 39.37007874015748143 ) ;
#1913 = ORIENTED_EDGE ( 'NONE', *, *, #39250, .F. ) ;
#1914 = EDGE_LOOP ( 'NONE', ( #37060, #41743, #23416, #50019 ) ) ;
#1915 = CARTESIAN_POINT ( 'NONE',  ( -0.2493966119946618154, 1.605482210820551758, -2.222016418551142181 ) ) ;
#1916 = LINE ( 'NONE', #48352, #8127 ) ;
#1917 = EDGE_CURVE ( 'NONE', #29859, #43448, #14303, .T. ) ;
#1918 = ORIENTED_EDGE ( 'NONE', *, *, #33050, .T. ) ;
#1919 = PLANE ( 'NONE',  #14377 ) ;
#1920 = LINE ( 'NONE', #25923, #20294 ) ;
#1921 = CARTESIAN_POINT ( 'NONE',  ( -0.5110594979943671179, 0.000000000000000000, -1.666798357583582524 ) ) ;
#1922 = EDGE_CURVE ( 'NONE', #50744, #13274, #1527, .T. ) ;
#1923 = CIRCLE ( 'NONE', #33258, 2.165354330708661568 ) ;
#1924 = AXIS2_PLACEMENT_3D ( 'NONE', #31727, #42823, #23455 ) ;
#1925 = ORIENTED_EDGE ( 'NONE', *, *, #24754, .T. ) ;
#1926 = ORIENTED_EDGE ( 'NONE', *, *, #43337, .T. ) ;
#1927 = CARTESIAN_POINT ( 'NONE',  ( -0.2727639067037602172, 3.346456692913386100, 1.102362204724404160 ) ) ;
#1928 = CARTESIAN_POINT ( 'NONE',  ( -0.8182917201112819283, 0.000000000000000000, 1.850393700787391849 ) ) ;
#1929 = FACE_OUTER_BOUND ( 'NONE', #20700, .T. ) ;
#1930 = EDGE_LOOP ( 'NONE', ( #23938, #32963, #17065, #45642 ) ) ;
#1931 = CARTESIAN_POINT ( 'NONE',  ( 1.287906020515830141, 3.346456692913386100, 1.259842519685033357 ) ) ;
#1932 = FACE_BOUND ( 'NONE', #27495, .T. ) ;
#1933 = VECTOR ( 'NONE', #48071, 39.37007874015748143 ) ;
#1934 = ORIENTED_EDGE ( 'NONE', *, *, #7135, .F. ) ;
#1935 = CARTESIAN_POINT ( 'NONE',  ( -0.07591351300297333182, 3.346456692913386100, -1.732283464566922726 ) ) ;
#1936 = ORIENTED_EDGE ( 'NONE', *, *, #4912, .F. ) ;
#1937 = ORIENTED_EDGE ( 'NONE', *, *, #20104, .F. ) ;
#1938 = DIRECTION ( 'NONE',  ( -0.9998717552508122886, -0.01601477604151181275, 0.000000000000000000 ) ) ;
#1939 = CARTESIAN_POINT ( 'NONE',  ( 0.000000000000000000, 3.346456692913386100, 0.000000000000000000 ) ) ;
#1940 = ORIENTED_EDGE ( 'NONE', *, *, #43000, .T. ) ;
#1941 = DIRECTION ( 'NONE',  ( 0.000000000000000000, -1.000000000000000000, 0.000000000000000000 ) ) ;
#1942 = PRODUCT_DEFINITION_CONTEXT ( 'detailed design', #14403, 'design' ) ;
#1943 = DIRECTION ( 'NONE',  ( 1.000000000000000000, 0.000000000000000000, 0.000000000000000000 ) ) ;
#1944 = ORIENTED_EDGE ( 'NONE', *, *, #20132, .F. ) ;
#1945 = CARTESIAN_POINT ( 'NONE',  ( 1.091055626815042645, 3.346456692913386100, -8.878505979408855953E-16 ) ) ;
#1946 = CARTESIAN_POINT ( 'NONE',  ( 2.947574761915768171, 1.205361022782829114E-17, -0.1816379373804913322 ) ) ;
#1947 = CARTESIAN_POINT ( 'NONE',  ( -0.2727639067037607723, 0.000000000000000000, 0.1574803149606283648 ) ) ;
#1948 = VECTOR ( 'NONE', #40537, 39.37007874015748854 ) ;
#1949 = ADVANCED_FACE ( 'NONE', ( #36649 ), #48980, .F. ) ;
#1950 = FACE_OUTER_BOUND ( 'NONE', #43350, .T. ) ;
#1951 = FACE_OUTER_BOUND ( 'NONE', #36387, .T. ) ;
#1952 = ORIENTED_EDGE ( 'NONE', *, *, #9468, .T. ) ;
#1953 = EDGE_CURVE ( 'NONE', #30043, #20275, #13025, .T. ) ;
#1954 = FACE_OUTER_BOUND ( 'NONE', #16449, .T. ) ;
#1955 = VECTOR ( 'NONE', #41461, 39.37007874015748143 ) ;
#1956 = PLANE ( 'NONE',  #42142 ) ;
#1957 = ADVANCED_FACE ( 'NONE', ( #5398 ), #24769, .T. ) ;
#1958 = VECTOR ( 'NONE', #12006, 39.37007874015748143 ) ;
#1959 = VECTOR ( 'NONE', #13764, 39.37007874015748854 ) ;
#1960 = VERTEX_POINT ( 'NONE', #21154 ) ;
#1961 = DIRECTION ( 'NONE',  ( 1.000000000000000000, -0.000000000000000000, 0.000000000000000000 ) ) ;
#1962 = FACE_OUTER_BOUND ( 'NONE', #20652, .T. ) ;
#1963 = ORIENTED_EDGE ( 'NONE', *, *, #46858, .F. ) ;
#1964 = CARTESIAN_POINT ( 'NONE',  ( 1.157218145390799036, 0.000000000000000000, 0.2363238328731523952 ) ) ;
#1965 = EDGE_CURVE ( 'NONE', #17854, #37445, #44376, .T. ) ;
#1966 = DIRECTION ( 'NONE',  ( 0.000000000000000000, 0.000000000000000000, 1.000000000000000000 ) ) ;
#1967 = CARTESIAN_POINT ( 'NONE',  ( -1.716666360678977599, 3.346456692913386100, 1.220472440944875281 ) ) ;
#1968 = CONICAL_SURFACE ( 'NONE', #45601, 2.246510896728926010, 0.01601546068027819014 ) ;
#1969 = ORIENTED_EDGE ( 'NONE', *, *, #17010, .T. ) ;
#1970 = CARTESIAN_POINT ( 'NONE',  ( -0.2727639067037602172, 0.000000000000000000, 2.047244094488179567 ) ) ;
#1971 = ORIENTED_EDGE ( 'NONE', *, *, #42708, .F. ) ;
#1972 = FACE_BOUND ( 'NONE', #28570, .T. ) ;
#1973 = LINE ( 'NONE', #21851, #42402 ) ;
#1974 = LINE ( 'NONE', #21346, #14410 ) ;
#1975 = EDGE_CURVE ( 'NONE', #29456, #40420, #33290, .T. ) ;
#1976 = DIRECTION ( 'NONE',  ( -0.000000000000000000, 1.000000000000000000, -0.000000000000000000 ) ) ;
#1977 = VERTEX_POINT ( 'NONE', #28373 ) ;
#1978 = ORIENTED_EDGE ( 'NONE', *, *, #45941, .T. ) ;
#1979 = DIRECTION ( 'NONE',  ( 1.734723475976806848E-16, -0.000000000000000000, 1.000000000000000000 ) ) ;
#1980 = VERTEX_POINT ( 'NONE', #8506 ) ;
#1981 = ADVANCED_FACE ( 'NONE', ( #48469, #16771, #40265, #33041, #47959, #32529, #44877, #48723, #40520, #9529, #13402, #5659, #36390, #4889, #1011, #44620, #20889, #5141, #25018, #24258, #25277, #12896, #40003, #9273, #4634, #41034, #20633, #20377, #36133, #763, #16514, #12633, #44116, #12831, #9464, #29073, #1206, #44558, #13597, #44310, #32979, #44813, #25211, #40969, #28823, #25460, #8951, #29333, #5077, #1457, #32723, #5332, #5589, #49171, #1972, #48654, #17214, #13090, #48400, #9207, #21341, #24709, #48154, #9722, #37351, #24955, #37094, #45066, #17461, #16708, #20826, #40707, #41222, #36326, #1713, #32462, #13339, #33227, #28564, #48910, #5842, #40460, #21592, #17720, #33485, #36583, #13849, #29596, #45315, #21085, #9972, #16965, #40200, #36841, #4829, #20574, #948, #26470, #34737, #38611, #41723, #30101, #49922, #41975, #3233, #29846, #45817, #42217, #34487, #6858, #41468, #46322, #22860, #18226, #14609, #50173, #2989, #2231, #6360, #10483, #10984, #34237, #33985, #18981, #45562, #6095, #18483, #21850, #2731, #25972, #18737, #26724, #14865, #22106, #30356, #46076, #30608, #37864, #10735, #2489, #50419, #26226, #22608, #42472 ), #38361, .F. ) ;
#1982 = LINE ( 'NONE', #6368, #2995 ) ;
#1983 = ORIENTED_EDGE ( 'NONE', *, *, #34002, .F. ) ;
#1984 = DIRECTION ( 'NONE',  ( 0.9998717552508121775, 0.01601477604151182663, 0.000000000000000000 ) ) ;
#1985 = EDGE_LOOP ( 'NONE', ( #10367, #36295, #11306, #46455 ) ) ;
#1986 = FACE_OUTER_BOUND ( 'NONE', #7666, .T. ) ;
#1987 = VECTOR ( 'NONE', #19193, 39.37007874015748143 ) ;
#1988 = DIRECTION ( 'NONE',  ( 0.01601477604151182663, -0.9998717552508123996, 0.000000000000000000 ) ) ;
#1989 = VECTOR ( 'NONE', #20549, 39.37007874015748143 ) ;
#1990 = ORIENTED_EDGE ( 'NONE', *, *, #18984, .T. ) ;
#1991 = LINE ( 'NONE', #14373, #45448 ) ;
#1992 = VECTOR ( 'NONE', #27537, 39.37007874015748143 ) ;
#1993 = ORIENTED_EDGE ( 'NONE', *, *, #2686, .F. ) ;
#1994 = VERTEX_POINT ( 'NONE', #15109 ) ;
#1995 = EDGE_CURVE ( 'NONE', #26915, #4915, #10227, .T. ) ;
#1996 = VECTOR ( 'NONE', #25407, 39.37007874015748854 ) ;
#1997 = AXIS2_PLACEMENT_3D ( 'NONE', #5441, #804, #16558 ) ;
#1998 = ORIENTED_EDGE ( 'NONE', *, *, #46406, .T. ) ;
#1999 = ORIENTED_EDGE ( 'NONE', *, *, #46946, .T. ) ;
#2000 = DIRECTION ( 'NONE',  ( 1.000000000000000000, 0.000000000000000000, 0.000000000000000000 ) ) ;
#2001 = VECTOR ( 'NONE', #23786, 39.37007874015748143 ) ;
#2002 = EDGE_LOOP ( 'NONE', ( #43852, #43434, #22980, #21233 ) ) ;
#2003 = DIRECTION ( 'NONE',  ( 1.000000000000000000, -0.000000000000000000, 0.000000000000000000 ) ) ;
#2004 = PLANE ( 'NONE',  #47446 ) ;
#2005 = DIRECTION ( 'NONE',  ( -0.000000000000000000, 0.000000000000000000, 1.000000000000000000 ) ) ;
#2006 = VERTEX_POINT ( 'NONE', #46570 ) ;
#2007 = FACE_OUTER_BOUND ( 'NONE', #28920, .T. ) ;
#2008 = DIRECTION ( 'NONE',  ( -0.01601477604151182663, 0.9998717552508123996, -0.000000000000000000 ) ) ;
#2009 = VERTEX_POINT ( 'NONE', #25715 ) ;
#2010 = EDGE_CURVE ( 'NONE', #48838, #20798, #19752, .T. ) ;
#2011 = DIRECTION ( 'NONE',  ( 0.000000000000000000, -1.000000000000000000, 0.000000000000000000 ) ) ;
#2012 = DIRECTION ( 'NONE',  ( 0.000000000000000000, 1.000000000000000000, 0.000000000000000000 ) ) ;
#2013 = LINE ( 'NONE', #47941, #38398 ) ;
#2014 = PLANE ( 'NONE',  #9984 ) ;
#2015 = EDGE_CURVE ( 'NONE', #19298, #47601, #17971, .T. ) ;
#2016 = CARTESIAN_POINT ( 'NONE',  ( -0.8942052331142552601, 0.000000000000000000, -1.771653543307081025 ) ) ;
#2017 = EDGE_CURVE ( 'NONE', #41776, #22927, #14099, .T. ) ;
#2018 = CARTESIAN_POINT ( 'NONE',  ( -2.182111253630085290, 0.000000000000000000, 0.4330708661417290162 ) ) ;
#2019 = EDGE_LOOP ( 'NONE', ( #1254, #36247, #6486, #7808 ) ) ;
#2020 = DIRECTION ( 'NONE',  ( -1.000000000000000000, 0.000000000000000000, 0.000000000000000000 ) ) ;
#2021 = EDGE_CURVE ( 'NONE', #22341, #945, #27831, .T. ) ;
#2022 = CARTESIAN_POINT ( 'NONE',  ( 1.834323595590318323, 0.000000000000000000, 1.151859023884926891 ) ) ;
#2023 = CARTESIAN_POINT ( 'NONE',  ( -0.8942052331142552601, 0.000000000000000000, -0.6299212598425177889 ) ) ;
#2024 = ORIENTED_EDGE ( 'NONE', *, *, #22534, .T. ) ;
#2025 = DIRECTION ( 'NONE',  ( -3.469446951953613696E-16, 0.000000000000000000, -1.000000000000000000 ) ) ;
#2026 = VECTOR ( 'NONE', #27967, 39.37007874015748143 ) ;
#2027 = VECTOR ( 'NONE', #20312, 39.37007874015748143 ) ;
#2028 = ORIENTED_EDGE ( 'NONE', *, *, #33301, .F. ) ;
#2029 = DIRECTION ( 'NONE',  ( -6.394449067488625930E-17, -1.000000000000000000, 9.687176266499597757E-17 ) ) ;
#2030 = VECTOR ( 'NONE', #47127, 39.37007874015748143 ) ;
#2032 = CIRCLE ( 'NONE', #23460, 2.443628662382284489 ) ;
#2031 = PLANE ( 'NONE',  #23384 ) ;
#2033 = DIRECTION ( 'NONE',  ( -0.000000000000000000, 1.000000000000000000, -0.000000000000000000 ) ) ;
#2034 = CARTESIAN_POINT ( 'NONE',  ( 0.8182917201112817063, 0.000000000000000000, -1.417322834645664331 ) ) ;
#2035 = ADVANCED_FACE ( 'NONE', ( #38859 ), #24124, .T. ) ;
#2036 = LINE ( 'NONE', #14923, #24443 ) ;
#2037 = ORIENTED_EDGE ( 'NONE', *, *, #20509, .T. ) ;
#2038 = LINE ( 'NONE', #6923, #3533 ) ;
#2039 = AXIS2_PLACEMENT_3D ( 'NONE', #7726, #15726, #39220 ) ;
#2040 = VERTEX_POINT ( 'NONE', #3999 ) ;
#2041 = PLANE ( 'NONE',  #15531 ) ;
#2042 = ORIENTED_EDGE ( 'NONE', *, *, #22947, .F. ) ;
#2043 = EDGE_CURVE ( 'NONE', #45470, #12597, #31618, .T. ) ;
#2044 = DIRECTION ( 'NONE',  ( -3.469446951953613696E-16, 0.000000000000000000, -1.000000000000000000 ) ) ;
#2045 = CARTESIAN_POINT ( 'NONE',  ( 0.5455278134075211005, 0.000000000000000000, 0.4330708661417287386 ) ) ;
#2046 = ORIENTED_EDGE ( 'NONE', *, *, #38984, .T. ) ;
#2047 = FACE_OUTER_BOUND ( 'NONE', #42994, .T. ) ;
#2048 = ADVANCED_FACE ( 'NONE', ( #11995 ), #8123, .F. ) ;
#2049 = LINE ( 'NONE', #6685, #4305 ) ;
#2050 = CARTESIAN_POINT ( 'NONE',  ( -1.738921996492520661, 6.764728787913346618E-05, 0.1249482579781430736 ) ) ;
#2051 = ORIENTED_EDGE ( 'NONE', *, *, #28454, .F. ) ;
#2052 = ORIENTED_EDGE ( 'NONE', *, *, #47966, .T. ) ;
#2053 = CARTESIAN_POINT ( 'NONE',  ( -0.6214413264104945434, 3.267716535433071279, -0.9842519685039342603 ) ) ;
#2054 = FACE_BOUND ( 'NONE', #15095, .T. ) ;
#2055 = ORIENTED_EDGE ( 'NONE', *, *, #37185, .F. ) ;
#2056 = EDGE_CURVE ( 'NONE', #6833, #47979, #42964, .T. ) ;
#2057 = DIRECTION ( 'NONE',  ( 1.734723475976806848E-16, -0.000000000000000000, 1.000000000000000000 ) ) ;
#2058 = CARTESIAN_POINT ( 'NONE',  ( 0.4536155964708684651, 0.5249316475426858419, -1.828623345083124629 ) ) ;
#2059 = ORIENTED_EDGE ( 'NONE', *, *, #19455, .T. ) ;
#2060 = EDGE_LOOP ( 'NONE', ( #50689, #8405, #10719, #45390 ) ) ;
#2061 = CARTESIAN_POINT ( 'NONE',  ( 0.002207914879453961969, 6.692913385826772199, 0.04916304461325451958 ) ) ;
#2062 = CIRCLE ( 'NONE', #40827, 2.106299212598425008 ) ;
#2063 = CARTESIAN_POINT ( 'NONE',  ( -2.339241080213612989, 5.905511811023623991, 1.802537235681883843 ) ) ;
#2064 = EDGE_CURVE ( 'NONE', #18162, #11395, #40734, .T. ) ;
#2065 = EDGE_LOOP ( 'NONE', ( #23297, #143 ) ) ;
#2066 = VECTOR ( 'NONE', #16030, 39.37007874015748143 ) ;
#2067 = ORIENTED_EDGE ( 'NONE', *, *, #16930, .F. ) ;
#2068 = VECTOR ( 'NONE', #9146, 39.37007874015748143 ) ;
#2070 = EDGE_CURVE ( 'NONE', #2321, #4093, #16123, .T. ) ;
#2069 = VERTEX_POINT ( 'NONE', #31116 ) ;
#2071 = CARTESIAN_POINT ( 'NONE',  ( 0.8067290215917983787, 1.574803149606302854, 2.009464521518182334 ) ) ;
#2072 = CARTESIAN_POINT ( 'NONE',  ( 0.000000000000000000, 3.267716535433071279, -0.6299212598425181220 ) ) ;
#2073 = CARTESIAN_POINT ( 'NONE',  ( -0.8942052331142552601, 3.267716535433071279, -1.907064071829739582 ) ) ;
#2074 = DIRECTION ( 'NONE',  ( -3.469446951953613696E-16, 0.000000000000000000, -1.000000000000000000 ) ) ;
#2075 = VERTEX_POINT ( 'NONE', #31888 ) ;
#2076 = ORIENTED_EDGE ( 'NONE', *, *, #96, .T. ) ;
#2077 = CIRCLE ( 'NONE', #32561, 2.106299212598425008 ) ;
#2078 = DIRECTION ( 'NONE',  ( 0.000000000000000000, -1.000000000000000000, 0.000000000000000000 ) ) ;
#2079 = CARTESIAN_POINT ( 'NONE',  ( 1.645338673473796254, 0.05427277550655955352, -1.027111169014480296 ) ) ;
#2080 = DIRECTION ( 'NONE',  ( -0.9510565162951544194, 0.000000000000000000, 0.3090169943749447312 ) ) ;
#2081 = CARTESIAN_POINT ( 'NONE',  ( -2.454875160333845674, 3.346456692913386100, -0.03937007874015881204 ) ) ;
#2082 = DIRECTION ( 'NONE',  ( 0.000000000000000000, 1.000000000000000000, 0.000000000000000000 ) ) ;
#2083 = ADVANCED_FACE ( 'NONE', ( #35241 ), #47062, .F. ) ;
#2084 = CARTESIAN_POINT ( 'NONE',  ( -0.5455278134075214336, 3.267716535433071279, -0.6299212598425175669 ) ) ;
#2085 = ADVANCED_FACE ( 'NONE', ( #27989 ), #43726, .F. ) ;
#2086 = CARTESIAN_POINT ( 'NONE',  ( -1.985260859929297572, 3.267716535433071279, 6.887757239314511260E-16 ) ) ;
#2087 = VERTEX_POINT ( 'NONE', #39872 ) ;
#2088 = DIRECTION ( 'NONE',  ( -0.000000000000000000, 1.000000000000000000, -0.000000000000000000 ) ) ;
#2089 = DIRECTION ( 'NONE',  ( -1.000000000000000000, -0.000000000000000000, -0.000000000000000000 ) ) ;
#2090 = ORIENTED_EDGE ( 'NONE', *, *, #40283, .F. ) ;
#2091 = VERTEX_POINT ( 'NONE', #39110 ) ;
#2092 = CARTESIAN_POINT ( 'NONE',  ( 0.9832762519060537221, 3.254021347498972094, -2.244094488188969283 ) ) ;
#2093 = ORIENTED_EDGE ( 'NONE', *, *, #50503, .F. ) ;
#2094 = AXIS2_PLACEMENT_3D ( 'NONE', #24493, #48198, #44596 ) ;
#2095 = VECTOR ( 'NONE', #27789, 39.37007874015748143 ) ;
#2096 = ORIENTED_EDGE ( 'NONE', *, *, #48432, .T. ) ;
#2097 = DIRECTION ( 'NONE',  ( -0.000000000000000000, 1.000000000000000000, -0.000000000000000000 ) ) ;
#2098 = VECTOR ( 'NONE', #21981, 39.37007874015748143 ) ;
#2099 = EDGE_LOOP ( 'NONE', ( #46700, #22556, #4842, #3168 ) ) ;
#2100 = DIRECTION ( 'NONE',  ( -1.156061316345072978E-16, -1.000000000000000000, -1.040474016969658122E-17 ) ) ;
#2101 = DIRECTION ( 'NONE',  ( 1.734723475976806848E-16, -0.000000000000000000, 1.000000000000000000 ) ) ;
#2102 = EDGE_CURVE ( 'NONE', #34448, #47888, #11736, .T. ) ;
#2103 = VERTEX_POINT ( 'NONE', #50667 ) ;
#2104 = VERTEX_POINT ( 'NONE', #16386 ) ;
#2105 = CIRCLE ( 'NONE', #43287, 1.743387098533651480 ) ;
#2106 = FACE_OUTER_BOUND ( 'NONE', #7010, .T. ) ;
#2107 = ORIENTED_EDGE ( 'NONE', *, *, #38743, .T. ) ;
#2108 = VERTEX_POINT ( 'NONE', #32139 ) ;
#2109 = LINE ( 'NONE', #37233, #30621 ) ;
#2110 = CARTESIAN_POINT ( 'NONE',  ( 0.1968503937007869686, 3.346456692913386100, -2.401574803149598480 ) ) ;
#2111 = DIRECTION ( 'NONE',  ( 0.000000000000000000, 1.160734090543304660E-16, -1.000000000000000000 ) ) ;
#2112 = EDGE_CURVE ( 'NONE', #49063, #44346, #7867, .T. ) ;
#2113 = VERTEX_POINT ( 'NONE', #42722 ) ;
#2114 = EDGE_CURVE ( 'NONE', #1008, #4354, #7367, .T. ) ;
#2115 = CARTESIAN_POINT ( 'NONE',  ( 0.1155636338427008941, -0.5222242541845523167, 0.000000000000000000 ) ) ;
#2116 = DIRECTION ( 'NONE',  ( 0.000000000000000000, 0.000000000000000000, 1.000000000000000000 ) ) ;
#2117 = DIRECTION ( 'NONE',  ( -0.000000000000000000, 1.000000000000000000, -0.000000000000000000 ) ) ;
#2118 = ADVANCED_FACE ( 'NONE', ( #19227 ), #15366, .F. ) ;
#2119 = ORIENTED_EDGE ( 'NONE', *, *, #28284, .F. ) ;
#2120 = CARTESIAN_POINT ( 'NONE',  ( -0.4349608091551079303, 6.692913385826772199, 2.121218629000294342 ) ) ;
#2121 = CARTESIAN_POINT ( 'NONE',  ( -0.2727639067037608278, 0.000000000000000000, -1.299212598425193210 ) ) ;
#2122 = DIRECTION ( 'NONE',  ( -3.469446951953613696E-16, 0.000000000000000000, -1.000000000000000000 ) ) ;
#2123 = VERTEX_POINT ( 'NONE', #15615 ) ;
#2124 = ORIENTED_EDGE ( 'NONE', *, *, #24368, .T. ) ;
#2125 = LINE ( 'NONE', #6761, #1099 ) ;
#2126 = DIRECTION ( 'NONE',  ( 0.000000000000000000, 0.000000000000000000, -1.000000000000000000 ) ) ;
#2127 = ADVANCED_FACE ( 'NONE', ( #27476 ), #43221, .F. ) ;
#2128 = DIRECTION ( 'NONE',  ( 0.000000000000000000, 0.000000000000000000, 1.000000000000000000 ) ) ;
#2129 = VERTEX_POINT ( 'NONE', #13279 ) ;
#2130 = ORIENTED_EDGE ( 'NONE', *, *, #10354, .T. ) ;
#2131 = VECTOR ( 'NONE', #554, 39.37007874015748143 ) ;
#2132 = VECTOR ( 'NONE', #33580, 39.37007874015748143 ) ;
#2133 = DIRECTION ( 'NONE',  ( 1.734723475976806848E-16, -0.000000000000000000, 1.000000000000000000 ) ) ;
#2134 = ORIENTED_EDGE ( 'NONE', *, *, #15843, .T. ) ;
#2135 = DIRECTION ( 'NONE',  ( 1.734723475976806848E-16, 0.000000000000000000, 1.000000000000000000 ) ) ;
#2136 = CARTESIAN_POINT ( 'NONE',  ( -3.927031490892378253E-16, 3.267716535433071279, -1.889763779527552146 ) ) ;
#2137 = CIRCLE ( 'NONE', #43349, 2.106299212598425008 ) ;
#2138 = ADVANCED_FACE ( 'NONE', ( #24642 ), #1396, .F. ) ;
#2139 = AXIS2_PLACEMENT_3D ( 'NONE', #14242, #29488, #9616 ) ;
#2140 = EDGE_CURVE ( 'NONE', #8542, #8317, #4782, .T. ) ;
#2141 = EDGE_CURVE ( 'NONE', #1994, #23693, #20758, .T. ) ;
#2142 = CARTESIAN_POINT ( 'NONE',  ( -0.2906532981117672110, 1.205361022782829114E-17, 1.877244666688175245 ) ) ;
#2143 = CARTESIAN_POINT ( 'NONE',  ( 2.168245791271197209, 1.753049777144058297, -2.004968704497248844 ) ) ;
#2144 = CARTESIAN_POINT ( 'NONE',  ( -0.3486774197067334380, 3.346456692913386100, 1.574803149606291974 ) ) ;
#2145 = VECTOR ( 'NONE', #4186, 39.37007874015748143 ) ;
#2146 = EDGE_LOOP ( 'NONE', ( #1482, #16863, #46508, #15990 ) ) ;
#2147 = EDGE_CURVE ( 'NONE', #23949, #38782, #5267, .T. ) ;
#2148 = DIRECTION ( 'NONE',  ( 1.000000000000000000, 0.000000000000000000, 0.000000000000000000 ) ) ;
#2149 = LINE ( 'NONE', #49345, #43308 ) ;
#2150 = CARTESIAN_POINT ( 'NONE',  ( 0.8182917201112819283, 0.000000000000000000, -0.7874015748031473194 ) ) ;
#2151 = ORIENTED_EDGE ( 'NONE', *, *, #34267, .F. ) ;
#2152 = CARTESIAN_POINT ( 'NONE',  ( 1.363819533518803029, 3.267716535433071279, -2.365849761790804994E-16 ) ) ;
#2153 = CARTESIAN_POINT ( 'NONE',  ( 1.722303613724171623, 1.475870595485188730, -2.398480198668616392 ) ) ;
#2154 = DIRECTION ( 'NONE',  ( -1.000000000000000000, 0.000000000000000000, -0.000000000000000000 ) ) ;
#2155 = ORIENTED_EDGE ( 'NONE', *, *, #10077, .F. ) ;
#2156 = PLANE ( 'NONE',  #41575 ) ;
#2157 = ORIENTED_EDGE ( 'NONE', *, *, #20849, .F. ) ;
#2158 = LINE ( 'NONE', #33671, #47708 ) ;
#2159 = CARTESIAN_POINT ( 'NONE',  ( 0.04921259842519669359, 1.574803149606302854, 2.164795024401847456 ) ) ;
#2160 = VERTEX_POINT ( 'NONE', #48595 ) ;
#2161 = B_SPLINE_CURVE_WITH_KNOTS ( 'NONE', 3,
 ( #2715, #6846, #46062, #38846 ),
 .UNSPECIFIED., .F., .F.,
 ( 4, 4 ),
 ( 0.1211873102087489551, 0.1625992483279400380 ),
 .UNSPECIFIED. ) ;
#2162 = CARTESIAN_POINT ( 'NONE',  ( 3.937007874015748143, 2.913385826771657250, 1.023622047244094446 ) ) ;
#2163 = FACE_OUTER_BOUND ( 'NONE', #23547, .T. ) ;
#2164 = CARTESIAN_POINT ( 'NONE',  ( -0.04921259842519689481, 0.000000000000000000, -2.165433070866142007 ) ) ;
#2165 = PLANE ( 'NONE',  #45793 ) ;
#2166 = VECTOR ( 'NONE', #4421, 39.37007874015748143 ) ;
#2167 = CARTESIAN_POINT ( 'NONE',  ( 1.387241876633648729, 1.574803149606302854, 1.662624236931697475 ) ) ;
#2168 = VERTEX_POINT ( 'NONE', #25397 ) ;
#2169 = ORIENTED_EDGE ( 'NONE', *, *, #14575, .T. ) ;
#2170 = LINE ( 'NONE', #21031, #50351 ) ;
#2171 = VECTOR ( 'NONE', #2851, 39.37007874015748143 ) ;
#2172 = DIRECTION ( 'NONE',  ( 1.734723475976806848E-16, -0.000000000000000000, 1.000000000000000000 ) ) ;
#2173 = AXIS2_PLACEMENT_3D ( 'NONE', #33770, #22138, #10006 ) ;
#2174 = VERTEX_POINT ( 'NONE', #16899 ) ;
#2175 = DIRECTION ( 'NONE',  ( -0.000000000000000000, 0.000000000000000000, 1.000000000000000000 ) ) ;
#2176 = CARTESIAN_POINT ( 'NONE',  ( -1.681836974315507049, 0.5249316497054297148, 0.8491494812773747736 ) ) ;
#2177 = LINE ( 'NONE', #38064, #35200 ) ;
#2178 = VECTOR ( 'NONE', #49310, 39.37007874015748143 ) ;
#2179 = VERTEX_POINT ( 'NONE', #43985 ) ;
#2180 = VERTEX_POINT ( 'NONE', #24894 ) ;
#2181 = ADVANCED_FACE ( 'NONE', ( #44747 ), #9399, .F. ) ;
#2182 = CARTESIAN_POINT ( 'NONE',  ( 2.152441353505198940, 1.205361022782829114E-17, -0.2419059403264799679 ) ) ;
#2183 = CARTESIAN_POINT ( 'NONE',  ( -2.133310810460457674, 0.5250879747123590180, 0.2393145321957796390 ) ) ;
#2184 = VECTOR ( 'NONE', #49480, 39.37007874015748143 ) ;
#2185 = LINE ( 'NONE', #28781, #28022 ) ;
#2186 = EDGE_CURVE ( 'NONE', #24144, #19688, #25374, .T. ) ;
#2187 = ORIENTED_EDGE ( 'NONE', *, *, #30207, .T. ) ;
#2188 = CARTESIAN_POINT ( 'NONE',  ( -1.166969139818016199, 3.346456692913386100, -1.823990790610291013 ) ) ;
#2189 = EDGE_CURVE ( 'NONE', #45998, #35616, #44249, .T. ) ;
#2191 = AXIS2_PLACEMENT_3D ( 'NONE', #7129, #50430, #12266 ) ;
#2190 = CARTESIAN_POINT ( 'NONE',  ( 1.560669927219590525, 3.267716535433071279, -0.3543307086614178592 ) ) ;
#2192 = ORIENTED_EDGE ( 'NONE', *, *, #3229, .F. ) ;
#2193 = CARTESIAN_POINT ( 'NONE',  ( 0.4788131938641111973, 1.628272305554966159, 2.914091152102192162 ) ) ;
#2194 = ORIENTED_EDGE ( 'NONE', *, *, #14285, .F. ) ;
#2195 = EDGE_LOOP ( 'NONE', ( #50078, #19189, #11181, #21896 ) ) ;
#2196 = DIRECTION ( 'NONE',  ( -0.000000000000000000, 1.000000000000000000, -0.000000000000000000 ) ) ;
#2197 = PLANE ( 'NONE',  #19286 ) ;
#2198 = EDGE_CURVE ( 'NONE', #31414, #50326, #5527, .T. ) ;
#2199 = ORIENTED_EDGE ( 'NONE', *, *, #48460, .F. ) ;
#2200 = LINE ( 'NONE', #28794, #28556 ) ;
#2201 = CARTESIAN_POINT ( 'NONE',  ( 0.1067246931122726866, 0.02962905676920215767, 0.000000000000000000 ) ) ;
#2202 = EDGE_LOOP ( 'NONE', ( #41177, #39326, #6550, #5166 ) ) ;
#2203 = ADVANCED_FACE ( 'NONE', ( #21527 ), #1135, .F. ) ;
#2204 = CARTESIAN_POINT ( 'NONE',  ( 0.7423782071083087075, 0.000000000000000000, -0.9448818897637765168 ) ) ;
#2205 = DIRECTION ( 'NONE',  ( 1.734723475976806848E-16, -0.000000000000000000, 1.000000000000000000 ) ) ;
#2206 = EDGE_CURVE ( 'NONE', #18373, #5670, #28756, .T. ) ;
#2207 = VECTOR ( 'NONE', #37854, 39.37007874015748143 ) ;
#2208 = LINE ( 'NONE', #9188, #46178 ) ;
#2209 = ADVANCED_FACE ( 'NONE', ( #9145 ), #40400, .F. ) ;
#2210 = CARTESIAN_POINT ( 'NONE',  ( 1.363819533518803251, 3.346456692913386100, 1.220472440944875281 ) ) ;
#2211 = DIRECTION ( 'NONE',  ( 1.000000000000000000, 0.000000000000000000, 0.000000000000000000 ) ) ;
#2212 = VECTOR ( 'NONE', #9248, 39.37007874015748143 ) ;
#2213 = ORIENTED_EDGE ( 'NONE', *, *, #3477, .F. ) ;
#2214 = LINE ( 'NONE', #21579, #43914 ) ;
#2215 = CIRCLE ( 'NONE', #49953, 1.682967650661292502 ) ;
#2216 = EDGE_CURVE ( 'NONE', #7713, #35081, #29268, .T. ) ;
#2217 = EDGE_CURVE ( 'NONE', #47517, #11723, #17658, .T. ) ;
#2218 = DIRECTION ( 'NONE',  ( -1.000000000000000000, 0.000000000000000000, 1.734723475976806848E-16 ) ) ;
#2219 = VERTEX_POINT ( 'NONE', #28240 ) ;
#2220 = FACE_OUTER_BOUND ( 'NONE', #828, .T. ) ;
#2221 = PLANE ( 'NONE',  #45081 ) ;
#2222 = ORIENTED_EDGE ( 'NONE', *, *, #33322, .F. ) ;
#2223 = CARTESIAN_POINT ( 'NONE',  ( 0.000000000000000000, 3.267716535433071279, -2.244094488188968395 ) ) ;
#2224 = AXIS2_PLACEMENT_3D ( 'NONE', #2386, #14251, #45723 ) ;
#2225 = PLANE ( 'NONE',  #33295 ) ;
#2226 = CARTESIAN_POINT ( 'NONE',  ( 2.110884035022549732, 1.741711621820001943, -0.9557545615714394538 ) ) ;
#2227 = AXIS2_PLACEMENT_3D ( 'NONE', #7320, #34937, #31831 ) ;
#2228 = ORIENTED_EDGE ( 'NONE', *, *, #27851, .F. ) ;
#2229 = PLANE ( 'NONE',  #38701 ) ;
#2230 = ORIENTED_EDGE ( 'NONE', *, *, #16362, .F. ) ;
#2231 = FACE_BOUND ( 'NONE', #3970, .T. ) ;
#2232 = CARTESIAN_POINT ( 'NONE',  ( 1.181102362204724310, 0.5905511811023621549, -1.062992125984252079 ) ) ;
#2233 = LINE ( 'NONE', #36843, #43244 ) ;
#2234 = DIRECTION ( 'NONE',  ( -1.000000000000000000, 0.000000000000000000, 0.000000000000000000 ) ) ;
#2235 = ORIENTED_EDGE ( 'NONE', *, *, #298, .F. ) ;
#2236 = ORIENTED_EDGE ( 'NONE', *, *, #36947, .T. ) ;
#2237 = DIRECTION ( 'NONE',  ( -0.000000000000000000, 1.000000000000000000, -0.000000000000000000 ) ) ;
#2238 = CARTESIAN_POINT ( 'NONE',  ( 1.015142113812069313, 3.346456692913386100, 0.7874015748031454320 ) ) ;
#2239 = ORIENTED_EDGE ( 'NONE', *, *, #17711, .T. ) ;
#2240 = DIRECTION ( 'NONE',  ( -0.000000000000000000, 1.000000000000000000, -0.000000000000000000 ) ) ;
#2241 = VERTEX_POINT ( 'NONE', #48343 ) ;
#2242 = CARTESIAN_POINT ( 'NONE',  ( 2.106197740627112402, 3.346456692913386100, 0.1574803149606280872 ) ) ;
#2243 = VECTOR ( 'NONE', #13775, 39.37007874015748143 ) ;
#2244 = DIRECTION ( 'NONE',  ( 3.986037398843765983E-20, 1.000000000000000000, 1.160734090543304660E-16 ) ) ;
#2245 = EDGE_CURVE ( 'NONE', #2075, #30992, #24382, .T. ) ;
#2246 = VECTOR ( 'NONE', #25440, 39.37007874015748143 ) ;
#2247 = ORIENTED_EDGE ( 'NONE', *, *, #8547, .F. ) ;
#2248 = ADVANCED_FACE ( 'NONE', ( #36265 ), #16645, .F. ) ;
#2249 = CARTESIAN_POINT ( 'NONE',  ( 1.328631193326356597, 1.732744587876588138, 2.127804219470494473 ) ) ;
#2250 = ORIENTED_EDGE ( 'NONE', *, *, #34945, .T. ) ;
#2251 = ORIENTED_EDGE ( 'NONE', *, *, #16576, .T. ) ;
#2252 = EDGE_CURVE ( 'NONE', #2180, #26524, #49360, .T. ) ;
#2253 = ORIENTED_EDGE ( 'NONE', *, *, #41769, .T. ) ;
#2254 = EDGE_LOOP ( 'NONE', ( #38376, #36963, #7977, #38935 ) ) ;
#2255 = CARTESIAN_POINT ( 'NONE',  ( 1.636583440222563857, 0.000000000000000000, 1.062992125984245639 ) ) ;
#2256 = ORIENTED_EDGE ( 'NONE', *, *, #8108, .F. ) ;
#2258 = DIRECTION ( 'NONE',  ( -1.000000000000000000, 0.000000000000000000, 1.734723475976806848E-16 ) ) ;
#2257 = VECTOR ( 'NONE', #1245, 39.37007874015748143 ) ;
#2259 = CARTESIAN_POINT ( 'NONE',  ( 0.7423782071083091516, 3.346456692913386100, 1.377952755905504256 ) ) ;
#2260 = ADVANCED_FACE ( 'NONE', ( #6029 ), #44342, .T. ) ;
#2261 = PLANE ( 'NONE',  #12368 ) ;
#2262 = CARTESIAN_POINT ( 'NONE',  ( 1.636583440222563857, 0.000000000000000000, -0.3149606299212596716 ) ) ;
#2263 = DIRECTION ( 'NONE',  ( 1.734723475976806848E-16, -0.000000000000000000, 1.000000000000000000 ) ) ;
#2264 = VERTEX_POINT ( 'NONE', #49102 ) ;
#2265 = EDGE_CURVE ( 'NONE', #2113, #38863, #22110, .T. ) ;
#2266 = LINE ( 'NONE', #49713, #24996 ) ;
#2267 = DIRECTION ( 'NONE',  ( 0.000000000000000000, 0.000000000000000000, 1.000000000000000000 ) ) ;
#2268 = EDGE_CURVE ( 'NONE', #45405, #32424, #49608, .T. ) ;
#2269 = DIRECTION ( 'NONE',  ( 1.734723475976806848E-16, -0.000000000000000000, 1.000000000000000000 ) ) ;
#2270 = DIRECTION ( 'NONE',  ( 0.000000000000000000, -1.000000000000000000, 0.000000000000000000 ) ) ;
#2271 = ORIENTED_EDGE ( 'NONE', *, *, #2436, .T. ) ;
#2272 = FACE_OUTER_BOUND ( 'NONE', #23827, .T. ) ;
#2273 = LINE ( 'NONE', #18023, #37672 ) ;
#2274 = VERTEX_POINT ( 'NONE', #2162 ) ;
#2275 = CARTESIAN_POINT ( 'NONE',  ( 0.5455278134075211005, 3.267716535433071279, 0.4330708661417287386 ) ) ;
#2276 = VECTOR ( 'NONE', #13484, 39.37007874015748143 ) ;
#2277 = VECTOR ( 'NONE', #43910, 39.37007874015748143 ) ;
#2278 = DIRECTION ( 'NONE',  ( 0.000000000000000000, 0.000000000000000000, 1.000000000000000000 ) ) ;
#2279 = ORIENTED_EDGE ( 'NONE', *, *, #32230, .F. ) ;
#2280 = CARTESIAN_POINT ( 'NONE',  ( 0.1067246931122726866, 0.02962905676920215767, 0.000000000000000000 ) ) ;
#2281 = B_SPLINE_CURVE_WITH_KNOTS ( 'NONE', 3,
 ( #8835, #24840, #8067, #40343 ),
 .UNSPECIFIED., .F., .F.,
 ( 4, 4 ),
 ( 0.1211775127643062722, 0.1625894504277921315 ),
 .UNSPECIFIED. ) ;
#2282 = ORIENTED_EDGE ( 'NONE', *, *, #11605, .F. ) ;
#2283 = DIRECTION ( 'NONE',  ( -3.469446951953613696E-16, 0.000000000000000000, -1.000000000000000000 ) ) ;
#2284 = FACE_OUTER_BOUND ( 'NONE', #35475, .T. ) ;
#2285 = CARTESIAN_POINT ( 'NONE',  ( -2.182111253630085290, 3.346456692913386100, 0.1181102362204704270 ) ) ;
#2286 = CARTESIAN_POINT ( 'NONE',  ( -1.363819533518803473, 0.000000000000000000, -0.4724409448818886470 ) ) ;
#2287 = CARTESIAN_POINT ( 'NONE',  ( 0.1968503937007873017, 0.000000000000000000, -1.574803149606293529 ) ) ;
#2288 = ORIENTED_EDGE ( 'NONE', *, *, #9406, .F. ) ;
#2289 = CARTESIAN_POINT ( 'NONE',  ( 1.015142113812069313, 3.267716535433071279, -3.521981712565032882E-16 ) ) ;
#2290 = B_SPLINE_CURVE_WITH_KNOTS ( 'NONE', 3,
 ( #44947, #40073, #9601, #4708 ),
 .UNSPECIFIED., .F., .F.,
 ( 4, 4 ),
 ( 0.001338086368243570886, 0.004829149077268580018 ),
 .UNSPECIFIED. ) ;
#2291 = ORIENTED_EDGE ( 'NONE', *, *, #25331, .T. ) ;
#2292 = EDGE_LOOP ( 'NONE', ( #24210, #36504, #29232, #35366 ) ) ;
#2293 = DIRECTION ( 'NONE',  ( 0.000000000000000000, 0.000000000000000000, -1.000000000000000000 ) ) ;
#2294 = ORIENTED_EDGE ( 'NONE', *, *, #36093, .T. ) ;
#2295 = CARTESIAN_POINT ( 'NONE',  ( 0.000000000000000000, 3.267716535433071279, 2.047244094488179567 ) ) ;
#2296 = VECTOR ( 'NONE', #8934, 39.37007874015748143 ) ;
#2297 = LINE ( 'NONE', #6681, #12873 ) ;
#2298 = VERTEX_POINT ( 'NONE', #10158 ) ;
#2299 = LINE ( 'NONE', #18301, #1700 ) ;
#2300 = DIRECTION ( 'NONE',  ( 0.000000000000000000, -1.000000000000000000, 0.000000000000000000 ) ) ;
#2301 = CARTESIAN_POINT ( 'NONE',  ( -1.599172890215279974, 5.905511811023623991, 1.460879300779171164 ) ) ;
#2302 = VERTEX_POINT ( 'NONE', #21786 ) ;
#2304 = VERTEX_POINT ( 'NONE', #37797 ) ;
#2303 = EDGE_CURVE ( 'NONE', #20098, #21303, #12173, .T. ) ;
#2305 = FACE_OUTER_BOUND ( 'NONE', #48145, .T. ) ;
#2306 = FACE_BOUND ( 'NONE', #42970, .T. ) ;
#2307 = VERTEX_POINT ( 'NONE', #37545 ) ;
#2308 = ADVANCED_FACE ( 'NONE', ( #25652 ), #2422, .F. ) ;
#2309 = LINE ( 'NONE', #36922, #13859 ) ;
#2310 = CARTESIAN_POINT ( 'NONE',  ( 1.560669927219590525, 3.267716535433071279, -5.414661521997676285E-16 ) ) ;
#2311 = AXIS2_PLACEMENT_3D ( 'NONE', #14353, #37606, #38112 ) ;
#2312 = AXIS2_PLACEMENT_3D ( 'NONE', #38674, #46631, #14668 ) ;
#2314 = ORIENTED_EDGE ( 'NONE', *, *, #12927, .T. ) ;
#2313 = EDGE_CURVE ( 'NONE', #7509, #35465, #18672, .T. ) ;
#2315 = EDGE_LOOP ( 'NONE', ( #20777, #23819, #16602, #48748 ) ) ;
#2316 = FACE_OUTER_BOUND ( 'NONE', #33186, .T. ) ;
#2317 = FACE_OUTER_BOUND ( 'NONE', #32941, .T. ) ;
#2318 = VERTEX_POINT ( 'NONE', #33675 ) ;
#2319 = ORIENTED_EDGE ( 'NONE', *, *, #49256, .T. ) ;
#2320 = AXIS2_PLACEMENT_3D ( 'NONE', #31509, #42112, #35130 ) ;
#2321 = VERTEX_POINT ( 'NONE', #45499 ) ;
#2322 = FACE_OUTER_BOUND ( 'NONE', #40191, .T. ) ;
#2323 = B_SPLINE_CURVE_WITH_KNOTS ( 'NONE', 3,
 ( #41483, #6628, #44825, #6111 ),
 .UNSPECIFIED., .F., .F.,
 ( 4, 4 ),
 ( 2.018269109134904797E-07, 0.002500207302720079423 ),
 .UNSPECIFIED. ) ;
#2324 = CARTESIAN_POINT ( 'NONE',  ( 1.015142113812069313, 3.267716535433071279, -0.4724409448818889246 ) ) ;
#2325 = VECTOR ( 'NONE', #18352, 39.37007874015748143 ) ;
#2326 = EDGE_CURVE ( 'NONE', #24313, #42844, #6294, .T. ) ;
#2327 = CARTESIAN_POINT ( 'NONE',  ( -1.091055626815042201, 0.000000000000000000, 1.377952755905504256 ) ) ;
#2328 = CARTESIAN_POINT ( 'NONE',  ( 0.000000000000000000, 3.346456692913386100, 0.000000000000000000 ) ) ;
#2329 = VECTOR ( 'NONE', #27569, 39.37007874015748143 ) ;
#2330 = ORIENTED_EDGE ( 'NONE', *, *, #10631, .F. ) ;
#2331 = ORIENTED_EDGE ( 'NONE', *, *, #15545, .F. ) ;
#2332 = LINE ( 'NONE', #21444, #31544 ) ;
#2333 = DIRECTION ( 'NONE',  ( 1.000000000000000000, 0.000000000000000000, -3.469446951953613696E-16 ) ) ;
#2334 = DIRECTION ( 'NONE',  ( -0.000000000000000000, 1.000000000000000000, -0.000000000000000000 ) ) ;
#2335 = EDGE_CURVE ( 'NONE', #36771, #7345, #22042, .T. ) ;
#2336 = VECTOR ( 'NONE', #44604, 39.37007874015748143 ) ;
#2337 = CARTESIAN_POINT ( 'NONE',  ( -0.5284761224300573712, 6.692913385826772199, -2.099874368989736784 ) ) ;
#2338 = DIRECTION ( 'NONE',  ( -0.01601477604151182663, 0.9998717552508123996, -0.000000000000000000 ) ) ;
#2339 = FACE_OUTER_BOUND ( 'NONE', #23939, .T. ) ;
#2340 = EDGE_CURVE ( 'NONE', #47312, #25798, #28682, .T. ) ;
#2341 = B_SPLINE_CURVE_WITH_KNOTS ( 'NONE', 3,
 ( #3364, #49796, #14483, #14740 ),
 .UNSPECIFIED., .F., .F.,
 ( 4, 4 ),
 ( 0.001822469492255983543, 0.004322476834427013172 ),
 .UNSPECIFIED. ) ;
#2342 = DIRECTION ( 'NONE',  ( -0.000000000000000000, 1.000000000000000000, -0.000000000000000000 ) ) ;
#2343 = ORIENTED_EDGE ( 'NONE', *, *, #47528, .T. ) ;
#2344 = FACE_OUTER_BOUND ( 'NONE', #43355, .T. ) ;
#2345 = CARTESIAN_POINT ( 'NONE',  ( -1.546800823997126262, 1.683127104815683728, -1.546979550173933182 ) ) ;
#2346 = VERTEX_POINT ( 'NONE', #30035 ) ;
#2347 = EDGE_CURVE ( 'NONE', #44092, #23693, #38049, .T. ) ;
#2348 = ORIENTED_EDGE ( 'NONE', *, *, #46632, .F. ) ;
#2349 = DIRECTION ( 'NONE',  ( -0.000000000000000000, 1.000000000000000000, -0.000000000000000000 ) ) ;
#2350 = VECTOR ( 'NONE', #50356, 39.37007874015748143 ) ;
#2351 = ORIENTED_EDGE ( 'NONE', *, *, #26375, .T. ) ;
#2352 = EDGE_LOOP ( 'NONE', ( #16503, #7392, #21030, #7725 ) ) ;
#2353 = DIRECTION ( 'NONE',  ( -0.000000000000000000, 1.000000000000000000, -0.000000000000000000 ) ) ;
#2354 = CIRCLE ( 'NONE', #33704, 2.246510896728926010 ) ;
#2355 = ORIENTED_EDGE ( 'NONE', *, *, #3937, .T. ) ;
#2356 = CLOSED_SHELL ( 'NONE', ( #48906, #33438, #3352, #23489, #38798, #12613, #1981, #26148, #45748, #32793, #12742, #47076, #17850, #46605, #13479, #44502, #33285, #18234, #19127, #22021, #1480, #20482, #22830, #45082, #41414, #8100, #5929, #9918, #825, #50557, #44636, #30340, #28705, #12764, #21875, #47533, #45573, #25579, #15596, #31809, #34099, #38632, #6964, #18519, #44071, #39087, #23040, #33571, #18845, #18917, #37640, #46903, #9983, #33504, #2127, #15569, #2083, #33592, #39274, #5546, #34130, #19212, #31291, #38017, #4876, #25682, #43758, #16134, #16170, #9431, #28778, #43961, #2085, #26636, #18257, #6200, #34720, #775, #24407, #34198, #42232, #32434, #5569, #25162, #30401, #17856, #31203, #17915, #3481, #20071, #28587, #42465, #39654, #34993, #30420, #21098, #2698, #42048, #30562, #44384, #5391, #12837, #17054, #34703, #8375, #42617, #46749, #21853, #16069, #14643, #39384, #46636, #7569, #38342, #14997, #3409, #18562, #15145, #33341, #3105, #26843, #3967, #9846, #10082, #26131, #4000, #13671, #30915, #23445, #9440, #5133, #2048, #27527, #173, #40582, #2377, #11057, #17916, #3378, #14604, #3713, #3390, #4834, #18792, #30859, #39290, #22194, #33106, #42623, #20890, #48977, #36657, #48033, #47615, #33939, #31416, #25433, #38146, #2209, #20013, #10874, #50094, #8881, #31151, #48660, #37316, #9075, #46348, #26351, #40740, #17521, #24730, #31141, #17072, #29773, #3070, #48590, #48557, #9441, #50843, #42390, #45308, #38379, #2181, #2716, #35796, #39765, #25482, #17485, #10709, #50625, #9002, #13678, #43478, #43962, #9939, #3462, #23778, #14717, #753, #203, #34493, #45780, #30642, #471, #1204, #41578, #8077, #2248, #12560, #27165, #15081, #37079, #30569, #20091, #16434, #38690, #38963, #35766, #4814, #35861, #33467, #22466, #20315, #10653, #39987, #44440, #44090, #27902, #10876, #29798, #41071, #20491, #46484, #12153, #19611, #10108, #891, #14633, #34325, #234, #23534, #10336, #28573, #34842, #38184, #47721, #20702, #12672, #40361, #3541, #39784, #925, #35353, #40157, #50494, #8349, #3238, #11887, #25414, #29922, #16528, #13514, #20262, #36506, #30652, #33249, #32624, #20008, #13260, #13351, #33972, #38011, #10941, #1949, #1150, #49776, #33728, #10972, #45339, #7755, #34248, #3038, #31478, #29576, #37103, #32334, #1142, #11478, #9495, #32702, #50278, #19526, #28565, #44002, #3057, #49762, #974, #34038, #19250, #20207, #35173, #22127, #11032, #28335, #10969, #25900, #19948, #44725, #5781, #47819, #35017, #26992, #5351, #31619, #15619, #41880, #40798, #15405, #34217, #13994, #14252, #683, #14409, #13867, #35753, #28352, #33817, #43255, #4447, #42579, #50558, #38517, #26728, #20173, #49349, #11665, #16917, #3421, #35470, #22846, #13508, #27282, #48429, #25684, #36381, #11983, #2371, #34708, #21693, #10195, #43898, #47711, #27889, #47492, #35299, #25772, #5766, #20796, #3643, #29338, #42051, #21358, #8078, #36063, #7219, #46393, #11991, #43767, #9202, #5190, #25485, #49049, #18678, #29047, #23066, #31360, #42987, #45139, #41201, #47730, #26501, #4625, #42855, #12665, #49892, #20722, #39574, #10635, #23757, #36282, #21379, #8946, #27413, #39648, #15086, #29414, #562, #11389, #32263, #48150, #18746, #1537, #10314, #29919, #31231, #27620, #12380, #9570, #20374, #9530, #40960, #49584, #39855, #45547, #11913, #34733, #35497, #28576, #30934, #14959, #23447, #8303, #44927, #709, #24170, #24973, #7273, #14835, #1674, #4383, #15873, #44353, #20405, #18787, #30875, #16371, #27319, #8701, #39001, #18387, #7722, #28909, #16632, #42212, #26783, #14124, #39596, #50654, #39440, #21764, #40392, #7066, #14383, #41319, #50216, #36345, #30077, #19831, #27344, #1536, #24933, #11795, #2138, #13386, #15700, #4156, #26325, #8707, #21903, #40940, #21022, #48131, #29866, #39350, #38462, #19051, #13931, #40501, #11668, #42176, #8301, #11576, #27033, #36934, #22885, #43332, #7155, #12634, #11919, #20247, #4358, #39935, #12373, #6141, #31328, #37384, #28391, #18563, #21606, #36571, #9047, #35520, #31549, #22273, #33111, #31008, #26898, #50783, #36080, #253, #9987, #9625, #9490, #19303, #39501, #9363, #44267, #28272, #30453, #47971, #26725, #40834, #35153, #39636, #22061, #1476, #47912, #2661, #28017, #18640, #9827, #41292, #31802, #28074, #34009, #2450, #23220, #37377, #44215, #32329, #33950, #20855, #35781, #27354, #25999, #4441, #6336, #46847, #48944, #16718, #44547, #37215, #23646, #37989, #34959, #41110, #51029, #40577, #36991, #1384, #33847, #17052, #25144, #7742, #45418, #46514, #21946, #1889, #25779, #37584, #24232, #18713, #25902, #19044, #40674, #1020, #14121, #50836, #1787, #19818, #19958, #27400, #8756, #45078, #50790, #16273, #9019, #23540, #44258, #31781, #26982, #41673, #34609, #12055, #27925, #12115, #37946, #15474, #12478, #47665, #18259, #21003, #18932, #12923, #35876, #43084, #12030, #14615, #30010, #17007, #13509, #35001, #23256, #41003, #25267, #20687, #28925, #29403, #36713, #41868, #20833, #4323, #14503, #8668, #30626, #32080, #37631, #20644, #32516, #5805, #46734, #17527, #12435, #31770, #42526, #38364, #44298, #11038, #6641, #7024, #10689, #16493, #33701, #6636, #892, #46065, #37707, #2672, #5479, #5866, #38118, #31035, #22796, #10259, #19016, #1826, #38093, #8608, #30587, #31748, #44086, #26078, #24935, #10240, #48299, #91, #44846, #39543, #18142, #40676, #7142, #44886, #44143, #33607, #13389, #11463, #48811, #32523, #20986, #11965, #3683, #41132, #11402, #33025, #15343, #4746, #9333, #36837, #23836, #9367, #19871, #36898, #600, #34142, #34886, #29136, #27257, #21718, #15548, #37985, #29941, #25516, #35727, #50248, #34960, #50459, #15953, #38640, #26035, #19586, #22599, #45576, #48178, #29213, #10978, #43217, #10114, #16292, #47599, #43796, #30143, #35402, #49243, #34806, #3837, #45963, #33046, #18002, #38993, #25676, #18432, #15015, #31392, #29068, #36440, #25502, #19835, #15597, #25231, #39023, #25845, #17747, #38221, #24870, #18408, #27127, #35281, #44726, #37840, #21835, #42749, #14742, #6558, #29564, #10164, #15470, #8815, #38282, #30825, #49195, #33858, #48965, #3629, #45282, #18106, #49612, #41155, #30708, #22367, #861, #16598, #41346, #50197, #49107, #33398, #38100, #16725, #40128, #49053, #24789, #34208, #9990, #37508, #25841, #18690, #48257, #6734, #1401, #23008, #13383, #23734, #31512, #15810, #38090, #15828, #14510, #12713, #21762, #26347, #9610, #6686, #50521, #38965, #4325, #29303, #39065, #12485, #43147, #13550, #32026, #8470, #39849, #6023, #29003, #37289, #3234, #3189, #31516, #4992, #3817, #11333, #1754, #14605, #44722, #27270, #25616, #30973, #48053, #33472, #11878, #6552, #45181, #31352, #40362, #12940, #27780, #6386, #4874, #41446, #46166, #21683, #3331, #24623, #22290, #9658, #11343, #16991, #27681, #14320, #5905, #11169, #40837, #4742, #12134, #18922, #48671, #43786, #34889, #1744, #39183, #45367, #6049, #20282, #29496, #24718, #3525, #22917, #49766, #49652, #23911, #11630, #25438, #46627, #41136, #42565, #50339, #44867, #31197, #23468, #47620, #21151, #16820 ) ) ;
#2357 = VECTOR ( 'NONE', #18556, 39.37007874015748143 ) ;
#2358 = CARTESIAN_POINT ( 'NONE',  ( 0.000000000000000000, 3.267716535433071279, -2.047244094488181343 ) ) ;
#2359 = DIRECTION ( 'NONE',  ( -1.000000000000000000, 0.000000000000000000, 0.000000000000000000 ) ) ;
#2360 = B_SPLINE_CURVE_WITH_KNOTS ( 'NONE', 3,
 ( #26234, #50425, #15376, #39115 ),
 .UNSPECIFIED., .F., .F.,
 ( 4, 4 ),
 ( 0.001189830169353655025, 0.002095527556305008809 ),
 .UNSPECIFIED. ) ;
#2361 = AXIS2_PLACEMENT_3D ( 'NONE', #39911, #16682, #410 ) ;
#2362 = EDGE_LOOP ( 'NONE', ( #8292, #35201, #32595, #34940 ) ) ;
#2363 = EDGE_LOOP ( 'NONE', ( #41631, #27503, #21057, #35997 ) ) ;
#2364 = LINE ( 'NONE', #6238, #48551 ) ;
#2365 = ORIENTED_EDGE ( 'NONE', *, *, #43765, .T. ) ;
#2366 = ORIENTED_EDGE ( 'NONE', *, *, #9528, .F. ) ;
#2367 = CARTESIAN_POINT ( 'NONE',  ( -0.8182917201112819283, 3.267716535433071279, -0.7874015748031467643 ) ) ;
#2368 = CARTESIAN_POINT ( 'NONE',  ( 0.000000000000000000, 3.267716535433071279, 0.000000000000000000 ) ) ;
#2369 = DIRECTION ( 'NONE',  ( -0.3513748240813304724, 1.086859790425929286E-16, -0.9362348706397417564 ) ) ;
#2370 = VECTOR ( 'NONE', #14345, 39.37007874015748143 ) ;
#2371 = ADVANCED_FACE ( 'NONE', ( #10919 ), #10673, .F. ) ;
#2372 = ORIENTED_EDGE ( 'NONE', *, *, #8147, .F. ) ;
#2373 = VECTOR ( 'NONE', #34773, 39.37007874015748143 ) ;
#2374 = DIRECTION ( 'NONE',  ( 1.734723475976806848E-16, 0.000000000000000000, 1.000000000000000000 ) ) ;
#2375 = CARTESIAN_POINT ( 'NONE',  ( 1.225600105435542764, 0.000000000000000000, -1.239880218767107412 ) ) ;
#2376 = FACE_OUTER_BOUND ( 'NONE', #15482, .T. ) ;
#2377 = ADVANCED_FACE ( 'NONE', ( #22539 ), #7051, .F. ) ;
#2378 = ORIENTED_EDGE ( 'NONE', *, *, #31728, .F. ) ;
#2379 = CARTESIAN_POINT ( 'NONE',  ( 0.8949303405208899331, 5.905511811023623991, -1.971765468592530102 ) ) ;
#2380 = CARTESIAN_POINT ( 'NONE',  ( -1.636583440222564301, 3.346456692913386100, 1.574803149606291530 ) ) ;
#2381 = DIRECTION ( 'NONE',  ( -3.469446951953613696E-16, 0.000000000000000000, -1.000000000000000000 ) ) ;
#2382 = ORIENTED_EDGE ( 'NONE', *, *, #21414, .F. ) ;
#2383 = VERTEX_POINT ( 'NONE', #41911 ) ;
#2384 = DIRECTION ( 'NONE',  ( -3.469446951953613696E-16, 0.000000000000000000, -1.000000000000000000 ) ) ;
#2385 = VECTOR ( 'NONE', #37297, 39.37007874015748143 ) ;
#2386 = CARTESIAN_POINT ( 'NONE',  ( 0.000000000000000000, 2.755905511811022723, 0.000000000000000000 ) ) ;
#2387 = DIRECTION ( 'NONE',  ( 0.3930250316539278810, 1.067170571554331359E-16, -0.9195277725514489076 ) ) ;
#2388 = VERTEX_POINT ( 'NONE', #34424 ) ;
#2389 = ORIENTED_EDGE ( 'NONE', *, *, #49200, .F. ) ;
#2390 = DIRECTION ( 'NONE',  ( -0.000000000000000000, -1.000000000000000000, 0.000000000000000000 ) ) ;
#2391 = ORIENTED_EDGE ( 'NONE', *, *, #41956, .T. ) ;
#2392 = CARTESIAN_POINT ( 'NONE',  ( 1.560669927219590525, 0.000000000000000000, -0.03937007874015908959 ) ) ;
#2393 = CARTESIAN_POINT ( 'NONE',  ( -1.091055626815042201, 3.346456692913386100, 0.9448818897637749625 ) ) ;
#2394 = VECTOR ( 'NONE', #3697, 39.37007874015748143 ) ;
#2395 = VECTOR ( 'NONE', #37002, 39.37007874015748143 ) ;
#2396 = B_SPLINE_CURVE_WITH_KNOTS ( 'NONE', 3,
 ( #29789, #33680, #10162, #2167 ),
 .UNSPECIFIED., .F., .F.,
 ( 4, 4 ),
 ( 0.1211873102087489551, 0.1625992483279400103 ),
 .UNSPECIFIED. ) ;
#2397 = EDGE_CURVE ( 'NONE', #47516, #33248, #27081, .T. ) ;
#2398 = PRESENTATION_LAYER_ASSIGNMENT (  '', '', ( #7343 ) ) ;
#2399 = CARTESIAN_POINT ( 'NONE',  ( -1.511286805986099546, 0.000000000000000000, 0.8691436966266951059 ) ) ;
#2400 = DIRECTION ( 'NONE',  ( 1.241861098869888840E-16, 1.000000000000000000, -3.427318860986102267E-17 ) ) ;
#2401 = PLANE ( 'NONE',  #27041 ) ;
#2402 = ORIENTED_EDGE ( 'NONE', *, *, #11322, .T. ) ;
#2403 = CARTESIAN_POINT ( 'NONE',  ( 1.971834065208953435, 5.905511811023623991, 0.8963217522330176878 ) ) ;
#2404 = CARTESIAN_POINT ( 'NONE',  ( 0.5455278134075211005, 3.346456692913386100, 0.1181102362204701633 ) ) ;
#2405 = AXIS2_PLACEMENT_3D ( 'NONE', #1897, #9648, #21517 ) ;
#2406 = DIRECTION ( 'NONE',  ( 1.734723475976806848E-16, 0.000000000000000000, 1.000000000000000000 ) ) ;
#2407 = EDGE_CURVE ( 'NONE', #44829, #16948, #50113, .T. ) ;
#2408 = ORIENTED_EDGE ( 'NONE', *, *, #43800, .T. ) ;
#2409 = DIRECTION ( 'NONE',  ( -0.000000000000000000, 0.000000000000000000, 1.000000000000000000 ) ) ;
#2410 = B_SPLINE_CURVE_WITH_KNOTS ( 'NONE', 3,
 ( #14053, #26428, #22558, #14304 ),
 .UNSPECIFIED., .F., .F.,
 ( 4, 4 ),
 ( 0.0006976809599606449393, 0.004868339597052293195 ),
 .UNSPECIFIED. ) ;
#2411 = ADVANCED_FACE ( 'NONE', ( #43661 ), #5593, .T. ) ;
#2412 = LINE ( 'NONE', #5514, #37708 ) ;
#2413 = DIRECTION ( 'NONE',  ( -3.469446951953613696E-16, 0.000000000000000000, -1.000000000000000000 ) ) ;
#2415 = EDGE_CURVE ( 'NONE', #26163, #39867, #34918, .T. ) ;
#2414 = ORIENTED_EDGE ( 'NONE', *, *, #41235, .F. ) ;
#2416 = DIRECTION ( 'NONE',  ( -1.000000000000000000, 0.000000000000000000, 0.000000000000000000 ) ) ;
#2417 = EDGE_CURVE ( 'NONE', #31066, #3209, #15553, .T. ) ;
#2418 = EDGE_LOOP ( 'NONE', ( #45602, #5149, #345, #16611 ) ) ;
#2419 = DIRECTION ( 'NONE',  ( -2.214792131866782686E-16, 0.6427876096865404731, 0.7660444431189771253 ) ) ;
#2420 = LINE ( 'NONE', #13530, #47160 ) ;
#2421 = ORIENTED_EDGE ( 'NONE', *, *, #42689, .T. ) ;
#2422 = PLANE ( 'NONE',  #17128 ) ;
#2423 = EDGE_CURVE ( 'NONE', #14924, #14452, #50054, .T. ) ;
#2424 = CARTESIAN_POINT ( 'NONE',  ( 0.5550072188453405442, 1.618366210323673338, -2.196007637835879045 ) ) ;
#2425 = CARTESIAN_POINT ( 'NONE',  ( -2.182111253630085290, 3.346456692913386100, -6.146657985744592735E-16 ) ) ;
#2426 = CARTESIAN_POINT ( 'NONE',  ( 0.1067246931122726866, 0.02962905676920215767, 0.000000000000000000 ) ) ;
#2427 = VECTOR ( 'NONE', #24583, 39.37007874015748143 ) ;
#2428 = ORIENTED_EDGE ( 'NONE', *, *, #44263, .T. ) ;
#2429 = ORIENTED_EDGE ( 'NONE', *, *, #48141, .F. ) ;
#2430 = PLANE ( 'NONE',  #15788 ) ;
#2431 = DIRECTION ( 'NONE',  ( -1.000000000000000000, -0.000000000000000000, -0.000000000000000000 ) ) ;
#2432 = ORIENTED_EDGE ( 'NONE', *, *, #9263, .T. ) ;
#2433 = FACE_OUTER_BOUND ( 'NONE', #29874, .T. ) ;
#2434 = CARTESIAN_POINT ( 'NONE',  ( 0.000000000000000000, 3.267716535433071279, 1.259842519685033357 ) ) ;
#2435 = LINE ( 'NONE', #6308, #49167 ) ;
#2436 = EDGE_CURVE ( 'NONE', #4899, #1768, #42657, .T. ) ;
#2437 = AXIS2_PLACEMENT_3D ( 'NONE', #42873, #3648, #27633 ) ;
#2438 = ORIENTED_EDGE ( 'NONE', *, *, #12627, .F. ) ;
#2439 = ORIENTED_EDGE ( 'NONE', *, *, #47362, .T. ) ;
#2440 = CARTESIAN_POINT ( 'NONE',  ( 1.900276455977023549, 1.738338356005314722, -1.313328886422038710 ) ) ;
#2441 = PLANE ( 'NONE',  #10980 ) ;
#2442 = LINE ( 'NONE', #23069, #27797 ) ;
#2443 = B_SPLINE_CURVE_WITH_KNOTS ( 'NONE', 3,
 ( #32915, #44748, #17912, #2424 ),
 .UNSPECIFIED., .F., .F.,
 ( 4, 4 ),
 ( 2.075194745768200593E-07, 0.01748493206081992365 ),
 .UNSPECIFIED. ) ;
#2444 = ADVANCED_FACE ( 'NONE', ( #31302 ), #38583, .T. ) ;
#2445 = VERTEX_POINT ( 'NONE', #7303 ) ;
#2446 = AXIS2_PLACEMENT_3D ( 'NONE', #44744, #29779, #49357 ) ;
#2447 = DIRECTION ( 'NONE',  ( 0.000000000000000000, 0.000000000000000000, -1.000000000000000000 ) ) ;
#2448 = DIRECTION ( 'NONE',  ( 1.000000000000000000, -0.000000000000000000, 0.000000000000000000 ) ) ;
#2449 = ORIENTED_EDGE ( 'NONE', *, *, #41484, .T. ) ;
#2450 = ADVANCED_FACE ( 'NONE', ( #19911 ), #15046, .F. ) ;
#2451 = CARTESIAN_POINT ( 'NONE',  ( 0.5110944796929292044, 1.628766292019647954, 2.908232962426333668 ) ) ;
#2452 = ORIENTED_EDGE ( 'NONE', *, *, #24335, .F. ) ;
#2453 = EDGE_LOOP ( 'NONE', ( #8318, #50108, #7998, #14636 ) ) ;
#2454 = VECTOR ( 'NONE', #29535, 39.37007874015748143 ) ;
#2455 = CARTESIAN_POINT ( 'NONE',  ( -1.195183497228115035E-16, 0.000000000000000000, -0.9448818897637765168 ) ) ;
#2456 = CARTESIAN_POINT ( 'NONE',  ( -1.285287856678015705, 0.000000000000000000, -1.251479330189099182 ) ) ;
#2457 = CARTESIAN_POINT ( 'NONE',  ( -1.439733046521776583, 3.346456692913386100, 1.574803149606291530 ) ) ;
#2458 = ORIENTED_EDGE ( 'NONE', *, *, #17814, .F. ) ;
#2459 = CARTESIAN_POINT ( 'NONE',  ( -2.623503965249869729, 1.678368413758691391, 1.355882097269835107 ) ) ;
#2460 = UNCERTAINTY_MEASURE_WITH_UNIT (LENGTH_MEASURE( 1.000000000000000082E-05 ), #9874, 'distance_accuracy_value', 'NONE');
#2461 = CARTESIAN_POINT ( 'NONE',  ( 0.7423782071083088185, 3.267716535433071279, -2.575641807848710687E-16 ) ) ;
#2462 = VERTEX_POINT ( 'NONE', #23539 ) ;
#2463 = EDGE_LOOP ( 'NONE', ( #36514, #44449, #11945, #18136 ) ) ;
#2464 = LINE ( 'NONE', #11218, #15398 ) ;
#2465 = CARTESIAN_POINT ( 'NONE',  ( 0.5455278134075211005, 3.346456692913386100, -1.141732283464564013 ) ) ;
#2466 = AXIS2_PLACEMENT_3D ( 'NONE', #31757, #46453, #11118 ) ;
#2467 = DIRECTION ( 'NONE',  ( 0.000000000000000000, 0.000000000000000000, -1.000000000000000000 ) ) ;
#2468 = B_SPLINE_CURVE_WITH_KNOTS ( 'NONE', 3,
 ( #3511, #19247, #47603, #19753 ),
 .UNSPECIFIED., .F., .F.,
 ( 4, 4 ),
 ( 3.374697576515009854E-07, 0.04668773305404667201 ),
 .UNSPECIFIED. ) ;
#2469 = CARTESIAN_POINT ( 'NONE',  ( 0.2727639067037604947, 0.000000000000000000, -0.1574803149606298636 ) ) ;
#2470 = CARTESIAN_POINT ( 'NONE',  ( 0.5455278134075211005, 3.346456692913386100, -1.456692913385822630 ) ) ;
#2471 = VERTEX_POINT ( 'NONE', #35429 ) ;
#2472 = CARTESIAN_POINT ( 'NONE',  ( -0.6214413264104945434, 0.000000000000000000, 2.047244094488179567 ) ) ;
#2473 = LINE ( 'NONE', #25960, #39681 ) ;
#2474 = AXIS2_PLACEMENT_3D ( 'NONE', #2328, #5431, #10328 ) ;
#2475 = VERTEX_POINT ( 'NONE', #46994 ) ;
#2476 = CARTESIAN_POINT ( 'NONE',  ( -0.1516443935822172906, 1.639856293254567943, -2.233914102096871801 ) ) ;
#2477 = EDGE_CURVE ( 'NONE', #17837, #8483, #23045, .T. ) ;
#2478 = DIRECTION ( 'NONE',  ( -3.469446951953613696E-16, 0.000000000000000000, -1.000000000000000000 ) ) ;
#2479 = ORIENTED_EDGE ( 'NONE', *, *, #48125, .T. ) ;
#2480 = DIRECTION ( 'NONE',  ( -0.000000000000000000, 1.000000000000000000, -0.000000000000000000 ) ) ;
#2481 = EDGE_CURVE ( 'NONE', #31368, #3488, #27410, .T. ) ;
#2482 = CARTESIAN_POINT ( 'NONE',  ( 0.000000000000000000, 6.692913385826772199, 0.000000000000000000 ) ) ;
#2483 = ADVANCED_FACE ( 'NONE', ( #45 ), #3675, .T. ) ;
#2484 = CARTESIAN_POINT ( 'NONE',  ( 0.5455278134075212115, 0.000000000000000000, 0.3149606299212576177 ) ) ;
#2485 = VERTEX_POINT ( 'NONE', #47508 ) ;
#2486 = DIRECTION ( 'NONE',  ( 1.734723475976806848E-16, -0.000000000000000000, 1.000000000000000000 ) ) ;
#2487 = VECTOR ( 'NONE', #3680, 39.37007874015748143 ) ;
#2488 = ORIENTED_EDGE ( 'NONE', *, *, #37151, .F. ) ;
#2489 = FACE_BOUND ( 'NONE', #33894, .T. ) ;
#2490 = DIRECTION ( 'NONE',  ( -0.01601477604151182663, 0.9998717552508123996, -0.000000000000000000 ) ) ;
#2491 = CARTESIAN_POINT ( 'NONE',  ( -1.166969139818015533, 3.346456692913386100, 1.102362204724404160 ) ) ;
#2492 = CARTESIAN_POINT ( 'NONE',  ( 1.232995795418176055, 1.205361022782829114E-17, 1.780798594093568221 ) ) ;
#2493 = EDGE_LOOP ( 'NONE', ( #47521, #11946, #18669, #38887 ) ) ;
#2494 = EDGE_LOOP ( 'NONE', ( #14837, #42039, #15228, #6702 ) ) ;
#2495 = CARTESIAN_POINT ( 'NONE',  ( 0.4696143004045478797, 3.267716535433071279, 0.2755905511810994302 ) ) ;
#2496 = EDGE_CURVE ( 'NONE', #2241, #11767, #15297, .T. ) ;
#2497 = DIRECTION ( 'NONE',  ( -0.000000000000000000, 0.000000000000000000, 1.000000000000000000 ) ) ;
#2498 = ORIENTED_EDGE ( 'NONE', *, *, #37156, .T. ) ;
#2499 = DIRECTION ( 'NONE',  ( -3.986037398843765983E-20, -1.000000000000000000, -1.160734090543304660E-16 ) ) ;
#2500 = EDGE_CURVE ( 'NONE', #25699, #47516, #3931, .T. ) ;
#2501 = ORIENTED_EDGE ( 'NONE', *, *, #36403, .T. ) ;
#2502 = CARTESIAN_POINT ( 'NONE',  ( 0.8182917201112819283, 3.346456692913386100, -0.7874015748031473194 ) ) ;
#2503 = EDGE_CURVE ( 'NONE', #33237, #39972, #20972, .T. ) ;
#2504 = DIRECTION ( 'NONE',  ( 1.000000000000000000, 0.000000000000000000, 0.000000000000000000 ) ) ;
#2505 = ORIENTED_EDGE ( 'NONE', *, *, #15936, .T. ) ;
#2506 = ADVANCED_FACE ( 'NONE', ( #34672 ), #38794, .F. ) ;
#2507 = EDGE_CURVE ( 'NONE', #27595, #23374, #27923, .T. ) ;
#2508 = FACE_OUTER_BOUND ( 'NONE', #29409, .T. ) ;
#2509 = ORIENTED_EDGE ( 'NONE', *, *, #5915, .T. ) ;
#2510 = ORIENTED_EDGE ( 'NONE', *, *, #37730, .F. ) ;
#2511 = VECTOR ( 'NONE', #47422, 39.37007874015748143 ) ;
#2512 = AXIS2_PLACEMENT_3D ( 'NONE', #30832, #26943, #42690 ) ;
#2513 = VERTEX_POINT ( 'NONE', #30794 ) ;
#2514 = ORIENTED_EDGE ( 'NONE', *, *, #9698, .T. ) ;
#2515 = CARTESIAN_POINT ( 'NONE',  ( -1.363819533518803473, 3.346456692913386100, -0.1574803149606300023 ) ) ;
#2516 = ORIENTED_EDGE ( 'NONE', *, *, #37449, .T. ) ;
#2517 = LINE ( 'NONE', #6131, #6491 ) ;
#2518 = CARTESIAN_POINT ( 'NONE',  ( 1.305557278495039775, 1.728812839972934334, -1.880670907523083191 ) ) ;
#2519 = CARTESIAN_POINT ( 'NONE',  ( -1.936702278443778624, 1.582576099004612713, 1.481523253277833740 ) ) ;
#2520 = DIRECTION ( 'NONE',  ( 0.000000000000000000, 0.000000000000000000, 1.000000000000000000 ) ) ;
#2521 = CARTESIAN_POINT ( 'NONE',  ( 1.599172890215259546, 0.000000000000000000, 1.460879300779193590 ) ) ;
#2522 = ORIENTED_EDGE ( 'NONE', *, *, #2990, .T. ) ;
#2523 = CARTESIAN_POINT ( 'NONE',  ( -2.139020239325885253, 1.673641627049041514, 0.3394120305351381872 ) ) ;
#2524 = FACE_OUTER_BOUND ( 'NONE', #18218, .T. ) ;
#2525 = CARTESIAN_POINT ( 'NONE',  ( 2.323794147221719175, 1.745121766917047790, -0.05509951330290247667 ) ) ;
#2526 = DIRECTION ( 'NONE',  ( 0.000000000000000000, -1.000000000000000000, 0.000000000000000000 ) ) ;
#2527 = ORIENTED_EDGE ( 'NONE', *, *, #41949, .F. ) ;
#2528 = CARTESIAN_POINT ( 'NONE',  ( -2.099568260077699033, 1.574803149606302854, -0.5296909464896101261 ) ) ;
#2529 = CARTESIAN_POINT ( 'NONE',  ( 2.138597145901430352, 5.118110236220475784, 0.3393547186367261159 ) ) ;
#2530 = VERTEX_POINT ( 'NONE', #46506 ) ;
#2531 = CARTESIAN_POINT ( 'NONE',  ( 2.088192093915797631, 3.346456692913386100, 0.2755905511810994302 ) ) ;
#2532 = CARTESIAN_POINT ( 'NONE',  ( -2.165177485265463719, 1.673231077555005886, -0.03196544747831084332 ) ) ;
#2533 = EDGE_CURVE ( 'NONE', #32050, #39562, #3426, .T. ) ;
#2534 = VERTEX_POINT ( 'NONE', #18044 ) ;
#2535 = EDGE_CURVE ( 'NONE', #26744, #6661, #44383, .T. ) ;
#2536 = EDGE_LOOP ( 'NONE', ( #23824, #22422, #1061, #6342 ) ) ;
#2537 = CARTESIAN_POINT ( 'NONE',  ( 0.7423782071083084855, 0.000000000000000000, -1.889763779527552812 ) ) ;
#2538 = EDGE_CURVE ( 'NONE', #20750, #13112, #16574, .T. ) ;
#2539 = DIRECTION ( 'NONE',  ( -0.000000000000000000, 1.000000000000000000, -0.000000000000000000 ) ) ;
#2540 = AXIS2_PLACEMENT_3D ( 'NONE', #46306, #2467, #34218 ) ;
#2541 = CARTESIAN_POINT ( 'NONE',  ( 0.002207914879453961969, 5.905511811023623991, 0.04916304461325442243 ) ) ;
#2542 = VECTOR ( 'NONE', #42779, 39.37007874015748143 ) ;
#2543 = CARTESIAN_POINT ( 'NONE',  ( -2.399155757346499218, 1.673679064067194133, 0.3746497807080386155 ) ) ;
#2544 = PLANE ( 'NONE',  #32716 ) ;
#2545 = EDGE_LOOP ( 'NONE', ( #20541, #44905, #9589, #35485, #7751, #29242, #48570, #9649, #7172, #17047, #27660, #5011, #13651 ) ) ;
#2546 = CARTESIAN_POINT ( 'NONE',  ( 0.000000000000000000, 5.905511811023623991, 0.000000000000000000 ) ) ;
#2547 = VERTEX_POINT ( 'NONE', #29913 ) ;
#2548 = ORIENTED_EDGE ( 'NONE', *, *, #44835, .T. ) ;
#2549 = DIRECTION ( 'NONE',  ( -0.000000000000000000, 1.000000000000000000, -0.000000000000000000 ) ) ;
#2550 = ORIENTED_EDGE ( 'NONE', *, *, #43827, .T. ) ;
#2551 = CARTESIAN_POINT ( 'NONE',  ( 0.5455278134075217666, 0.000000000000000000, 1.889763779527550369 ) ) ;
#2552 = VECTOR ( 'NONE', #28318, 39.37007874015748143 ) ;
#2553 = CARTESIAN_POINT ( 'NONE',  ( -1.152114531865843006, 1.205361022782829114E-17, 1.393499336327983729 ) ) ;
#2554 = ORIENTED_EDGE ( 'NONE', *, *, #25354, .F. ) ;
#2555 = DIRECTION ( 'NONE',  ( -0.000000000000000000, 1.000000000000000000, -0.000000000000000000 ) ) ;
#2556 = EDGE_CURVE ( 'NONE', #12830, #11574, #48021, .T. ) ;
#2557 = DIRECTION ( 'NONE',  ( 9.964307797194671432E-17, -1.000000000000000000, -5.953396763000495864E-17 ) ) ;
#2558 = DIRECTION ( 'NONE',  ( 1.000000000000000000, 0.000000000000000000, 0.000000000000000000 ) ) ;
#2559 = ORIENTED_EDGE ( 'NONE', *, *, #23506, .F. ) ;
#2560 = ORIENTED_EDGE ( 'NONE', *, *, #1723, .T. ) ;
#2561 = EDGE_CURVE ( 'NONE', #23674, #14569, #33805, .T. ) ;
#2562 = DIRECTION ( 'NONE',  ( -0.3513748240813434620, 0.000000000000000000, 0.9362348706397368714 ) ) ;
#2563 = FACE_BOUND ( 'NONE', #35204, .T. ) ;
#2564 = ORIENTED_EDGE ( 'NONE', *, *, #231, .F. ) ;
#2565 = CARTESIAN_POINT ( 'NONE',  ( 0.9442395380435398833, 1.624600478255878055, -2.074157072296122450 ) ) ;
#2566 = DIRECTION ( 'NONE',  ( -1.000000000000000000, 0.000000000000000000, -0.000000000000000000 ) ) ;
#2567 = VERTEX_POINT ( 'NONE', #28429 ) ;
#2568 = ORIENTED_EDGE ( 'NONE', *, *, #29344, .T. ) ;
#2569 = DIRECTION ( 'NONE',  ( -0.01601477604151182663, 0.9998717552508123996, -0.000000000000000000 ) ) ;
#2570 = PLANE ( 'NONE',  #14674 ) ;
#2571 = ORIENTED_EDGE ( 'NONE', *, *, #24158, .F. ) ;
#2572 = ORIENTED_EDGE ( 'NONE', *, *, #13681, .T. ) ;
#2573 = ORIENTED_EDGE ( 'NONE', *, *, #46894, .T. ) ;
#2574 = CARTESIAN_POINT ( 'NONE',  ( 0.7572931578342089187, 1.049866565067838486, 1.877743133592741698 ) ) ;
#2575 = VECTOR ( 'NONE', #25824, 39.37007874015748143 ) ;
#2576 = LINE ( 'NONE', #25557, #15910 ) ;
#2577 = VECTOR ( 'NONE', #28841, 39.37007874015748143 ) ;
#2578 = CARTESIAN_POINT ( 'NONE',  ( 1.062992125984252079, 0.000000000000000000, 1.014069264286641570 ) ) ;
#2579 = LINE ( 'NONE', #44910, #42834 ) ;
#2580 = ORIENTED_EDGE ( 'NONE', *, *, #820, .F. ) ;
#2581 = ORIENTED_EDGE ( 'NONE', *, *, #32205, .T. ) ;
#2582 = CARTESIAN_POINT ( 'NONE',  ( 0.2727639067037602172, 3.346456692913386100, -2.148105963102950877 ) ) ;
#2583 = CARTESIAN_POINT ( 'NONE',  ( -0.6214413264104945434, 0.000000000000000000, -1.929133858267710000 ) ) ;
#2584 = DIRECTION ( 'NONE',  ( -5.782411586589357392E-17, -0.000000000000000000, -1.000000000000000000 ) ) ;
#2585 = AXIS2_PLACEMENT_3D ( 'NONE', #7748, #39243, #3883 ) ;
#2586 = CARTESIAN_POINT ( 'NONE',  ( 1.015142113812069091, 3.267716535433071279, -1.614173228346451605 ) ) ;
#2587 = CARTESIAN_POINT ( 'NONE',  ( -0.8240339662865816539, 1.629086743072089005, 2.055573381764717489 ) ) ;
#2588 = VECTOR ( 'NONE', #14851, 39.37007874015748143 ) ;
#2589 = DIRECTION ( 'NONE',  ( 1.734723475976806848E-16, -0.000000000000000000, 1.000000000000000000 ) ) ;
#2590 = DIRECTION ( 'NONE',  ( -3.469446951953613696E-16, 0.000000000000000000, -1.000000000000000000 ) ) ;
#2591 = EDGE_CURVE ( 'NONE', #39943, #48506, #44180, .T. ) ;
#2592 = VERTEX_POINT ( 'NONE', #8823 ) ;
#2593 = DIRECTION ( 'NONE',  ( -1.000000000000000000, 0.000000000000000000, 0.000000000000000000 ) ) ;
#2594 = CARTESIAN_POINT ( 'NONE',  ( -0.3136974817027967100, 1.522126940893053337, -2.936457595020224520 ) ) ;
#2595 = EDGE_CURVE ( 'NONE', #286, #37788, #39416, .T. ) ;
#2596 = ORIENTED_EDGE ( 'NONE', *, *, #39324, .T. ) ;
#2597 = EDGE_CURVE ( 'NONE', #12774, #42097, #17170, .T. ) ;
#2598 = ORIENTED_EDGE ( 'NONE', *, *, #23941, .F. ) ;
#2599 = CARTESIAN_POINT ( 'NONE',  ( -1.439733046521776583, 3.267716535433071279, 1.537421584259135443 ) ) ;
#2600 = EDGE_LOOP ( 'NONE', ( #16707, #9194, #43189, #50480 ) ) ;
#2601 = EDGE_CURVE ( 'NONE', #32050, #50372, #6478, .T. ) ;
#2602 = VERTEX_POINT ( 'NONE', #819 ) ;
#2603 = LINE ( 'NONE', #42096, #19617 ) ;
#2604 = ORIENTED_EDGE ( 'NONE', *, *, #46888, .F. ) ;
#2605 = VECTOR ( 'NONE', #37851, 39.37007874015748143 ) ;
#2606 = DIRECTION ( 'NONE',  ( 1.000000000000000000, -0.000000000000000000, 0.000000000000000000 ) ) ;
#2607 = DIRECTION ( 'NONE',  ( -0.01601477604151182663, 0.9998717552508123996, -0.000000000000000000 ) ) ;
#2608 = AXIS2_PLACEMENT_3D ( 'NONE', #18998, #15884, #11759 ) ;
#2609 = EDGE_CURVE ( 'NONE', #23622, #3117, #25270, .T. ) ;
#2610 = ORIENTED_EDGE ( 'NONE', *, *, #40646, .F. ) ;
#2611 = ORIENTED_EDGE ( 'NONE', *, *, #41833, .T. ) ;
#2612 = VECTOR ( 'NONE', #17528, 39.37007874015748143 ) ;
#2613 = CARTESIAN_POINT ( 'NONE',  ( 2.951990591674675368, 0.000000000000000000, -0.08331184815398383348 ) ) ;
#2614 = ORIENTED_EDGE ( 'NONE', *, *, #34073, .F. ) ;
#2615 = ORIENTED_EDGE ( 'NONE', *, *, #12126, .F. ) ;
#2616 = EDGE_CURVE ( 'NONE', #972, #5208, #21617, .T. ) ;
#2617 = CARTESIAN_POINT ( 'NONE',  ( -2.216704495933535579, 1.676569812073664512, -1.000984397190004094 ) ) ;
#2618 = DIRECTION ( 'NONE',  ( -1.000000000000000000, 0.000000000000000000, -0.000000000000000000 ) ) ;
#2620 = DIRECTION ( 'NONE',  ( -0.000000000000000000, 1.000000000000000000, -0.000000000000000000 ) ) ;
#2619 = VECTOR ( 'NONE', #14689, 39.37007874015748854 ) ;
#2621 = CARTESIAN_POINT ( 'NONE',  ( -1.091055626815042201, 3.267716535433071279, 1.062992125984246083 ) ) ;
#2622 = AXIS2_PLACEMENT_3D ( 'NONE', #46495, #11164, #35672 ) ;
#2623 = ORIENTED_EDGE ( 'NONE', *, *, #1211, .F. ) ;
#2624 = DIRECTION ( 'NONE',  ( 0.9998717552508121775, 0.01601477604151182663, 0.000000000000000000 ) ) ;
#2625 = FACE_OUTER_BOUND ( 'NONE', #19248, .T. ) ;
#2626 = CARTESIAN_POINT ( 'NONE',  ( -1.743268982565497449, 0.0004610889948519912205, -0.02902809809614041725 ) ) ;
#2627 = EDGE_LOOP ( 'NONE', ( #34197, #13549, #40584, #24964 ) ) ;
#2628 = CARTESIAN_POINT ( 'NONE',  ( 0.07982360342473591996, 1.709180471932028711, 0.000000000000000000 ) ) ;
#2629 = DIRECTION ( 'NONE',  ( -0.000000000000000000, 1.000000000000000000, -0.000000000000000000 ) ) ;
#2630 = CARTESIAN_POINT ( 'NONE',  ( -1.363819533518803029, 0.000000000000000000, 0.4724409448818871482 ) ) ;
#2631 = ORIENTED_EDGE ( 'NONE', *, *, #13029, .T. ) ;
#2632 = EDGE_LOOP ( 'NONE', ( #19838, #19520, #47143, #50541 ) ) ;
#2633 =( CONVERSION_BASED_UNIT ( 'INCH', #38015 ) LENGTH_UNIT ( ) NAMED_UNIT ( #47178 ) );
#2634 = ADVANCED_FACE ( 'NONE', ( #20172 ), #36139, .F. ) ;
#2635 = DIRECTION ( 'NONE',  ( -0.000000000000000000, 1.000000000000000000, -0.000000000000000000 ) ) ;
#2636 = DIRECTION ( 'NONE',  ( -1.000000000000000000, 0.000000000000000000, -0.000000000000000000 ) ) ;
#2637 = DIRECTION ( 'NONE',  ( 3.986037398843765983E-20, 1.000000000000000000, 1.160734090543304660E-16 ) ) ;
#2638 = ORIENTED_EDGE ( 'NONE', *, *, #48244, .T. ) ;
#2639 = ORIENTED_EDGE ( 'NONE', *, *, #41074, .T. ) ;
#2640 = SURFACE_STYLE_USAGE ( .BOTH. , #18894 ) ;
#2641 = CARTESIAN_POINT ( 'NONE',  ( -0.7329371533687082385, 1.663354224513332591, 2.092961330735970904 ) ) ;
#2642 = ORIENTED_EDGE ( 'NONE', *, *, #20952, .T. ) ;
#2643 = CARTESIAN_POINT ( 'NONE',  ( 2.074656761899007495, 1.205361022782829114E-17, -0.6223516566630619140 ) ) ;
#2644 = LINE ( 'NONE', #18391, #26774 ) ;
#2645 = AXIS2_PLACEMENT_3D ( 'NONE', #23311, #43176, #38573 ) ;
#2646 = CARTESIAN_POINT ( 'NONE',  ( 0.002207914879453961535, -5.712274067634378313E-18, 0.04916304461325374242 ) ) ;
#2647 = CARTESIAN_POINT ( 'NONE',  ( -1.166969139818016199, 3.346456692913386100, -0.9842519685039344823 ) ) ;
#2649 = CARTESIAN_POINT ( 'NONE',  ( -0.6214413264104939882, 0.000000000000000000, 1.220472440944875281 ) ) ;
#2648 = AXIS2_PLACEMENT_3D ( 'NONE', #26799, #42292, #18811 ) ;
#2650 = ORIENTED_EDGE ( 'NONE', *, *, #27329, .F. ) ;
#2651 = CARTESIAN_POINT ( 'NONE',  ( 2.259006893506616986, 1.652495484661263836, -1.550124774990060628 ) ) ;
#2652 = LINE ( 'NONE', #22525, #15322 ) ;
#2653 = VECTOR ( 'NONE', #29557, 39.37007874015748143 ) ;
#2654 = LINE ( 'NONE', #15034, #19100 ) ;
#2655 = EDGE_CURVE ( 'NONE', #21677, #13391, #15391, .T. ) ;
#2656 = ORIENTED_EDGE ( 'NONE', *, *, #21895, .T. ) ;
#2657 = AXIS2_PLACEMENT_3D ( 'NONE', #3801, #26776, #19279 ) ;
#2658 = LINE ( 'NONE', #10664, #24883 ) ;
#2659 = DIRECTION ( 'NONE',  ( -5.782411586589357392E-17, 0.000000000000000000, -1.000000000000000000 ) ) ;
#2660 = CARTESIAN_POINT ( 'NONE',  ( 1.363819533518803251, 0.000000000000000000, 0.2755905511810996522 ) ) ;
#2661 = ADVANCED_FACE ( 'NONE', ( #5908 ), #43920, .F. ) ;
#2662 = ORIENTED_EDGE ( 'NONE', *, *, #41443, .F. ) ;
#2663 = EDGE_CURVE ( 'NONE', #31145, #39431, #12433, .T. ) ;
#2664 = CARTESIAN_POINT ( 'NONE',  ( 2.378961647330872786, 3.267716535433071279, -1.161035397307311917E-15 ) ) ;
#2665 = ORIENTED_EDGE ( 'NONE', *, *, #21611, .F. ) ;
#2666 = DIRECTION ( 'NONE',  ( 0.000000000000000000, 0.000000000000000000, -1.000000000000000000 ) ) ;
#2667 = ORIENTED_EDGE ( 'NONE', *, *, #8525, .F. ) ;
#2668 = CARTESIAN_POINT ( 'NONE',  ( -1.091055626815042645, 0.000000000000000000, 1.692913385826762873 ) ) ;
#2669 = CARTESIAN_POINT ( 'NONE',  ( 1.015142113812069091, 3.267716535433071279, -3.521981712565030910E-16 ) ) ;
#2670 = CARTESIAN_POINT ( 'NONE',  ( 0.000000000000000000, 6.692913385826772199, 0.000000000000000000 ) ) ;
#2671 = CARTESIAN_POINT ( 'NONE',  ( 1.716372756112214626, 1.049866565877818347, -1.074000356430005798 ) ) ;
#2672 = ADVANCED_FACE ( 'NONE', ( #21658 ), #2041, .F. ) ;
#2673 = VERTEX_POINT ( 'NONE', #25783 ) ;
#2674 = ORIENTED_EDGE ( 'NONE', *, *, #19897, .F. ) ;
#2675 = DIRECTION ( 'NONE',  ( -3.469446951953613696E-16, 0.000000000000000000, -1.000000000000000000 ) ) ;
#2676 = CARTESIAN_POINT ( 'NONE',  ( 1.661821349926414726, 1.574803149606302854, 1.388203579611976268 ) ) ;
#2677 = VERTEX_POINT ( 'NONE', #6170 ) ;
#2678 = FACE_OUTER_BOUND ( 'NONE', #15132, .T. ) ;
#2679 = CARTESIAN_POINT ( 'NONE',  ( 0.8182917201112819283, 3.267716535433071279, 0.2755905511810994302 ) ) ;
#2680 = CARTESIAN_POINT ( 'NONE',  ( 0.7423782071083085965, 3.346456692913386100, 0.7480314960629872445 ) ) ;
#2681 = ORIENTED_EDGE ( 'NONE', *, *, #39283, .F. ) ;
#2682 = CIRCLE ( 'NONE', #25749, 2.164630168518208109 ) ;
#2683 = ORIENTED_EDGE ( 'NONE', *, *, #29505, .T. ) ;
#2684 = DIRECTION ( 'NONE',  ( 5.779879058770898378E-18, 1.000000000000000000, 1.286990067732318227E-16 ) ) ;
#2685 = CARTESIAN_POINT ( 'NONE',  ( -2.043634885149970160, 6.692913385826772199, 0.7157624142945935297 ) ) ;
#2686 = EDGE_CURVE ( 'NONE', #3807, #4133, #21919, .T. ) ;
#2687 = LINE ( 'NONE', #42175, #23899 ) ;
#2688 = EDGE_LOOP ( 'NONE', ( #6169, #6988, #41784, #45022, #137, #30100, #45760, #17085, #36619, #17847, #20834 ) ) ;
#2689 = CARTESIAN_POINT ( 'NONE',  ( -2.308557526972533136, 0.000000000000000000, 1.841013194464759639 ) ) ;
#2690 = CIRCLE ( 'NONE', #37345, 2.165354330708661568 ) ;
#2691 = FACE_BOUND ( 'NONE', #4794, .T. ) ;
#2692 = EDGE_LOOP ( 'NONE', ( #31759, #49098, #33816, #34064 ) ) ;
#2693 = CARTESIAN_POINT ( 'NONE',  ( -0.5455278134075216556, 3.267716535433071279, -2.381957271744193250 ) ) ;
#2694 = ORIENTED_EDGE ( 'NONE', *, *, #4583, .T. ) ;
#2695 = EDGE_LOOP ( 'NONE', ( #5623, #45545, #49439, #35314 ) ) ;
#2696 = CARTESIAN_POINT ( 'NONE',  ( 0.2509224957585530213, 1.679112537684454676, -2.238970375727059370 ) ) ;
#2697 = CARTESIAN_POINT ( 'NONE',  ( -1.326676825859837816, 1.205361022782829114E-17, -1.200346386814097999 ) ) ;
#2698 = ADVANCED_FACE ( 'NONE', ( #2802 ), #6928, .F. ) ;
#2699 = CONICAL_SURFACE ( 'NONE', #44721, 1.850107469027523210, 0.6386652850508578450 ) ;
#2700 = AXIS2_PLACEMENT_3D ( 'NONE', #21274, #1646, #17399 ) ;
#2701 = CARTESIAN_POINT ( 'NONE',  ( 0.07982360342473591996, 1.709180471932028711, 0.000000000000000000 ) ) ;
#2702 = CARTESIAN_POINT ( 'NONE',  ( 0.000000000000000000, 3.267716535433071279, 0.2755905511810994302 ) ) ;
#2703 = LINE ( 'NONE', #49144, #46078 ) ;
#2704 = ORIENTED_EDGE ( 'NONE', *, *, #16102, .T. ) ;
#2705 = EDGE_CURVE ( 'NONE', #9409, #7396, #46141, .T. ) ;
#2706 = ORIENTED_EDGE ( 'NONE', *, *, #24843, .F. ) ;
#2707 = LINE ( 'NONE', #11470, #20330 ) ;
#2708 = FACE_OUTER_BOUND ( 'NONE', #33108, .T. ) ;
#2709 = EDGE_CURVE ( 'NONE', #33470, #13670, #38428, .T. ) ;
#2710 = DIRECTION ( 'NONE',  ( 0.000000000000000000, -1.000000000000000000, 0.000000000000000000 ) ) ;
#2711 = DIRECTION ( 'NONE',  ( 1.000000000000000000, -0.000000000000000000, 0.000000000000000000 ) ) ;
#2712 = CARTESIAN_POINT ( 'NONE',  ( -1.930387128362887283, 1.555218655107503789, 2.234422008625466471 ) ) ;
#2713 = VERTEX_POINT ( 'NONE', #37928 ) ;
#2714 = CARTESIAN_POINT ( 'NONE',  ( -0.5455278134075214336, 0.000000000000000000, -0.6299212598425175669 ) ) ;
#2715 = CARTESIAN_POINT ( 'NONE',  ( 1.743145509346915256, 0.000000000000000000, -0.02902255290747513330 ) ) ;
#2716 = ADVANCED_FACE ( 'NONE', ( #46883 ), #49993, .F. ) ;
#2717 = ORIENTED_EDGE ( 'NONE', *, *, #28917, .F. ) ;
#2718 = LINE ( 'NONE', #34724, #2588 ) ;
#2719 = CARTESIAN_POINT ( 'NONE',  ( 0.000000000000000000, 1.574803149606302854, 0.000000000000000000 ) ) ;
#2720 = VERTEX_POINT ( 'NONE', #30675 ) ;
#2721 = CYLINDRICAL_SURFACE ( 'NONE', #3171, 2.164630168518208109 ) ;
#2722 = EDGE_CURVE ( 'NONE', #24890, #48785, #11308, .T. ) ;
#2723 = LINE ( 'NONE', #46070, #30082 ) ;
#2724 = EDGE_CURVE ( 'NONE', #25196, #30067, #46639, .T. ) ;
#2725 = LINE ( 'NONE', #14603, #23525 ) ;
#2726 = VECTOR ( 'NONE', #30564, 39.37007874015748143 ) ;
#2727 = B_SPLINE_CURVE_WITH_KNOTS ( 'NONE', 3,
 ( #37920, #18037, #34301, #10287 ),
 .UNSPECIFIED., .F., .F.,
 ( 4, 4 ),
 ( 0.1211775127643062860, 0.1625894504277921315 ),
 .UNSPECIFIED. ) ;
#2728 = ORIENTED_EDGE ( 'NONE', *, *, #47181, .T. ) ;
#2729 = CARTESIAN_POINT ( 'NONE',  ( -0.8942052331142552601, 0.000000000000000000, -7.512581982576723358E-16 ) ) ;
#2730 = ORIENTED_EDGE ( 'NONE', *, *, #40773, .T. ) ;
#2731 = FACE_BOUND ( 'NONE', #13357, .T. ) ;
#2732 = CARTESIAN_POINT ( 'NONE',  ( -0.3486774197067334380, 0.000000000000000000, 0.6299212598425164567 ) ) ;
#2733 = VECTOR ( 'NONE', #11892, 39.37007874015748143 ) ;
#2734 = LINE ( 'NONE', #26471, #39983 ) ;
#2735 = LINE ( 'NONE', #17723, #2918 ) ;
#2736 = VERTEX_POINT ( 'NONE', #50238 ) ;
#2737 = ORIENTED_EDGE ( 'NONE', *, *, #32580, .F. ) ;
#2738 = CARTESIAN_POINT ( 'NONE',  ( 2.153610746787201435, 1.643970771453353130, -0.8669779829368272628 ) ) ;
#2739 = VECTOR ( 'NONE', #27011, 39.37007874015748143 ) ;
#2740 = CARTESIAN_POINT ( 'NONE',  ( -1.636583440222564301, 3.267716535433071279, -1.456692913385822186 ) ) ;
#2741 = DIRECTION ( 'NONE',  ( -0.000000000000000000, 1.000000000000000000, -0.000000000000000000 ) ) ;
#2742 = DIRECTION ( 'NONE',  ( 1.734723475976806848E-16, -0.000000000000000000, 1.000000000000000000 ) ) ;
#2743 = DIRECTION ( 'NONE',  ( 0.000000000000000000, 0.000000000000000000, 1.000000000000000000 ) ) ;
#2744 = ORIENTED_EDGE ( 'NONE', *, *, #7404, .F. ) ;
#2745 = VERTEX_POINT ( 'NONE', #3055 ) ;
#2746 = DIRECTION ( 'NONE',  ( -0.000000000000000000, 1.000000000000000000, -0.000000000000000000 ) ) ;
#2747 = EDGE_CURVE ( 'NONE', #43721, #6632, #45887, .T. ) ;
#2748 = B_SPLINE_CURVE_WITH_KNOTS ( 'NONE', 3,
 ( #23805, #23293, #4437, #39552 ),
 .UNSPECIFIED., .F., .F.,
 ( 4, 4 ),
 ( 0.01320882309506746059, 0.03074212603091753399 ),
 .UNSPECIFIED. ) ;
#2749 = CARTESIAN_POINT ( 'NONE',  ( 0.2727639067037602172, 3.346456692913386100, -1.929133858267710000 ) ) ;
#2750 = ORIENTED_EDGE ( 'NONE', *, *, #47124, .F. ) ;
#2751 = CARTESIAN_POINT ( 'NONE',  ( 1.015142113812069313, 3.267716535433071279, 0.1574803149606286423 ) ) ;
#2752 = VERTEX_POINT ( 'NONE', #14928 ) ;
#2753 = VERTEX_POINT ( 'NONE', #10795 ) ;
#2754 = EDGE_CURVE ( 'NONE', #3488, #51000, #14678, .T. ) ;
#2755 = EDGE_CURVE ( 'NONE', #26908, #33352, #36962, .T. ) ;
#2756 = ADVANCED_FACE ( 'NONE', ( #6425 ), #42542, .T. ) ;
#2757 = ORIENTED_EDGE ( 'NONE', *, *, #13860, .F. ) ;
#2758 = ORIENTED_EDGE ( 'NONE', *, *, #18868, .T. ) ;
#2759 = DIRECTION ( 'NONE',  ( 1.734723475976806848E-16, -0.000000000000000000, 1.000000000000000000 ) ) ;
#2760 = AXIS2_PLACEMENT_3D ( 'NONE', #17106, #41615, #20974 ) ;
#2761 = ORIENTED_EDGE ( 'NONE', *, *, #15896, .T. ) ;
#2762 = VECTOR ( 'NONE', #2856, 39.37007874015748143 ) ;
#2763 = DIRECTION ( 'NONE',  ( 1.734723475976806848E-16, 0.000000000000000000, 1.000000000000000000 ) ) ;
#2764 = LINE ( 'NONE', #12294, #7112 ) ;
#2765 = VECTOR ( 'NONE', #3754, 39.37007874015748143 ) ;
#2766 = CIRCLE ( 'NONE', #37425, 2.165354330708661568 ) ;
#2767 = B_SPLINE_CURVE_WITH_KNOTS ( 'NONE', 3,
 ( #17208, #28558, #24702, #5072 ),
 .UNSPECIFIED., .F., .F.,
 ( 4, 4 ),
 ( 0.01476714571944508919, 0.03075156743765733100 ),
 .UNSPECIFIED. ) ;
#2768 = CARTESIAN_POINT ( 'NONE',  ( 0.000000000000000000, 0.000000000000000000, 2.952755905511811108 ) ) ;
#2769 = DIRECTION ( 'NONE',  ( 5.175581015019631661E-17, -0.9063077870366510469, 0.4226182617406972208 ) ) ;
#2770 = FACE_OUTER_BOUND ( 'NONE', #15780, .T. ) ;
#2771 = VECTOR ( 'NONE', #40117, 39.37007874015748143 ) ;
#2772 = ORIENTED_EDGE ( 'NONE', *, *, #37237, .F. ) ;
#2773 = CARTESIAN_POINT ( 'NONE',  ( 1.129352609985932121, 1.660373803670742721, 1.986167711467785368 ) ) ;
#2774 = DIRECTION ( 'NONE',  ( 0.000000000000000000, 0.000000000000000000, 1.000000000000000000 ) ) ;
#2775 = CARTESIAN_POINT ( 'NONE',  ( -1.091055626815042645, 3.346456692913386100, -1.259842519685034690 ) ) ;
#2776 = CARTESIAN_POINT ( 'NONE',  ( 1.560669927219590525, 3.346456692913386100, -0.6692913385826764205 ) ) ;
#2777 = EDGE_CURVE ( 'NONE', #42794, #19022, #7185, .T. ) ;
#2778 = VERTEX_POINT ( 'NONE', #22926 ) ;
#2779 = DIRECTION ( 'NONE',  ( 0.000000000000000000, -1.000000000000000000, 0.000000000000000000 ) ) ;
#2780 = CARTESIAN_POINT ( 'NONE',  ( 1.015142113812069313, 3.267716535433071279, -1.102362204724405714 ) ) ;
#2781 = ORIENTED_EDGE ( 'NONE', *, *, #12812, .T. ) ;
#2782 = CARTESIAN_POINT ( 'NONE',  ( -0.8942052331142547050, 0.000000000000000000, 1.259842519685033357 ) ) ;
#2783 = B_SPLINE_CURVE_WITH_KNOTS ( 'NONE', 3,
 ( #48143, #12820, #19525, #47113 ),
 .UNSPECIFIED., .F., .F.,
 ( 4, 4 ),
 ( 0.1211873102087489551, 0.1625992483279400103 ),
 .UNSPECIFIED. ) ;
#2784 = EDGE_CURVE ( 'NONE', #15952, #45538, #14853, .T. ) ;
#2785 = CARTESIAN_POINT ( 'NONE',  ( -0.5455278134075214336, 3.346456692913386100, -1.141732283464563791 ) ) ;
#2786 = EDGE_CURVE ( 'NONE', #11424, #14385, #19042, .T. ) ;
#2787 = EDGE_LOOP ( 'NONE', ( #23679, #21720, #40074, #26383 ) ) ;
#2788 = EDGE_CURVE ( 'NONE', #18489, #46962, #42284, .T. ) ;
#2789 = CARTESIAN_POINT ( 'NONE',  ( 1.833433833923351353, 3.346456692913386100, -0.6299212598425181220 ) ) ;
#2790 = ORIENTED_EDGE ( 'NONE', *, *, #43736, .T. ) ;
#2791 = FACE_OUTER_BOUND ( 'NONE', #36958, .T. ) ;
#2792 = CARTESIAN_POINT ( 'NONE',  ( -1.567214440306964107, 0.002817858044914879883, 0.7874684655159520652 ) ) ;
#2793 = DIRECTION ( 'NONE',  ( 1.000000000000000000, 0.000000000000000000, 0.000000000000000000 ) ) ;
#2794 = CARTESIAN_POINT ( 'NONE',  ( -2.009930929872525418, 6.692913385826772199, -0.8055662819784122908 ) ) ;
#2795 = DIRECTION ( 'NONE',  ( 1.734723475976806848E-16, -0.000000000000000000, 1.000000000000000000 ) ) ;
#2796 = ORIENTED_EDGE ( 'NONE', *, *, #45299, .T. ) ;
#2797 = DIRECTION ( 'NONE',  ( 0.000000000000000000, -1.000000000000000000, 0.000000000000000000 ) ) ;
#2798 = VECTOR ( 'NONE', #32690, 39.37007874015748143 ) ;
#2799 = ORIENTED_EDGE ( 'NONE', *, *, #13198, .F. ) ;
#2800 = ORIENTED_EDGE ( 'NONE', *, *, #6201, .T. ) ;
#2801 = VECTOR ( 'NONE', #44909, 39.37007874015748143 ) ;
#2802 = FACE_OUTER_BOUND ( 'NONE', #12291, .T. ) ;
#2803 = VERTEX_POINT ( 'NONE', #18294 ) ;
#2804 = DIRECTION ( 'NONE',  ( -1.000000000000000000, -0.000000000000000000, -0.000000000000000000 ) ) ;
#2805 = AXIS2_PLACEMENT_3D ( 'NONE', #30159, #38173, #18543 ) ;
#2806 = DIRECTION ( 'NONE',  ( -0.000000000000000000, 1.000000000000000000, -0.000000000000000000 ) ) ;
#2807 = B_SPLINE_CURVE_WITH_KNOTS ( 'NONE', 3,
 ( #28351, #17009, #44101, #9766 ),
 .UNSPECIFIED., .F., .F.,
 ( 4, 4 ),
 ( 3.600755517447333241E-07, 0.04362148976465617112 ),
 .UNSPECIFIED. ) ;
#2808 = ORIENTED_EDGE ( 'NONE', *, *, #34482, .F. ) ;
#2809 = CIRCLE ( 'NONE', #18471, 2.165354330708661568 ) ;
#2810 = CARTESIAN_POINT ( 'NONE',  ( 0.4330136603435741360, 0.5160455853568218787, -0.4330136603435745246 ) ) ;
#2811 = DIRECTION ( 'NONE',  ( -0.000000000000000000, 1.000000000000000000, -0.000000000000000000 ) ) ;
#2812 = VECTOR ( 'NONE', #22468, 39.37007874015748143 ) ;
#2813 = CARTESIAN_POINT ( 'NONE',  ( 1.636583440222563857, 0.000000000000000000, -1.161035397307311917E-15 ) ) ;
#2814 = EDGE_LOOP ( 'NONE', ( #41167, #32354, #23924, #9809 ) ) ;
#2815 = ORIENTED_EDGE ( 'NONE', *, *, #298, .T. ) ;
#2816 = LINE ( 'NONE', #29927, #16627 ) ;
#2817 = FACE_BOUND ( 'NONE', #22157, .T. ) ;
#2818 = ORIENTED_EDGE ( 'NONE', *, *, #26777, .F. ) ;
#2819 = CARTESIAN_POINT ( 'NONE',  ( 0.2727639067037610499, 0.000000000000000000, 1.102362204724404160 ) ) ;
#2820 = CARTESIAN_POINT ( 'NONE',  ( 2.076281802138679300, 3.267716535433071279, -0.3543307086614178592 ) ) ;
#2821 = EDGE_CURVE ( 'NONE', #1831, #22006, #14423, .T. ) ;
#2822 = VERTEX_POINT ( 'NONE', #26294 ) ;
#2823 = ORIENTED_EDGE ( 'NONE', *, *, #10811, .F. ) ;
#2824 = CARTESIAN_POINT ( 'NONE',  ( -0.8182917201112818173, 3.267716535433071279, 1.419509857074483292E-16 ) ) ;
#2825 = EDGE_CURVE ( 'NONE', #38085, #18489, #42040, .T. ) ;
#2826 = CARTESIAN_POINT ( 'NONE',  ( -0.9156248155784967313, 2.755905511811024056, 1.033395398741681293 ) ) ;
#2827 = B_SPLINE_CURVE_WITH_KNOTS ( 'NONE', 3,
 ( #29053, #5313, #1696, #5571 ),
 .UNSPECIFIED., .F., .F.,
 ( 4, 4 ),
 ( 0.07024079619148275444, 0.1174078461799845929 ),
 .UNSPECIFIED. ) ;
#2828 = EDGE_LOOP ( 'NONE', ( #11380, #18244, #20241, #10926 ) ) ;
#2829 = B_SPLINE_CURVE_WITH_KNOTS ( 'NONE', 3,
 ( #26609, #15691, #26360, #39956 ),
 .UNSPECIFIED., .F., .F.,
 ( 4, 4 ),
 ( 0.001847190087347970510, 0.04527886744616707593 ),
 .UNSPECIFIED. ) ;
#2830 = ORIENTED_EDGE ( 'NONE', *, *, #23546, .T. ) ;
#2831 = LINE ( 'NONE', #46165, #28508 ) ;
#2832 = CARTESIAN_POINT ( 'NONE',  ( -1.181102362204724088, 0.5905511811023621549, 1.062992125984251635 ) ) ;
#2833 = DIRECTION ( 'NONE',  ( -0.000000000000000000, 1.000000000000000000, -0.000000000000000000 ) ) ;
#2834 = VERTEX_POINT ( 'NONE', #19544 ) ;
#2835 = VERTEX_POINT ( 'NONE', #35561 ) ;
#2836 = FACE_OUTER_BOUND ( 'NONE', #27778, .T. ) ;
#2837 = PLANE ( 'NONE',  #45935 ) ;
#2838 = VECTOR ( 'NONE', #24868, 39.37007874015748143 ) ;
#2839 = LINE ( 'NONE', #29444, #14263 ) ;
#2840 = EDGE_CURVE ( 'NONE', #1425, #25537, #35818, .T. ) ;
#2841 = CARTESIAN_POINT ( 'NONE',  ( 0.2928062650698783909, 1.621632777088613198, -2.704337167149358567 ) ) ;
#2842 = VECTOR ( 'NONE', #47643, 39.37007874015748143 ) ;
#2843 = PLANE ( 'NONE',  #48668 ) ;
#2844 = AXIS2_PLACEMENT_3D ( 'NONE', #37146, #20875, #8745 ) ;
#2845 = EDGE_CURVE ( 'NONE', #16391, #11818, #4579, .T. ) ;
#2846 = DIRECTION ( 'NONE',  ( 2.866708903754326305E-17, 1.000000000000000000, 1.255987235303924321E-16 ) ) ;
#2847 = EDGE_CURVE ( 'NONE', #18948, #5697, #47901, .T. ) ;
#2848 = CIRCLE ( 'NONE', #9450, 2.952755905511811552 ) ;
#2849 = ORIENTED_EDGE ( 'NONE', *, *, #23615, .F. ) ;
#2850 = LINE ( 'NONE', #38726, #12680 ) ;
#2851 = DIRECTION ( 'NONE',  ( -0.000000000000000000, 1.000000000000000000, -0.000000000000000000 ) ) ;
#2852 = EDGE_CURVE ( 'NONE', #46840, #24596, #28805, .T. ) ;
#2853 = EDGE_CURVE ( 'NONE', #1578, #12830, #23940, .T. ) ;
#2854 = VERTEX_POINT ( 'NONE', #447 ) ;
#2855 = ORIENTED_EDGE ( 'NONE', *, *, #43113, .F. ) ;
#2856 = DIRECTION ( 'NONE',  ( -1.000000000000000000, -0.000000000000000000, -0.000000000000000000 ) ) ;
#2857 = DIRECTION ( 'NONE',  ( -1.000000000000000000, -0.000000000000000000, -0.000000000000000000 ) ) ;
#2858 = ORIENTED_EDGE ( 'NONE', *, *, #857, .F. ) ;
#2859 = ORIENTED_EDGE ( 'NONE', *, *, #12292, .F. ) ;
#2860 = CARTESIAN_POINT ( 'NONE',  ( 0.000000000000000000, 3.267716535433071279, -0.03937007874015881204 ) ) ;
#2861 = ORIENTED_EDGE ( 'NONE', *, *, #45624, .F. ) ;
#2862 = CARTESIAN_POINT ( 'NONE',  ( 1.363819533518803029, 3.346456692913386100, -1.299212598425193210 ) ) ;
#2863 = CARTESIAN_POINT ( 'NONE',  ( 0.8182917201112819283, 0.000000000000000000, 0.4724409448818868706 ) ) ;
#2864 = ORIENTED_EDGE ( 'NONE', *, *, #5171, .F. ) ;
#2865 = APPLICATION_CONTEXT ( 'automotive_design' ) ;
#2866 = CARTESIAN_POINT ( 'NONE',  ( 2.437165669488590147, 1.655293914011273682, 1.255609184467661565 ) ) ;
#2867 = VECTOR ( 'NONE', #49148, 39.37007874015748143 ) ;
#2868 = ORIENTED_EDGE ( 'NONE', *, *, #21726, .T. ) ;
#2869 = VERTEX_POINT ( 'NONE', #50989 ) ;
#2870 = VECTOR ( 'NONE', #30210, 39.37007874015748143 ) ;
#2871 = CARTESIAN_POINT ( 'NONE',  ( 0.5905511811023621549, 0.000000000000000000, -4.133858267716536083 ) ) ;
#2872 = CARTESIAN_POINT ( 'NONE',  ( -0.5110942158649443012, 1.612844421080423585, 2.908233010304054122 ) ) ;
#2873 = FACE_OUTER_BOUND ( 'NONE', #31931, .T. ) ;
#2874 = DIRECTION ( 'NONE',  ( -3.986037398843765983E-20, -1.000000000000000000, -1.160734090543304660E-16 ) ) ;
#2875 = AXIS2_PLACEMENT_3D ( 'NONE', #21279, #21789, #13790 ) ;
#2876 = EDGE_LOOP ( 'NONE', ( #31617, #49159, #47406, #47144 ) ) ;
#2877 = FACE_OUTER_BOUND ( 'NONE', #39614, .T. ) ;
#2878 = LINE ( 'NONE', #30248, #21744 ) ;
#2879 = CARTESIAN_POINT ( 'NONE',  ( -0.2727639067037611054, 3.267716535433071279, -2.244094488188968395 ) ) ;
#2880 = ORIENTED_EDGE ( 'NONE', *, *, #41807, .T. ) ;
#2881 = DIRECTION ( 'NONE',  ( -0.9998717552508121775, -0.01601477604151182316, 0.000000000000000000 ) ) ;
#2882 = EDGE_CURVE ( 'NONE', #10927, #9086, #12324, .T. ) ;
#2883 = VECTOR ( 'NONE', #27287, 39.37007874015748143 ) ;
#2884 = EDGE_CURVE ( 'NONE', #13726, #31313, #19796, .T. ) ;
#2885 = ORIENTED_EDGE ( 'NONE', *, *, #3547, .F. ) ;
#2886 = ORIENTED_EDGE ( 'NONE', *, *, #18926, .F. ) ;
#2887 =( NAMED_UNIT ( * ) PLANE_ANGLE_UNIT ( ) SI_UNIT ( $, .RADIAN. ) );
#2888 = EDGE_CURVE ( 'NONE', #50909, #6728, #4319, .T. ) ;
#2889 = DIRECTION ( 'NONE',  ( -3.469446951953613696E-16, 0.000000000000000000, -1.000000000000000000 ) ) ;
#2890 = CARTESIAN_POINT ( 'NONE',  ( -2.327682539360300229, 1.048322422875415105, -1.048418689369857715 ) ) ;
#2891 = LINE ( 'NONE', #19131, #26344 ) ;
#2892 = ORIENTED_EDGE ( 'NONE', *, *, #18984, .F. ) ;
#2893 = ORIENTED_EDGE ( 'NONE', *, *, #41242, .F. ) ;
#2894 = CARTESIAN_POINT ( 'NONE',  ( -0.9959141369039302694, 1.049866565067838264, 1.762829326557763254 ) ) ;
#2895 = DIRECTION ( 'NONE',  ( 3.986037398843765983E-20, 1.000000000000000000, 1.160734090543304660E-16 ) ) ;
#2896 = EDGE_LOOP ( 'NONE', ( #11511, #30166, #37758, #3468 ) ) ;
#2897 = FACE_OUTER_BOUND ( 'NONE', #36066, .T. ) ;
#2898 = DIRECTION ( 'NONE',  ( 1.000000000000000000, -0.000000000000000000, 0.000000000000000000 ) ) ;
#2899 = EDGE_CURVE ( 'NONE', #13855, #7934, #28057, .T. ) ;
#2900 = CARTESIAN_POINT ( 'NONE',  ( -2.338262049203568171, 5.118110236220475784, -0.7080022065394827591 ) ) ;
#2901 = DIRECTION ( 'NONE',  ( -0.8439299085898972486, 0.000000000000000000, 0.5364534550056021533 ) ) ;
#2902 = CYLINDRICAL_SURFACE ( 'NONE', #50080, 2.854330708661417138 ) ;
#2903 = ORIENTED_EDGE ( 'NONE', *, *, #41295, .F. ) ;
#2904 = CIRCLE ( 'NONE', #36703, 1.743387098533651480 ) ;
#2905 = DIRECTION ( 'NONE',  ( -0.000000000000000000, 0.000000000000000000, 1.000000000000000000 ) ) ;
#2906 = CARTESIAN_POINT ( 'NONE',  ( 0.1155636338427008941, -0.5222242541845523167, 0.000000000000000000 ) ) ;
#2907 = CIRCLE ( 'NONE', #28468, 2.165354330708661568 ) ;
#2908 = EDGE_CURVE ( 'NONE', #19682, #37143, #20049, .T. ) ;
#2909 = VECTOR ( 'NONE', #33784, 39.37007874015748143 ) ;
#2910 = CARTESIAN_POINT ( 'NONE',  ( -2.277873973731453727, 1.562946399538843290, 1.879489153247635214 ) ) ;
#2911 = VECTOR ( 'NONE', #27412, 39.37007874015748143 ) ;
#2912 = ORIENTED_EDGE ( 'NONE', *, *, #38774, .T. ) ;
#2913 = CARTESIAN_POINT ( 'NONE',  ( 0.2727639067037610499, 0.000000000000000000, 1.732283464566921172 ) ) ;
#2914 = DIRECTION ( 'NONE',  ( -1.000000000000000000, 0.000000000000000000, 1.734723475976806848E-16 ) ) ;
#2915 = CARTESIAN_POINT ( 'NONE',  ( 0.000000000000000000, 3.346456692913386100, 0.000000000000000000 ) ) ;
#2916 = ORIENTED_EDGE ( 'NONE', *, *, #28214, .T. ) ;
#2917 = CARTESIAN_POINT ( 'NONE',  ( -2.491402175429631605, 1.581999109372839385, -1.585592796919542025 ) ) ;
#2918 = VECTOR ( 'NONE', #6863, 39.37007874015748143 ) ;
#2919 = VERTEX_POINT ( 'NONE', #32470 ) ;
#2920 = CARTESIAN_POINT ( 'NONE',  ( 4.268512490100411402E-16, 0.000000000000000000, 1.889763779527550369 ) ) ;
#2921 = B_SPLINE_CURVE_WITH_KNOTS ( 'NONE', 3,
 ( #18113, #41106, #2617, #33873 ),
 .UNSPECIFIED., .F., .F.,
 ( 4, 4 ),
 ( 2.175031271859537185E-07, 0.01985119632386593558 ),
 .UNSPECIFIED. ) ;
#2922 = VERTEX_POINT ( 'NONE', #48161 ) ;
#2923 = CARTESIAN_POINT ( 'NONE',  ( -1.439733046521776139, 3.267716535433071279, 4.995077429881866871E-16 ) ) ;
#2924 = EDGE_CURVE ( 'NONE', #38926, #9751, #30057, .T. ) ;
#2925 = CARTESIAN_POINT ( 'NONE',  ( -0.2707497483110039016, 1.707396405527592087, -2.459269194452897267 ) ) ;
#2926 = CARTESIAN_POINT ( 'NONE',  ( 0.1968503937007877735, 3.346456692913386100, 2.007874015748021268 ) ) ;
#2927 = CARTESIAN_POINT ( 'NONE',  ( 0.000000000000000000, 3.346456692913386100, 0.000000000000000000 ) ) ;
#2928 = ORIENTED_EDGE ( 'NONE', *, *, #1306, .T. ) ;
#2929 = EDGE_LOOP ( 'NONE', ( #48498, #46715, #10632, #31822 ) ) ;
#2930 = ORIENTED_EDGE ( 'NONE', *, *, #43107, .T. ) ;
#2931 = FACE_OUTER_BOUND ( 'NONE', #46094, .T. ) ;
#2932 = CARTESIAN_POINT ( 'NONE',  ( -0.3486774197067334380, 0.000000000000000000, 1.574803149606291974 ) ) ;
#2933 = ORIENTED_EDGE ( 'NONE', *, *, #23168, .F. ) ;
#2934 = LINE ( 'NONE', #43165, #19836 ) ;
#2935 = DIRECTION ( 'NONE',  ( 1.734723475976806848E-16, -0.000000000000000000, 1.000000000000000000 ) ) ;
#2936 = DIRECTION ( 'NONE',  ( -1.000000000000000000, 0.000000000000000000, 1.734723475976806848E-16 ) ) ;
#2937 = ORIENTED_EDGE ( 'NONE', *, *, #19497, .F. ) ;
#2938 = EDGE_LOOP ( 'NONE', ( #17566, #39632, #24346, #26723 ) ) ;
#2939 = CARTESIAN_POINT ( 'NONE',  ( 0.000000000000000000, 3.267716535433071279, -0.9842519685039348154 ) ) ;
#2940 = PLANE ( 'NONE',  #27436 ) ;
#2941 = FACE_OUTER_BOUND ( 'NONE', #42130, .T. ) ;
#2942 = ORIENTED_EDGE ( 'NONE', *, *, #32110, .T. ) ;
#2943 = CARTESIAN_POINT ( 'NONE',  ( -0.1515599155143076138, 1.705474441417569320, -2.232975473887063966 ) ) ;
#2944 = CARTESIAN_POINT ( 'NONE',  ( 0.000000000000000000, 3.346456692913386100, 0.000000000000000000 ) ) ;
#2945 = VECTOR ( 'NONE', #30142, 39.37007874015748143 ) ;
#2946 = ORIENTED_EDGE ( 'NONE', *, *, #41862, .F. ) ;
#2947 = EDGE_CURVE ( 'NONE', #2091, #45399, #27055, .T. ) ;
#2948 = VECTOR ( 'NONE', #6704, 39.37007874015748143 ) ;
#2949 = DIRECTION ( 'NONE',  ( 1.000000000000000000, -0.000000000000000000, 0.000000000000000000 ) ) ;
#2950 = ORIENTED_EDGE ( 'NONE', *, *, #11989, .F. ) ;
#2951 = ORIENTED_EDGE ( 'NONE', *, *, #41510, .F. ) ;
#2952 = CARTESIAN_POINT ( 'NONE',  ( -3.927031490892378253E-16, 3.346456692913386100, -1.889763779527552146 ) ) ;
#2953 = CARTESIAN_POINT ( 'NONE',  ( 2.996777194923521126, 2.755905511811027164, 0.9139393566314084616 ) ) ;
#2954 = VECTOR ( 'NONE', #26237, 39.37007874015748143 ) ;
#2955 = EDGE_CURVE ( 'NONE', #28023, #10001, #47392, .T. ) ;
#2956 = CARTESIAN_POINT ( 'NONE',  ( 1.091055626815042645, 3.346456692913386100, -0.6299212598425181220 ) ) ;
#2957 = EDGE_CURVE ( 'NONE', #5918, #22349, #11403, .T. ) ;
#2958 = AXIS2_PLACEMENT_3D ( 'NONE', #50068, #46952, #14751 ) ;
#2959 = CARTESIAN_POINT ( 'NONE',  ( 0.000000000000000000, 3.346456692913386100, 0.000000000000000000 ) ) ;
#2960 = EDGE_CURVE ( 'NONE', #29593, #41945, #40210, .T. ) ;
#2961 = CARTESIAN_POINT ( 'NONE',  ( -0.2727639067037602172, 0.000000000000000000, 1.102362204724404160 ) ) ;
#2962 = ORIENTED_EDGE ( 'NONE', *, *, #44917, .T. ) ;
#2963 = VECTOR ( 'NONE', #21923, 39.37007874015748143 ) ;
#2964 = ORIENTED_EDGE ( 'NONE', *, *, #34389, .T. ) ;
#2965 = CARTESIAN_POINT ( 'NONE',  ( -0.07591351300297333182, 3.346456692913386100, -0.4724409448818883694 ) ) ;
#2966 = CARTESIAN_POINT ( 'NONE',  ( 2.106197740627111514, 3.267716535433071279, -0.9842519685039348154 ) ) ;
#2967 = EDGE_CURVE ( 'NONE', #10846, #6843, #27291, .T. ) ;
#2968 = FACE_OUTER_BOUND ( 'NONE', #1001, .T. ) ;
#2969 = FACE_OUTER_BOUND ( 'NONE', #29696, .T. ) ;
#2970 = PLANE ( 'NONE',  #15481 ) ;
#2971 = ORIENTED_EDGE ( 'NONE', *, *, #34380, .T. ) ;
#2972 = LINE ( 'NONE', #2714, #19200 ) ;
#2973 = EDGE_CURVE ( 'NONE', #41852, #6627, #24198, .T. ) ;
#2974 = DIRECTION ( 'NONE',  ( 1.000000000000000000, 0.000000000000000000, 0.000000000000000000 ) ) ;
#2975 = ORIENTED_EDGE ( 'NONE', *, *, #30199, .F. ) ;
#2976 = PLANE ( 'NONE',  #5867 ) ;
#2977 = DIRECTION ( 'NONE',  ( -3.469446951953613696E-16, 0.000000000000000000, -1.000000000000000000 ) ) ;
#2978 = ORIENTED_EDGE ( 'NONE', *, *, #2980, .T. ) ;
#2979 = FACE_OUTER_BOUND ( 'NONE', #5943, .T. ) ;
#2980 = EDGE_CURVE ( 'NONE', #22076, #22611, #4838, .T. ) ;
#2981 = AXIS2_PLACEMENT_3D ( 'NONE', #44162, #20419, #4166 ) ;
#2982 = FACE_OUTER_BOUND ( 'NONE', #9514, .T. ) ;
#2983 = CARTESIAN_POINT ( 'NONE',  ( 0.000000000000000000, 3.267716535433071279, 0.000000000000000000 ) ) ;
#2984 = VECTOR ( 'NONE', #37724, 39.37007874015748143 ) ;
#2985 = VECTOR ( 'NONE', #18006, 39.37007874015748143 ) ;
#2986 = ORIENTED_EDGE ( 'NONE', *, *, #3772, .T. ) ;
#2987 = LINE ( 'NONE', #18735, #15620 ) ;
#2988 = VERTEX_POINT ( 'NONE', #1719 ) ;
#2989 = FACE_BOUND ( 'NONE', #1345, .T. ) ;
#2990 = EDGE_CURVE ( 'NONE', #48375, #11317, #32985, .T. ) ;
#2991 = VECTOR ( 'NONE', #47268, 39.37007874015748143 ) ;
#2992 = CARTESIAN_POINT ( 'NONE',  ( -1.400213059116977909, 1.591076668371641745, -2.010953412639263416 ) ) ;
#2993 = DIRECTION ( 'NONE',  ( 1.000000000000000000, -0.000000000000000000, 0.000000000000000000 ) ) ;
#2994 = AXIS2_PLACEMENT_3D ( 'NONE', #331, #11697, #23564 ) ;
#2995 = VECTOR ( 'NONE', #38127, 39.37007874015748143 ) ;
#2996 = VERTEX_POINT ( 'NONE', #1466 ) ;
#2997 = VERTEX_POINT ( 'NONE', #37615 ) ;
#2998 = DIRECTION ( 'NONE',  ( 1.000000000000000000, -0.000000000000000000, 0.000000000000000000 ) ) ;
#2999 = PLANE ( 'NONE',  #7327 ) ;
#3000 = EDGE_CURVE ( 'NONE', #5416, #8542, #33236, .T. ) ;
#3001 = CARTESIAN_POINT ( 'NONE',  ( 1.225600105435542764, 0.000000000000000000, -1.239880218767107412 ) ) ;
#3002 = CARTESIAN_POINT ( 'NONE',  ( 0.07982360342473591996, 1.709180471932028711, 0.000000000000000000 ) ) ;
#3003 = EDGE_CURVE ( 'NONE', #26865, #9331, #40519, .T. ) ;
#3004 = CARTESIAN_POINT ( 'NONE',  ( 0.000000000000000000, 5.905511811023623991, 0.000000000000000000 ) ) ;
#3005 = ORIENTED_EDGE ( 'NONE', *, *, #39189, .T. ) ;
#3006 = ORIENTED_EDGE ( 'NONE', *, *, #37184, .F. ) ;
#3007 = DIRECTION ( 'NONE',  ( -3.469446951953613696E-16, 0.000000000000000000, -1.000000000000000000 ) ) ;
#3008 = CARTESIAN_POINT ( 'NONE',  ( 2.182111253630085290, 3.346456692913386100, 0.3149606299212573401 ) ) ;
#3009 = ORIENTED_EDGE ( 'NONE', *, *, #8241, .T. ) ;
#3010 = DIRECTION ( 'NONE',  ( -1.000000000000000000, 0.000000000000000000, -0.000000000000000000 ) ) ;
#3011 = ORIENTED_EDGE ( 'NONE', *, *, #41706, .F. ) ;
#3012 = ORIENTED_EDGE ( 'NONE', *, *, #26199, .F. ) ;
#3013 = EDGE_CURVE ( 'NONE', #14432, #17810, #1215, .T. ) ;
#3014 = VECTOR ( 'NONE', #8179, 39.37007874015748143 ) ;
#3015 = EDGE_LOOP ( 'NONE', ( #4364, #35256, #17032, #19002 ) ) ;
#3016 = VERTEX_POINT ( 'NONE', #36847 ) ;
#3017 = LINE ( 'NONE', #3516, #539 ) ;
#3018 = EDGE_CURVE ( 'NONE', #13176, #3567, #41229, .T. ) ;
#3019 = VECTOR ( 'NONE', #7593, 39.37007874015748143 ) ;
#3020 = B_SPLINE_CURVE_WITH_KNOTS ( 'NONE', 3,
 ( #36411, #43623, #31772, #36155 ),
 .UNSPECIFIED., .F., .F.,
 ( 4, 4 ),
 ( 2.271256559101463624E-07, 0.002500295287316845264 ),
 .UNSPECIFIED. ) ;
#3021 = LINE ( 'NONE', #11524, #17188 ) ;
#3022 = DIRECTION ( 'NONE',  ( -3.469446951953613696E-16, 0.000000000000000000, -1.000000000000000000 ) ) ;
#3023 = VECTOR ( 'NONE', #46540, 39.37007874015748143 ) ;
#3024 = LINE ( 'NONE', #22392, #28878 ) ;
#3025 = VECTOR ( 'NONE', #40345, 39.37007874015748143 ) ;
#3026 = FACE_OUTER_BOUND ( 'NONE', #29811, .T. ) ;
#3027 = CARTESIAN_POINT ( 'NONE',  ( 0.002207914879453961969, 5.905511811023623991, 0.04916304461325442243 ) ) ;
#3028 = ORIENTED_EDGE ( 'NONE', *, *, #15970, .T. ) ;
#3029 = CARTESIAN_POINT ( 'NONE',  ( 1.287906020515830141, 3.267716535433071279, -0.9448818897637765168 ) ) ;
#3030 = DIRECTION ( 'NONE',  ( 1.000000000000000000, 0.000000000000000000, 0.000000000000000000 ) ) ;
#3031 = CARTESIAN_POINT ( 'NONE',  ( -0.7030424734358586836, 1.700546966416025096, -2.362433046144440052 ) ) ;
#3032 = CARTESIAN_POINT ( 'NONE',  ( 0.7423782071083087075, 0.000000000000000000, -0.3149606299212593941 ) ) ;
#3033 = VERTEX_POINT ( 'NONE', #9979 ) ;
#3034 = CARTESIAN_POINT ( 'NONE',  ( 1.472219874544872020, 5.905511811023623991, 2.560030851058969770 ) ) ;
#3035 = DIRECTION ( 'NONE',  ( -3.469446951953613696E-16, 0.000000000000000000, -1.000000000000000000 ) ) ;
#3036 = VERTEX_POINT ( 'NONE', #21097 ) ;
#3037 = CARTESIAN_POINT ( 'NONE',  ( -1.001904449526793695, 1.691854617476330036, -1.967052558704270426 ) ) ;
#3038 = ADVANCED_FACE ( 'NONE', ( #9216 ), #5598, .F. ) ;
#3039 = CARTESIAN_POINT ( 'NONE',  ( 0.8182917201112819283, 3.346456692913386100, -0.03937007874015881204 ) ) ;
#3040 = LINE ( 'NONE', #7171, #42231 ) ;
#3041 = EDGE_LOOP ( 'NONE', ( #43908, #38007, #8061, #47649 ) ) ;
#3042 = CARTESIAN_POINT ( 'NONE',  ( -1.977278193622379332, 1.577807025067274882, -0.8986486843887250275 ) ) ;
#3043 = EDGE_CURVE ( 'NONE', #19314, #50260, #45214, .T. ) ;
#3044 = FACE_OUTER_BOUND ( 'NONE', #47672, .T. ) ;
#3045 = CARTESIAN_POINT ( 'NONE',  ( -1.088485032206041980, 1.592042674141829650, 1.917766907668551069 ) ) ;
#3046 = EDGE_CURVE ( 'NONE', #40619, #41687, #48916, .T. ) ;
#3047 = CARTESIAN_POINT ( 'NONE',  ( -2.084291548511494785, -9.441392994058988408E-17, 0.6254821886024599653 ) ) ;
#3048 = DIRECTION ( 'NONE',  ( 0.000000000000000000, 1.000000000000000000, 0.000000000000000000 ) ) ;
#3049 = ORIENTED_EDGE ( 'NONE', *, *, #27749, .F. ) ;
#3050 = EDGE_CURVE ( 'NONE', #26629, #49397, #13857, .T. ) ;
#3051 = CARTESIAN_POINT ( 'NONE',  ( -2.077098083605152024, 1.682859781437124225, 1.719375723742733175 ) ) ;
#3052 = VECTOR ( 'NONE', #32500, 39.37007874015748143 ) ;
#3053 = ORIENTED_EDGE ( 'NONE', *, *, #38808, .F. ) ;
#3054 = ORIENTED_EDGE ( 'NONE', *, *, #37642, .F. ) ;
#3055 = CARTESIAN_POINT ( 'NONE',  ( 2.378961647330872786, 3.267716535433071279, 0.4330708661417287386 ) ) ;
#3056 = ORIENTED_EDGE ( 'NONE', *, *, #3876, .T. ) ;
#3057 = ADVANCED_FACE ( 'NONE', ( #21859 ), #37101, .F. ) ;
#3058 = LINE ( 'NONE', #26296, #38659 ) ;
#3059 = CARTESIAN_POINT ( 'NONE',  ( -1.439733046521777027, 0.000000000000000000, -0.8267716535433052849 ) ) ;
#3060 = EDGE_LOOP ( 'NONE', ( #35581, #1737, #1454, #39950 ) ) ;
#3061 = LINE ( 'NONE', #33557, #6644 ) ;
#3062 = CONICAL_SURFACE ( 'NONE', #12944, 2.244934639244524632, 1.554780866114618743 ) ;
#3063 = DIRECTION ( 'NONE',  ( -0.9998717552508122886, -0.01601477604151185785, 0.000000000000000000 ) ) ;
#3064 = CARTESIAN_POINT ( 'NONE',  ( -0.7697287008956239518, 1.608815407510722606, -2.850711186113256801 ) ) ;
#3065 = VERTEX_POINT ( 'NONE', #25468 ) ;
#3066 = ORIENTED_EDGE ( 'NONE', *, *, #35114, .F. ) ;
#3067 = CARTESIAN_POINT ( 'NONE',  ( 0.000000000000000000, 3.267716535433071279, -0.3149606299212589500 ) ) ;
#3068 = FACE_BOUND ( 'NONE', #5329, .T. ) ;
#3069 = ORIENTED_EDGE ( 'NONE', *, *, #42157, .T. ) ;
#3070 = ADVANCED_FACE ( 'NONE', ( #44819 ), #20837, .F. ) ;
#3071 = PLANE ( 'NONE',  #34462 ) ;
#3072 = ORIENTED_EDGE ( 'NONE', *, *, #45485, .F. ) ;
#3073 = ORIENTED_EDGE ( 'NONE', *, *, #49878, .T. ) ;
#3074 = EDGE_CURVE ( 'NONE', #35684, #49197, #17473, .T. ) ;
#3075 = CARTESIAN_POINT ( 'NONE',  ( 0.1968503937007870241, 0.000000000000000000, -2.204724409448811429 ) ) ;
#3076 = EDGE_CURVE ( 'NONE', #23904, #47505, #46599, .T. ) ;
#3077 = LINE ( 'NONE', #6448, #4797 ) ;
#3078 = VERTEX_POINT ( 'NONE', #17728 ) ;
#3079 = DIRECTION ( 'NONE',  ( -1.000000000000000000, 0.000000000000000000, -0.000000000000000000 ) ) ;
#3080 = ORIENTED_EDGE ( 'NONE', *, *, #39447, .F. ) ;
#3081 = FACE_OUTER_BOUND ( 'NONE', #25459, .T. ) ;
#3082 = CARTESIAN_POINT ( 'NONE',  ( 0.000000000000000000, 3.267716535433071279, 0.000000000000000000 ) ) ;
#3083 = VECTOR ( 'NONE', #15575, 39.37007874015748143 ) ;
#3084 = AXIS2_PLACEMENT_3D ( 'NONE', #32579, #27655, #28165 ) ;
#3085 = CARTESIAN_POINT ( 'NONE',  ( 1.560669927219590747, 3.267716535433071279, -0.7874015748031473194 ) ) ;
#3086 = VERTEX_POINT ( 'NONE', #45072 ) ;
#3087 = ORIENTED_EDGE ( 'NONE', *, *, #6730, .T. ) ;
#3089 = CARTESIAN_POINT ( 'NONE',  ( 2.576863348864709913, 5.905511811023623991, 1.442554885838450041 ) ) ;
#3088 = CIRCLE ( 'NONE', #1434, 2.246510896728926010 ) ;
#3090 = DIRECTION ( 'NONE',  ( -0.01601477604151182663, 0.9998717552508123996, -0.000000000000000000 ) ) ;
#3091 = LINE ( 'NONE', #46674, #25801 ) ;
#3092 = PLANE ( 'NONE',  #28424 ) ;
#3093 = DIRECTION ( 'NONE',  ( 0.000000000000000000, 1.160734090543304660E-16, -1.000000000000000000 ) ) ;
#3094 = CARTESIAN_POINT ( 'NONE',  ( 0.8851946049640924130, 0.02786979497863227920, -1.724702069279120620 ) ) ;
#3095 = CARTESIAN_POINT ( 'NONE',  ( -0.2727639067037611054, 3.346456692913386100, -2.088563196121306476 ) ) ;
#3096 = ORIENTED_EDGE ( 'NONE', *, *, #21228, .F. ) ;
#3097 = DIRECTION ( 'NONE',  ( -0.000000000000000000, 1.000000000000000000, 0.000000000000000000 ) ) ;
#3098 = VECTOR ( 'NONE', #24688, 39.37007874015748143 ) ;
#3099 = ORIENTED_EDGE ( 'NONE', *, *, #48780, .F. ) ;
#3100 = EDGE_LOOP ( 'NONE', ( #662, #12203, #29239, #4476 ) ) ;
#3101 = CARTESIAN_POINT ( 'NONE',  ( 0.6423411368267323285, 0.5233491696640697466, -2.142486692618893684 ) ) ;
#3102 = PLANE ( 'NONE',  #41018 ) ;
#3103 = EDGE_CURVE ( 'NONE', #10488, #3716, #29608, .T. ) ;
#3104 = EDGE_LOOP ( 'NONE', ( #29069, #28174, #40713, #4819 ) ) ;
#3105 = ADVANCED_FACE ( 'NONE', ( #44318 ), #5086, .F. ) ;
#3106 = EDGE_CURVE ( 'NONE', #30941, #13400, #3499, .T. ) ;
#3107 = ORIENTED_EDGE ( 'NONE', *, *, #7943, .F. ) ;
#3108 = CARTESIAN_POINT ( 'NONE',  ( -1.363819533518803473, 3.267716535433071279, 1.850393700787392293 ) ) ;
#3109 = ORIENTED_EDGE ( 'NONE', *, *, #2561, .F. ) ;
#3110 = DIRECTION ( 'NONE',  ( -0.000000000000000000, 0.000000000000000000, 1.000000000000000000 ) ) ;
#3111 = DIRECTION ( 'NONE',  ( 0.000000000000000000, 1.000000000000000000, 0.000000000000000000 ) ) ;
#3112 = AXIS2_PLACEMENT_3D ( 'NONE', #36008, #15857, #27226 ) ;
#3113 = CIRCLE ( 'NONE', #38953, 2.165354330708661568 ) ;
#3114 = VERTEX_POINT ( 'NONE', #2495 ) ;
#3115 = CARTESIAN_POINT ( 'NONE',  ( 2.623503965249849301, 1.661669217907264740, 1.355882097269874187 ) ) ;
#3116 = VERTEX_POINT ( 'NONE', #38618 ) ;
#3117 = VERTEX_POINT ( 'NONE', #11250 ) ;
#3118 = LINE ( 'NONE', #8209, #14111 ) ;
#3119 = DIRECTION ( 'NONE',  ( 0.000000000000000000, 0.000000000000000000, 1.000000000000000000 ) ) ;
#3120 = DIRECTION ( 'NONE',  ( 1.000000000000000000, 0.000000000000000000, 0.000000000000000000 ) ) ;
#3121 = FACE_OUTER_BOUND ( 'NONE', #40793, .T. ) ;
#3122 = VECTOR ( 'NONE', #12651, 39.37007874015748143 ) ;
#3123 = EDGE_CURVE ( 'NONE', #10682, #13031, #19235, .T. ) ;
#3124 = ORIENTED_EDGE ( 'NONE', *, *, #27710, .T. ) ;
#3125 = EDGE_CURVE ( 'NONE', #50633, #39173, #22867, .T. ) ;
#3126 = CARTESIAN_POINT ( 'NONE',  ( 1.363819533518803251, 3.267716535433071279, -0.4724409448818889246 ) ) ;
#3127 = CARTESIAN_POINT ( 'NONE',  ( 0.2646829987306325571, 0.000000000000000000, -2.940868978332396910 ) ) ;
#3128 = LINE ( 'NONE', #18372, #47554 ) ;
#3129 = ORIENTED_EDGE ( 'NONE', *, *, #42959, .T. ) ;
#3130 = EDGE_CURVE ( 'NONE', #13030, #11129, #46580, .T. ) ;
#3131 = CIRCLE ( 'NONE', #28695, 1.743387098533651480 ) ;
#3132 = CARTESIAN_POINT ( 'NONE',  ( 0.000000000000000000, 6.692913385826772199, 0.000000000000000000 ) ) ;
#3133 = EDGE_CURVE ( 'NONE', #15165, #40291, #26259, .T. ) ;
#3134 = ORIENTED_EDGE ( 'NONE', *, *, #37768, .F. ) ;
#3135 = ORIENTED_EDGE ( 'NONE', *, *, #19551, .T. ) ;
#3136 = APPLICATION_PROTOCOL_DEFINITION ( 'draft international standard', 'automotive_design', 1998, #1884 ) ;
#3137 = CONICAL_SURFACE ( 'NONE', #5614, 2.493791675044291445, 0.4363323129985800519 ) ;
#3138 = LINE ( 'NONE', #15011, #21833 ) ;
#3139 = DIRECTION ( 'NONE',  ( -1.000000000000000000, 0.000000000000000000, -0.000000000000000000 ) ) ;
#3140 = CARTESIAN_POINT ( 'NONE',  ( -2.182111253630085290, 3.267716535433071279, 3.785359618865289765E-16 ) ) ;
#3141 = DIRECTION ( 'NONE',  ( -3.469446951953613696E-16, 0.000000000000000000, -1.000000000000000000 ) ) ;
#3142 = EDGE_LOOP ( 'NONE', ( #24679, #26358, #50088, #35426 ) ) ;
#3143 = VERTEX_POINT ( 'NONE', #18491 ) ;
#3144 = CARTESIAN_POINT ( 'NONE',  ( 0.8182917201112819283, 3.346456692913386100, -0.6692913385826764205 ) ) ;
#3145 = CARTESIAN_POINT ( 'NONE',  ( 0.2727639067037604392, 3.346456692913386100, -0.3543307086614173040 ) ) ;
#3146 = ORIENTED_EDGE ( 'NONE', *, *, #38843, .T. ) ;
#3147 = CARTESIAN_POINT ( 'NONE',  ( 0.000000000000000000, 2.755905511811024056, -1.181102362204723200 ) ) ;
#3148 = CARTESIAN_POINT ( 'NONE',  ( 2.020961963619422264, 0.000000000000000000, 0.6739302580930450759 ) ) ;
#3149 = VECTOR ( 'NONE', #15678, 39.37007874015748143 ) ;
#3150 = CARTESIAN_POINT ( 'NONE',  ( -1.735196932040237394, 1.680109596358665636, 1.320828101803479315 ) ) ;
#3151 = CARTESIAN_POINT ( 'NONE',  ( 1.556712866041120247, 1.645058926882370542, 2.509548638715870084 ) ) ;
#3152 = CARTESIAN_POINT ( 'NONE',  ( 0.000000000000000000, 3.267716535433071279, 0.000000000000000000 ) ) ;
#3153 = ORIENTED_EDGE ( 'NONE', *, *, #29643, .T. ) ;
#3154 = CARTESIAN_POINT ( 'NONE',  ( 0.000000000000000000, 3.267716535433071279, -0.9448818897637765168 ) ) ;
#3155 = CARTESIAN_POINT ( 'NONE',  ( -1.088485032206041980, 1.592042674141829650, 1.917766907668551069 ) ) ;
#3156 = VECTOR ( 'NONE', #2196, 39.37007874015748143 ) ;
#3157 = CARTESIAN_POINT ( 'NONE',  ( -1.863748091109392879, 3.346456692913386100, 1.102362204724404160 ) ) ;
#3158 = ORIENTED_EDGE ( 'NONE', *, *, #3617, .F. ) ;
#3160 = CARTESIAN_POINT ( 'NONE',  ( -1.971834065208965203, 0.000000000000000000, 0.8963217522329899323 ) ) ;
#3159 = VECTOR ( 'NONE', #11112, 39.37007874015748143 ) ;
#3161 = DIRECTION ( 'NONE',  ( 1.734723475976806848E-16, 0.000000000000000000, 1.000000000000000000 ) ) ;
#3162 = DIRECTION ( 'NONE',  ( 0.000000000000000000, 0.000000000000000000, 1.000000000000000000 ) ) ;
#3163 = ORIENTED_EDGE ( 'NONE', *, *, #16884, .F. ) ;
#3164 = AXIS2_PLACEMENT_3D ( 'NONE', #16738, #39971, #12348 ) ;
#3165 = CARTESIAN_POINT ( 'NONE',  ( 1.905060681038603487, -1.256585629014249294E-16, 1.081042454612135106 ) ) ;
#3166 = ADVANCED_FACE ( 'NONE', ( #49432 ), #34246, .T. ) ;
#3167 = EDGE_CURVE ( 'NONE', #22305, #31088, #14871, .T. ) ;
#3168 = ORIENTED_EDGE ( 'NONE', *, *, #10013, .T. ) ;
#3169 = DIRECTION ( 'NONE',  ( -1.000000000000000000, 0.000000000000000000, 0.000000000000000000 ) ) ;
#3170 = ORIENTED_EDGE ( 'NONE', *, *, #32471, .F. ) ;
#3171 = AXIS2_PLACEMENT_3D ( 'NONE', #21586, #1707, #41214 ) ;
#3172 = CARTESIAN_POINT ( 'NONE',  ( -1.236813753895212642, 1.541669022091038732, -2.681693691597581974 ) ) ;
#3173 = EDGE_CURVE ( 'NONE', #14116, #12624, #35575, .T. ) ;
#3174 = ORIENTED_EDGE ( 'NONE', *, *, #38464, .F. ) ;
#3175 = CARTESIAN_POINT ( 'NONE',  ( 1.312623452344844566, 0.000000000000000000, 1.722945714930923744 ) ) ;
#3176 = LINE ( 'NONE', #34178, #808 ) ;
#3177 = LINE ( 'NONE', #30799, #1292 ) ;
#3178 = EDGE_LOOP ( 'NONE', ( #19252, #27222, #23843, #48316 ) ) ;
#3179 = VERTEX_POINT ( 'NONE', #2740 ) ;
#3180 = VERTEX_POINT ( 'NONE', #49932 ) ;
#3181 = CARTESIAN_POINT ( 'NONE',  ( -1.053808008129011320, 3.267716535433071279, 2.204724409448808764 ) ) ;
#3182 = CARTESIAN_POINT ( 'NONE',  ( 0.000000000000000000, 3.346456692913386100, -2.493791675044291445 ) ) ;
#3183 = ORIENTED_EDGE ( 'NONE', *, *, #22189, .F. ) ;
#3184 = DIRECTION ( 'NONE',  ( 1.734723475976806848E-16, 0.000000000000000000, 1.000000000000000000 ) ) ;
#3185 = CARTESIAN_POINT ( 'NONE',  ( 1.363819533518803251, 3.346456692913386100, 1.417322834645662777 ) ) ;
#3186 = CARTESIAN_POINT ( 'NONE',  ( -2.548348758378718326, 1.050013800432074706, -0.06518427251839807590 ) ) ;
#3187 = ORIENTED_EDGE ( 'NONE', *, *, #41641, .T. ) ;
#3188 = ORIENTED_EDGE ( 'NONE', *, *, #14731, .F. ) ;
#3189 = ADVANCED_FACE ( 'NONE', ( #6870 ), #42730, .F. ) ;
#3190 = LINE ( 'NONE', #26929, #18061 ) ;
#3191 = LINE ( 'NONE', #50375, #24172 ) ;
#3192 = AXIS2_PLACEMENT_3D ( 'NONE', #31897, #12262, #43737 ) ;
#3193 = DIRECTION ( 'NONE',  ( -0.8584487936018655452, 0.000000000000000000, -0.5128992774059071280 ) ) ;
#3194 = EDGE_LOOP ( 'NONE', ( #4997, #14927, #17748, #13431 ) ) ;
#3195 = DIRECTION ( 'NONE',  ( 1.734723475976806848E-16, -0.000000000000000000, 1.000000000000000000 ) ) ;
#3196 = DIRECTION ( 'NONE',  ( -0.000000000000000000, 1.000000000000000000, -0.000000000000000000 ) ) ;
#3197 = ORIENTED_EDGE ( 'NONE', *, *, #35942, .T. ) ;
#3198 = EDGE_CURVE ( 'NONE', #45979, #19989, #23215, .T. ) ;
#3199 = FACE_OUTER_BOUND ( 'NONE', #6239, .T. ) ;
#3200 = VERTEX_POINT ( 'NONE', #23116 ) ;
#3201 = EDGE_LOOP ( 'NONE', ( #15679, #26156, #28563, #16403 ) ) ;
#3202 = CARTESIAN_POINT ( 'NONE',  ( 1.636583440222563857, 0.000000000000000000, -0.3149606299212596716 ) ) ;
#3203 = CARTESIAN_POINT ( 'NONE',  ( 0.5272349255864849926, 0.000000000000000000, 2.905303903342417726 ) ) ;
#3204 = AXIS2_PLACEMENT_3D ( 'NONE', #38568, #10938, #31068 ) ;
#3205 = CIRCLE ( 'NONE', #11416, 2.165354330708661568 ) ;
#3206 = DIRECTION ( 'NONE',  ( 1.734723475976806848E-16, -0.000000000000000000, 1.000000000000000000 ) ) ;
#3207 = CARTESIAN_POINT ( 'NONE',  ( -0.1824162227212925702, 1.021972889971727971, -2.575817126301924720 ) ) ;
#3208 = DIRECTION ( 'NONE',  ( -0.000000000000000000, 1.000000000000000000, -0.000000000000000000 ) ) ;
#3209 = VERTEX_POINT ( 'NONE', #42225 ) ;
#3210 = CONICAL_SURFACE ( 'NONE', #46087, 1.850107469027523210, 0.6386652850508578450 ) ;
#3211 = ORIENTED_EDGE ( 'NONE', *, *, #15642, .F. ) ;
#3212 = CARTESIAN_POINT ( 'NONE',  ( 0.7423782071083087075, 0.000000000000000000, 0.3149606299212576177 ) ) ;
#3213 = LINE ( 'NONE', #15092, #6963 ) ;
#3214 = CARTESIAN_POINT ( 'NONE',  ( 0.07982360342473591996, 1.709180471932028711, 0.000000000000000000 ) ) ;
#3215 = FACE_OUTER_BOUND ( 'NONE', #8236, .T. ) ;
#3216 = EDGE_LOOP ( 'NONE', ( #43220, #10851, #17471, #40232, #47933, #5909, #8649, #32382, #28969, #29769, #45034 ) ) ;
#3217 = CARTESIAN_POINT ( 'NONE',  ( 0.1968503937007878568, 0.000000000000000000, 1.889763779527550369 ) ) ;
#3218 = LINE ( 'NONE', #39096, #4223 ) ;
#3219 = ORIENTED_EDGE ( 'NONE', *, *, #8414, .T. ) ;
#3220 = LINE ( 'NONE', #22097, #38051 ) ;
#3221 = DIRECTION ( 'NONE',  ( 1.000000000000000000, -0.000000000000000000, 0.000000000000000000 ) ) ;
#3222 = PLANE ( 'NONE',  #38669 ) ;
#3223 = AXIS2_PLACEMENT_3D ( 'NONE', #15563, #39306, #35439 ) ;
#3224 = B_SPLINE_CURVE_WITH_KNOTS ( 'NONE', 3,
 ( #34791, #19030, #27279, #26526 ),
 .UNSPECIFIED., .F., .F.,
 ( 4, 4 ),
 ( 0.001786984533467655609, 0.004287017325207927165 ),
 .UNSPECIFIED. ) ;
#3225 = CARTESIAN_POINT ( 'NONE',  ( 0.000000000000000000, 3.267716535433071279, -0.6299212598425181220 ) ) ;
#3226 = CARTESIAN_POINT ( 'NONE',  ( -1.091055626815042645, 0.000000000000000000, -1.574803149606293529 ) ) ;
#3227 = CARTESIAN_POINT ( 'NONE',  ( 1.363819533518803251, 3.346456692913386100, 0.4724409448818871482 ) ) ;
#3228 = EDGE_CURVE ( 'NONE', #47957, #869, #10741, .T. ) ;
#3229 = EDGE_CURVE ( 'NONE', #46970, #23957, #46085, .T. ) ;
#3230 = ORIENTED_EDGE ( 'NONE', *, *, #47814, .F. ) ;
#3231 = FACE_OUTER_BOUND ( 'NONE', #20858, .T. ) ;
#3232 = ORIENTED_EDGE ( 'NONE', *, *, #48206, .T. ) ;
#3233 = FACE_BOUND ( 'NONE', #24083, .T. ) ;
#3234 = ADVANCED_FACE ( 'NONE', ( #25982 ), #2999, .F. ) ;
#3235 = VECTOR ( 'NONE', #50891, 39.37007874015748143 ) ;
#3236 = DIRECTION ( 'NONE',  ( -0.000000000000000000, -1.000000000000000000, -0.000000000000000000 ) ) ;
#3238 = ADVANCED_FACE ( 'NONE', ( #33994 ), #45829, .F. ) ;
#3237 = DIRECTION ( 'NONE',  ( 1.734723475976806848E-16, -0.000000000000000000, 1.000000000000000000 ) ) ;
#3239 = EDGE_CURVE ( 'NONE', #33931, #46747, #26235, .T. ) ;
#3240 = AXIS2_PLACEMENT_3D ( 'NONE', #39108, #6611, #14862 ) ;
#3241 = EDGE_LOOP ( 'NONE', ( #4466, #3607, #39192, #8451, #33437, #10241, #41815, #15004, #38481, #19779, #50318 ) ) ;
#3242 = VERTEX_POINT ( 'NONE', #38124 ) ;
#3243 = CYLINDRICAL_SURFACE ( 'NONE', #9213, 2.164630168518208109 ) ;
#3244 = CARTESIAN_POINT ( 'NONE',  ( -1.091055626815042201, 0.000000000000000000, 1.062992125984246083 ) ) ;
#3245 = DIRECTION ( 'NONE',  ( 1.000000000000000000, 0.000000000000000000, 0.000000000000000000 ) ) ;
#3246 = DIRECTION ( 'NONE',  ( -1.000000000000000000, 0.000000000000000000, -0.000000000000000000 ) ) ;
#3247 = VECTOR ( 'NONE', #34664, 39.37007874015748143 ) ;
#3248 = LINE ( 'NONE', #35000, #18658 ) ;
#3249 = B_SPLINE_CURVE_WITH_KNOTS ( 'NONE', 3,
 ( #11330, #50265, #7211, #27571 ),
 .UNSPECIFIED., .F., .F.,
 ( 4, 4 ),
 ( 7.244828104690220634E-07, 0.005111537570788880769 ),
 .UNSPECIFIED. ) ;
#3250 = DIRECTION ( 'NONE',  ( -0.000000000000000000, 1.000000000000000000, -0.000000000000000000 ) ) ;
#3251 = ORIENTED_EDGE ( 'NONE', *, *, #1563, .F. ) ;
#3252 = EDGE_CURVE ( 'NONE', #49628, #11104, #7623, .T. ) ;
#3253 = VERTEX_POINT ( 'NONE', #12003 ) ;
#3254 = FACE_OUTER_BOUND ( 'NONE', #46091, .T. ) ;
#3255 = DIRECTION ( 'NONE',  ( -1.000000000000000000, 0.000000000000000000, 0.000000000000000000 ) ) ;
#3256 = VERTEX_POINT ( 'NONE', #31629 ) ;
#3257 = EDGE_CURVE ( 'NONE', #47679, #37198, #8131, .T. ) ;
#3258 = CARTESIAN_POINT ( 'NONE',  ( -1.051609096396380005, 0.4349011127721510994, 1.025452293874513199 ) ) ;
#3259 = VERTEX_POINT ( 'NONE', #27232 ) ;
#3260 = VERTEX_POINT ( 'NONE', #43227 ) ;
#3261 = VECTOR ( 'NONE', #44884, 39.37007874015748143 ) ;
#3262 = EDGE_CURVE ( 'NONE', #11733, #6435, #11501, .T. ) ;
#3263 = ORIENTED_EDGE ( 'NONE', *, *, #41239, .F. ) ;
#3264 = ORIENTED_EDGE ( 'NONE', *, *, #18392, .F. ) ;
#3265 = PLANE ( 'NONE',  #502 ) ;
#3266 = B_SPLINE_CURVE_WITH_KNOTS ( 'NONE', 3,
 ( #41625, #14762, #18639, #1867 ),
 .UNSPECIFIED., .F., .F.,
 ( 4, 4 ),
 ( 0.01307398419200031005, 0.03074127892600248685 ),
 .UNSPECIFIED. ) ;
#3267 = B_SPLINE_CURVE_WITH_KNOTS ( 'NONE', 3,
 ( #4982, #44968, #9626, #25366 ),
 .UNSPECIFIED., .F., .F.,
 ( 4, 4 ),
 ( 2.656727046556617721E-07, 0.01658836988290275996 ),
 .UNSPECIFIED. ) ;
#3268 = CARTESIAN_POINT ( 'NONE',  ( 1.363819533518803251, 0.000000000000000000, 1.220472440944875281 ) ) ;
#3269 = EDGE_CURVE ( 'NONE', #18410, #37571, #7874, .T. ) ;
#3270 = CARTESIAN_POINT ( 'NONE',  ( 0.000000000000000000, 3.267716535433071279, -0.7874015748031470974 ) ) ;
#3271 = CIRCLE ( 'NONE', #51004, 2.246510896728926010 ) ;
#3272 = CARTESIAN_POINT ( 'NONE',  ( 0.1968503937007872462, 3.267716535433071279, -0.5118110236220465570 ) ) ;
#3273 = DIRECTION ( 'NONE',  ( 0.000000000000000000, 1.000000000000000000, 0.000000000000000000 ) ) ;
#3274 = CARTESIAN_POINT ( 'NONE',  ( 0.3941266864751867272, 0.01134630888347559936, 1.896204066697775970 ) ) ;
#3275 = ORIENTED_EDGE ( 'NONE', *, *, #42395, .T. ) ;
#3276 = DIRECTION ( 'NONE',  ( 0.000000000000000000, 1.160734090543304660E-16, -1.000000000000000000 ) ) ;
#3277 = CARTESIAN_POINT ( 'NONE',  ( 0.2727639067037604947, 3.346456692913386100, -1.102362204724405714 ) ) ;
#3278 = AXIS2_PLACEMENT_3D ( 'NONE', #49300, #3111, #49797 ) ;
#3279 = CARTESIAN_POINT ( 'NONE',  ( -0.8182917201112814842, 3.267716535433071279, 0.9055118110236167750 ) ) ;
#3280 = DIRECTION ( 'NONE',  ( 1.734723475976806848E-16, 0.000000000000000000, 1.000000000000000000 ) ) ;
#3281 = EDGE_LOOP ( 'NONE', ( #24899, #13152, #5466, #50344 ) ) ;
#3282 = CARTESIAN_POINT ( 'NONE',  ( -3.073077335812187894, 2.755905511811027164, 0.6509316561051810002 ) ) ;
#3283 = CARTESIAN_POINT ( 'NONE',  ( -2.182111253630085290, 0.000000000000000000, 0.4330708661417290162 ) ) ;
#3284 = ORIENTED_EDGE ( 'NONE', *, *, #4359, .F. ) ;
#3285 = DIRECTION ( 'NONE',  ( -9.390536051998861478E-17, -1.000000000000000000, 6.822623802544654332E-17 ) ) ;
#3286 = DIRECTION ( 'NONE',  ( 0.000000000000000000, -1.000000000000000000, -0.000000000000000000 ) ) ;
#3287 = LINE ( 'NONE', #10782, #11717 ) ;
#3288 = ORIENTED_EDGE ( 'NONE', *, *, #20336, .F. ) ;
#3289 = CARTESIAN_POINT ( 'NONE',  ( -1.363819533518803473, 3.267716535433071279, 1.732283464566920950 ) ) ;
#3290 = EDGE_CURVE ( 'NONE', #24851, #9179, #30639, .T. ) ;
#3291 = CARTESIAN_POINT ( 'NONE',  ( 1.629109206296508017, 1.701186718475893533, -1.625674421363809907 ) ) ;
#3292 = LINE ( 'NONE', #22166, #10569 ) ;
#3293 = CARTESIAN_POINT ( 'NONE',  ( 2.695799277629594037, 1.761268146152256575, -1.205759334241453651 ) ) ;
#3295 = EDGE_CURVE ( 'NONE', #43929, #43549, #35752, .T. ) ;
#3294 = LINE ( 'NONE', #39427, #2883 ) ;
#3296 = AXIS2_PLACEMENT_3D ( 'NONE', #40923, #37052, #25671 ) ;
#3297 = ORIENTED_EDGE ( 'NONE', *, *, #4382, .F. ) ;
#3298 = EDGE_CURVE ( 'NONE', #40227, #35873, #39370, .T. ) ;
#3299 = DIRECTION ( 'NONE',  ( 1.000000000000000000, 0.000000000000000000, 0.000000000000000000 ) ) ;
#3300 = VERTEX_POINT ( 'NONE', #47069 ) ;
#3301 = ORIENTED_EDGE ( 'NONE', *, *, #35809, .F. ) ;
#3302 = CARTESIAN_POINT ( 'NONE',  ( -1.648912428261716023, 0.001020809608550144430, 0.5875093135061575378 ) ) ;
#3303 = ORIENTED_EDGE ( 'NONE', *, *, #30368, .F. ) ;
#3304 = CARTESIAN_POINT ( 'NONE',  ( 2.009930929872536964, 1.574803149606302854, -0.8055662819783826478 ) ) ;
#3305 = LINE ( 'NONE', #19047, #479 ) ;
#3306 = ORIENTED_EDGE ( 'NONE', *, *, #7095, .F. ) ;
#3307 = VECTOR ( 'NONE', #48691, 39.37007874015748143 ) ;
#3308 = CARTESIAN_POINT ( 'NONE',  ( 2.685986181519757210, 2.755905511811027164, -1.228718213908074119 ) ) ;
#3309 = AXIS2_PLACEMENT_3D ( 'NONE', #31850, #340, #11460 ) ;
#3310 = LINE ( 'NONE', #19052, #24950 ) ;
#3311 = CARTESIAN_POINT ( 'NONE',  ( 0.4349608091550764555, 1.574803149606302854, 2.121218629000301004 ) ) ;
#3312 = ORIENTED_EDGE ( 'NONE', *, *, #30981, .T. ) ;
#3313 = ORIENTED_EDGE ( 'NONE', *, *, #17274, .T. ) ;
#3314 = DIRECTION ( 'NONE',  ( -0.9909497617679332571, 0.000000000000000000, -0.1342332658176667304 ) ) ;
#3315 = FACE_BOUND ( 'NONE', #49368, .T. ) ;
#3316 = EDGE_LOOP ( 'NONE', ( #44463, #23044, #2855, #2192 ) ) ;
#3317 = VECTOR ( 'NONE', #47653, 39.37007874015748143 ) ;
#3318 = CARTESIAN_POINT ( 'NONE',  ( 0.7423782071083087075, 3.267716535433071279, -0.6299212598425181220 ) ) ;
#3319 = B_SPLINE_CURVE_WITH_KNOTS ( 'NONE', 3,
 ( #43400, #558, #3664, #34910 ),
 .UNSPECIFIED., .F., .F.,
 ( 4, 4 ),
 ( 5.924731125040265931E-05, 0.05030560113089571628 ),
 .UNSPECIFIED. ) ;
#3320 = ADVANCED_FACE ( 'NONE', ( #19739 ), #27901, .T. ) ;
#3321 = ORIENTED_EDGE ( 'NONE', *, *, #45459, .F. ) ;
#3322 = VERTEX_POINT ( 'NONE', #382 ) ;
#3323 = CARTESIAN_POINT ( 'NONE',  ( -0.5859249214279436124, 1.049866565067837820, -1.938067127089992070 ) ) ;
#3324 = DIRECTION ( 'NONE',  ( 8.881784197001252323E-16, 0.000000000000000000, 1.000000000000000000 ) ) ;
#3325 = EDGE_LOOP ( 'NONE', ( #27783, #36487, #10237, #666 ) ) ;
#3326 = CARTESIAN_POINT ( 'NONE',  ( 0.000000000000000000, 1.574803149606302854, 0.000000000000000000 ) ) ;
#3327 = EDGE_CURVE ( 'NONE', #44522, #9751, #7231, .T. ) ;
#3328 = ORIENTED_EDGE ( 'NONE', *, *, #42838, .T. ) ;
#3329 = CARTESIAN_POINT ( 'NONE',  ( 2.947574761915768171, 1.205361022782829114E-17, -0.1816379373804913322 ) ) ;
#3330 = PLANE ( 'NONE',  #30772 ) ;
#3331 = ADVANCED_FACE ( 'NONE', ( #32150 ), #35501, .F. ) ;
#3332 = LINE ( 'NONE', #34339, #33001 ) ;
#3333 = ORIENTED_EDGE ( 'NONE', *, *, #37981, .F. ) ;
#3334 = ORIENTED_EDGE ( 'NONE', *, *, #23127, .F. ) ;
#3335 = CARTESIAN_POINT ( 'NONE',  ( -2.139229417893219853, 1.205361022782829114E-17, -0.3394403656973710159 ) ) ;
#3336 = DIRECTION ( 'NONE',  ( 0.000000000000000000, 1.000000000000000000, 0.000000000000000000 ) ) ;
#3337 = CARTESIAN_POINT ( 'NONE',  ( -2.543969358050849117, 1.049938081865076756, -0.1635119977925399981 ) ) ;
#3338 = ADVANCED_FACE ( 'NONE', ( #50928 ), #8388, .T. ) ;
#3339 = CARTESIAN_POINT ( 'NONE',  ( 1.287906020515829919, 3.267716535433071279, -2.076684646723067296 ) ) ;
#3340 = EDGE_CURVE ( 'NONE', #46657, #25764, #40149, .T. ) ;
#3341 = PLANE ( 'NONE',  #28912 ) ;
#3342 = VECTOR ( 'NONE', #4674, 39.37007874015748143 ) ;
#3343 = AXIS2_PLACEMENT_3D ( 'NONE', #15060, #38561, #23059 ) ;
#3344 = CARTESIAN_POINT ( 'NONE',  ( 1.398572223930554026, 1.205361022782829114E-17, 1.525996566212370231 ) ) ;
#3345 = CARTESIAN_POINT ( 'NONE',  ( 0.5455278134075211005, 3.346456692913386100, -0.1968503937007880511 ) ) ;
#3346 = ORIENTED_EDGE ( 'NONE', *, *, #30233, .F. ) ;
#3347 = CARTESIAN_POINT ( 'NONE',  ( -0.07591351300297333182, 0.000000000000000000, -0.1574803149606301411 ) ) ;
#3348 = CARTESIAN_POINT ( 'NONE',  ( -0.2156685157583833057, 1.520013147563287648, -2.945280361644576850 ) ) ;
#3349 = VECTOR ( 'NONE', #36535, 39.37007874015748143 ) ;
#3350 = ORIENTED_EDGE ( 'NONE', *, *, #14027, .F. ) ;
#3352 = ADVANCED_FACE ( 'NONE', ( #28249 ), #40308, .F. ) ;
#3351 = VERTEX_POINT ( 'NONE', #12512 ) ;
#3353 = CARTESIAN_POINT ( 'NONE',  ( -0.8942052331142547050, 3.267716535433071279, 1.377952755905504256 ) ) ;
#3354 = CARTESIAN_POINT ( 'NONE',  ( 0.9914495361338625523, 1.734714548371065312, 2.781765111341823360 ) ) ;
#3355 =( BOUNDED_CURVE ( )  B_SPLINE_CURVE ( 3, ( #14492, #22745, #4329, #35829 ),
 .UNSPECIFIED., .F., .F. ) 
 B_SPLINE_CURVE_WITH_KNOTS ( ( 4, 4 ),
 ( 1.825764642043493646, 1.876704608224056381 ),
 .UNSPECIFIED. ) 
 CURVE ( )  GEOMETRIC_REPRESENTATION_ITEM ( )  RATIONAL_B_SPLINE_CURVE ( ( 1.000000000000000000, 0.9997837716768099847, 0.9997837716768099847, 1.000000000000000000 ) ) 
 REPRESENTATION_ITEM ( '' )  );
#3356 = ORIENTED_EDGE ( 'NONE', *, *, #3900, .T. ) ;
#3357 = EDGE_CURVE ( 'NONE', #17408, #38652, #22684, .T. ) ;
#3358 = EDGE_CURVE ( 'NONE', #21585, #25120, #31376, .T. ) ;
#3359 = LINE ( 'NONE', #51045, #26267 ) ;
#3360 = EDGE_CURVE ( 'NONE', #47112, #12259, #50674, .T. ) ;
#3361 = VERTEX_POINT ( 'NONE', #40910 ) ;
#3362 = CARTESIAN_POINT ( 'NONE',  ( -1.097585813245683273, 0.000000000000000000, -0.9794755770252108196 ) ) ;
#3363 = ORIENTED_EDGE ( 'NONE', *, *, #13778, .F. ) ;
#3364 = CARTESIAN_POINT ( 'NONE',  ( 2.312113436335841321, 1.646509482104762334, 0.2635349935491774209 ) ) ;
#3365 = LINE ( 'NONE', #34616, #14011 ) ;
#3366 = ORIENTED_EDGE ( 'NONE', *, *, #41324, .F. ) ;
#3367 = DIRECTION ( 'NONE',  ( -0.9998717552508121775, -0.01601477604151185438, 0.000000000000000000 ) ) ;
#3368 = ORIENTED_EDGE ( 'NONE', *, *, #23732, .T. ) ;
#3369 = ORIENTED_EDGE ( 'NONE', *, *, #49867, .F. ) ;
#3370 = DIRECTION ( 'NONE',  ( -1.000000000000000000, -0.000000000000000000, -0.000000000000000000 ) ) ;
#3371 = CARTESIAN_POINT ( 'NONE',  ( 0.4696143004045476577, 3.346456692913386100, -2.113816876263008293 ) ) ;
#3372 = DIRECTION ( 'NONE',  ( -0.000000000000000000, -1.000000000000000000, -0.000000000000000000 ) ) ;
#3373 = AXIS2_PLACEMENT_3D ( 'NONE', #21134, #2270, #18018 ) ;
#3374 = ORIENTED_EDGE ( 'NONE', *, *, #7664, .F. ) ;
#3375 = AXIS2_PLACEMENT_3D ( 'NONE', #24468, #40218, #36342 ) ;
#3376 = LINE ( 'NONE', #27116, #23718 ) ;
#3377 = DIRECTION ( 'NONE',  ( -3.986037398843765983E-20, -1.000000000000000000, -1.160734090543304660E-16 ) ) ;
#3378 = ADVANCED_FACE ( 'NONE', ( #5536 ), #12777, .F. ) ;
#3379 = VERTEX_POINT ( 'NONE', #36781 ) ;
#3380 = LINE ( 'NONE', #19121, #12555 ) ;
#3381 = ORIENTED_EDGE ( 'NONE', *, *, #22347, .T. ) ;
#3382 = ORIENTED_EDGE ( 'NONE', *, *, #7527, .T. ) ;
#3383 = CIRCLE ( 'NONE', #32223, 2.165354330708661568 ) ;
#3384 = DIRECTION ( 'NONE',  ( 0.8184814127304661513, -0.2728986718806660772, 0.5055833184555332815 ) ) ;
#3385 = EDGE_CURVE ( 'NONE', #31518, #29992, #9154, .T. ) ;
#3386 = ORIENTED_EDGE ( 'NONE', *, *, #32466, .F. ) ;
#3387 = CARTESIAN_POINT ( 'NONE',  ( -1.181102362204724310, 0.4724409448818890911, -1.062992125984252079 ) ) ;
#3388 = VECTOR ( 'NONE', #10526, 39.37007874015748143 ) ;
#3389 = FACE_OUTER_BOUND ( 'NONE', #42721, .T. ) ;
#3390 = ADVANCED_FACE ( 'NONE', ( #20770 ), #9413, .F. ) ;
#3391 = EDGE_CURVE ( 'NONE', #15612, #22693, #28507, .T. ) ;
#3392 = CARTESIAN_POINT ( 'NONE',  ( -2.047329853004924427, 1.609493418792719233, 0.7169629821276162218 ) ) ;
#3393 = LINE ( 'NONE', #11644, #48565 ) ;
#3394 = ORIENTED_EDGE ( 'NONE', *, *, #38672, .T. ) ;
#3396 = EDGE_CURVE ( 'NONE', #45413, #1213, #1659, .T. ) ;
#3395 = VERTEX_POINT ( 'NONE', #29280 ) ;
#3397 = CARTESIAN_POINT ( 'NONE',  ( -0.2156685157583831947, 1.617455082123532062, -2.945280361644576850 ) ) ;
#3398 = DIRECTION ( 'NONE',  ( -0.000000000000000000, 1.000000000000000000, -0.000000000000000000 ) ) ;
#3399 = EDGE_LOOP ( 'NONE', ( #29587, #39428, #39387, #24580 ) ) ;
#3400 = DIRECTION ( 'NONE',  ( -3.981026654148454344E-17, 1.000000000000000000, -1.225234019452869602E-16 ) ) ;
#3401 = CARTESIAN_POINT ( 'NONE',  ( 2.867773316779195447, 2.755905511811027164, -0.7050287376752003565 ) ) ;
#3402 = EDGE_CURVE ( 'NONE', #22349, #41895, #25662, .T. ) ;
#3403 = LINE ( 'NONE', #283, #4457 ) ;
#3404 = CARTESIAN_POINT ( 'NONE',  ( -0.5443978225238782498, 1.600757226547528500, -2.157565353623420723 ) ) ;
#3405 = DIRECTION ( 'NONE',  ( 1.734723475976806848E-16, -0.000000000000000000, 1.000000000000000000 ) ) ;
#3406 = VERTEX_POINT ( 'NONE', #25157 ) ;
#3407 = LINE ( 'NONE', #50586, #38273 ) ;
#3408 =( NAMED_UNIT ( * ) PLANE_ANGLE_UNIT ( ) SI_UNIT ( $, .RADIAN. ) );
#3409 = ADVANCED_FACE ( 'NONE', ( #45014 ), #1407, .F. ) ;
#3410 = VECTOR ( 'NONE', #26959, 39.37007874015748143 ) ;
#3411 = ORIENTED_EDGE ( 'NONE', *, *, #10906, .F. ) ;
#3412 = CARTESIAN_POINT ( 'NONE',  ( -1.166969139818015533, 0.000000000000000000, 0.7874015748031456541 ) ) ;
#3413 = EDGE_CURVE ( 'NONE', #26317, #49645, #13288, .T. ) ;
#3414 = AXIS2_PLACEMENT_3D ( 'NONE', #46093, #10748, #26488 ) ;
#3415 = DIRECTION ( 'NONE',  ( -3.469446951953613696E-16, 0.000000000000000000, -1.000000000000000000 ) ) ;
#3416 = FACE_OUTER_BOUND ( 'NONE', #36091, .T. ) ;
#3417 = EDGE_LOOP ( 'NONE', ( #1170, #50567, #20684, #22013 ) ) ;
#3418 = EDGE_CURVE ( 'NONE', #4264, #31838, #33173, .T. ) ;
#3419 = FACE_OUTER_BOUND ( 'NONE', #50236, .T. ) ;
#3420 = AXIS2_PLACEMENT_3D ( 'NONE', #28248, #12776, #39369 ) ;
#3421 = ADVANCED_FACE ( 'NONE', ( #21287 ), #37041, .F. ) ;
#3422 = ORIENTED_EDGE ( 'NONE', *, *, #35506, .T. ) ;
#3423 = DIRECTION ( 'NONE',  ( -0.01601477604151182663, 0.9998717552508123996, -0.000000000000000000 ) ) ;
#3424 = VECTOR ( 'NONE', #10867, 39.37007874015748143 ) ;
#3425 = VERTEX_POINT ( 'NONE', #24902 ) ;
#3426 = LINE ( 'NONE', #29404, #34492 ) ;
#3427 = VERTEX_POINT ( 'NONE', #21536 ) ;
#3428 = VECTOR ( 'NONE', #16887, 39.37007874015748143 ) ;
#3429 = CARTESIAN_POINT ( 'NONE',  ( -1.293618082698012151, 0.000000000000000000, -1.168738992012460898 ) ) ;
#3430 = CARTESIAN_POINT ( 'NONE',  ( -1.909347346926324462, 0.000000000000000000, 1.102362204724404160 ) ) ;
#3431 = CARTESIAN_POINT ( 'NONE',  ( -2.947574761915765063, 0.000000000000000000, -0.1816379373805331598 ) ) ;
#3432 = ORIENTED_EDGE ( 'NONE', *, *, #50034, .F. ) ;
#3433 = ORIENTED_EDGE ( 'NONE', *, *, #46228, .F. ) ;
#3434 = ORIENTED_EDGE ( 'NONE', *, *, #33399, .F. ) ;
#3435 = DIRECTION ( 'NONE',  ( -1.000000000000000000, 0.000000000000000000, 0.000000000000000000 ) ) ;
#3436 = CARTESIAN_POINT ( 'NONE',  ( 1.312248418042879727, 1.574803149606302854, -1.722429524498089393 ) ) ;
#3437 = ORIENTED_EDGE ( 'NONE', *, *, #19119, .F. ) ;
#3438 = ORIENTED_EDGE ( 'NONE', *, *, #44602, .T. ) ;
#3439 = LINE ( 'NONE', #22810, #25603 ) ;
#3440 = CARTESIAN_POINT ( 'NONE',  ( -0.8182917201112819283, 3.346456692913386100, -0.3543307086614175816 ) ) ;
#3441 = DIRECTION ( 'NONE',  ( 1.734723475976806848E-16, -0.000000000000000000, 1.000000000000000000 ) ) ;
#3442 = ORIENTED_EDGE ( 'NONE', *, *, #8413, .T. ) ;
#3443 = ORIENTED_EDGE ( 'NONE', *, *, #35989, .F. ) ;
#3444 = DIRECTION ( 'NONE',  ( -0.000000000000000000, 1.000000000000000000, -0.000000000000000000 ) ) ;
#3445 = CARTESIAN_POINT ( 'NONE',  ( 2.222091332265985208, 1.743492810207595500, 0.6702560524809636489 ) ) ;
#3446 = LINE ( 'NONE', #26182, #46136 ) ;
#3447 = ORIENTED_EDGE ( 'NONE', *, *, #24272, .F. ) ;
#3448 = DIRECTION ( 'NONE',  ( -0.9998717552508122886, -0.01601477604151180928, 0.000000000000000000 ) ) ;
#3449 = ORIENTED_EDGE ( 'NONE', *, *, #29863, .T. ) ;
#3450 = CARTESIAN_POINT ( 'NONE',  ( 0.2727639067037610499, 3.346456692913386100, 1.417322834645662777 ) ) ;
#3451 = ORIENTED_EDGE ( 'NONE', *, *, #41715, .F. ) ;
#3452 = ORIENTED_EDGE ( 'NONE', *, *, #20598, .F. ) ;
#3453 = CARTESIAN_POINT ( 'NONE',  ( -0.3486774197067339376, 3.267716535433071279, 0.3149606299212577287 ) ) ;
#3454 = LINE ( 'NONE', #46784, #1987 ) ;
#3455 = CIRCLE ( 'NONE', #29848, 2.106299212598425008 ) ;
#3457 = AXIS2_PLACEMENT_3D ( 'NONE', #2628, #18123, #33630 ) ;
#3456 = CARTESIAN_POINT ( 'NONE',  ( 4.268512490100411402E-16, 3.346456692913386100, 2.204724409448808764 ) ) ;
#3458 = EDGE_CURVE ( 'NONE', #21434, #51008, #1916, .T. ) ;
#3459 = CARTESIAN_POINT ( 'NONE',  ( -0.1158910538491989134, 0.02606345816900213982, -1.836661962001401305 ) ) ;
#3460 = CARTESIAN_POINT ( 'NONE',  ( -2.951990591674674480, 1.673246673531018525, -0.08331184815402598032 ) ) ;
#3461 = VERTEX_POINT ( 'NONE', #5278 ) ;
#3462 = ADVANCED_FACE ( 'NONE', ( #21033 ), #36273, .F. ) ;
#3463 = VECTOR ( 'NONE', #27048, 39.37007874015748143 ) ;
#3464 = B_SPLINE_CURVE_WITH_KNOTS ( 'NONE', 3,
 ( #560, #47757, #24562, #31547 ),
 .UNSPECIFIED., .F., .F.,
 ( 4, 4 ),
 ( 0.1211775127643062860, 0.1625894504277921315 ),
 .UNSPECIFIED. ) ;
#3465 = EDGE_CURVE ( 'NONE', #9737, #7396, #49116, .T. ) ;
#3466 = VECTOR ( 'NONE', #9545, 39.37007874015748143 ) ;
#3467 = B_SPLINE_CURVE_WITH_KNOTS ( 'NONE', 3,
 ( #5095, #45083, #36856, #32480 ),
 .UNSPECIFIED., .F., .F.,
 ( 4, 4 ),
 ( 0.004647244867734754738, 0.007368060854785507194 ),
 .UNSPECIFIED. ) ;
#3468 = ORIENTED_EDGE ( 'NONE', *, *, #20957, .F. ) ;
#3469 = LINE ( 'NONE', #30079, #7948 ) ;
#3470 = FACE_OUTER_BOUND ( 'NONE', #6524, .T. ) ;
#3471 = LINE ( 'NONE', #19207, #400 ) ;
#3472 = DIRECTION ( 'NONE',  ( -0.01601477604151182663, 0.9998717552508123996, -0.000000000000000000 ) ) ;
#3473 = DIRECTION ( 'NONE',  ( 1.000000000000000000, -0.000000000000000000, 0.000000000000000000 ) ) ;
#3474 = B_SPLINE_CURVE_WITH_KNOTS ( 'NONE', 3,
 ( #12705, #21222, #4957, #20699 ),
 .UNSPECIFIED., .F., .F.,
 ( 4, 4 ),
 ( 0.01081890587439299049, 0.03073583352486373987 ),
 .UNSPECIFIED. ) ;
#3475 = ORIENTED_EDGE ( 'NONE', *, *, #26253, .T. ) ;
#3476 = CARTESIAN_POINT ( 'NONE',  ( -2.422796457295655959, 1.673308113726643898, -0.1580701165447715717 ) ) ;
#3477 = EDGE_CURVE ( 'NONE', #713, #42090, #41413, .T. ) ;
#3478 = FACE_OUTER_BOUND ( 'NONE', #50517, .T. ) ;
#3479 = ORIENTED_EDGE ( 'NONE', *, *, #36883, .T. ) ;
#3480 = DIRECTION ( 'NONE',  ( -1.000000000000000000, 0.000000000000000000, -0.000000000000000000 ) ) ;
#3481 = ADVANCED_FACE ( 'NONE', ( #32405 ), #8897, .T. ) ;
#3482 = PLANE ( 'NONE',  #22035 ) ;
#3483 = CARTESIAN_POINT ( 'NONE',  ( 2.083034095169011428E-16, 3.267716535433071279, -3.613488146149790065E-32 ) ) ;
#3484 = DIRECTION ( 'NONE',  ( -1.000000000000000000, 0.000000000000000000, 1.734723475976806848E-16 ) ) ;
#3485 = DIRECTION ( 'NONE',  ( -1.000000000000000000, 0.000000000000000000, 1.734723475976806848E-16 ) ) ;
#3486 = DIRECTION ( 'NONE',  ( -0.000000000000000000, 0.000000000000000000, 1.000000000000000000 ) ) ;
#3487 = EDGE_CURVE ( 'NONE', #23037, #44686, #50366, .T. ) ;
#3488 = VERTEX_POINT ( 'NONE', #49371 ) ;
#3489 = DIRECTION ( 'NONE',  ( -1.000000000000000000, 0.000000000000000000, 1.734723475976806848E-16 ) ) ;
#3490 = ORIENTED_EDGE ( 'NONE', *, *, #23462, .T. ) ;
#3491 = CARTESIAN_POINT ( 'NONE',  ( 1.461782879395301160, 6.692913385826772199, -1.598346982901808655 ) ) ;
#3492 = VECTOR ( 'NONE', #37440, 39.37007874015748143 ) ;
#3493 = LINE ( 'NONE', #10736, #35856 ) ;
#3494 = LINE ( 'NONE', #7119, #26823 ) ;
#3495 = VECTOR ( 'NONE', #39892, 39.37007874015748143 ) ;
#3496 = VERTEX_POINT ( 'NONE', #10681 ) ;
#3497 = ORIENTED_EDGE ( 'NONE', *, *, #31581, .F. ) ;
#3498 = DIRECTION ( 'NONE',  ( -1.000000000000000000, 0.000000000000000000, -0.000000000000000000 ) ) ;
#3499 = LINE ( 'NONE', #18989, #46030 ) ;
#3500 = VECTOR ( 'NONE', #136, 39.37007874015748143 ) ;
#3501 = DIRECTION ( 'NONE',  ( -0.000000000000000000, 1.000000000000000000, -0.000000000000000000 ) ) ;
#3502 = CARTESIAN_POINT ( 'NONE',  ( 0.7145799201508789000, 1.574803149606302854, 2.044048657746659448 ) ) ;
#3503 = CARTESIAN_POINT ( 'NONE',  ( 0.8182917201112817063, 0.000000000000000000, -1.929133858267711110 ) ) ;
#3504 = FACE_OUTER_BOUND ( 'NONE', #11513, .T. ) ;
#3505 = AXIS2_PLACEMENT_3D ( 'NONE', #9310, #32047, #33076 ) ;
#3506 = ORIENTED_EDGE ( 'NONE', *, *, #26603, .T. ) ;
#3507 = VERTEX_POINT ( 'NONE', #26173 ) ;
#3508 = CARTESIAN_POINT ( 'NONE',  ( -1.712496953225537633, 3.346456692913386100, 1.417322834645662333 ) ) ;
#3509 = CARTESIAN_POINT ( 'NONE',  ( 1.560669927219590747, 3.346456692913386100, -0.7874015748031473194 ) ) ;
#3510 = VERTEX_POINT ( 'NONE', #18931 ) ;
#3511 = CARTESIAN_POINT ( 'NONE',  ( 0.3136974817028395091, 1.508467219206862664, -2.936457595020219635 ) ) ;
#3512 = ORIENTED_EDGE ( 'NONE', *, *, #17558, .F. ) ;
#3513 = VERTEX_POINT ( 'NONE', #11185 ) ;
#3514 = VERTEX_POINT ( 'NONE', #34683 ) ;
#3515 = ORIENTED_EDGE ( 'NONE', *, *, #39388, .F. ) ;
#3516 = CARTESIAN_POINT ( 'NONE',  ( -2.182111253630085734, 3.346456692913386100, -0.6299212598425177889 ) ) ;
#3517 = VERTEX_POINT ( 'NONE', #29793 ) ;
#3518 = EDGE_CURVE ( 'NONE', #13855, #36871, #18683, .T. ) ;
#3519 = EDGE_CURVE ( 'NONE', #32787, #8317, #14809, .T. ) ;
#3520 = CARTESIAN_POINT ( 'NONE',  ( 0.8182917201112819283, 0.000000000000000000, 0.5905511811023579360 ) ) ;
#3521 = EDGE_CURVE ( 'NONE', #23961, #31953, #33668, .T. ) ;
#3522 = FACE_OUTER_BOUND ( 'NONE', #30560, .T. ) ;
#3523 = EDGE_CURVE ( 'NONE', #24076, #46112, #26420, .T. ) ;
#3524 = CARTESIAN_POINT ( 'NONE',  ( 0.000000000000000000, 3.346456692913386100, 0.000000000000000000 ) ) ;
#3525 = ADVANCED_FACE ( 'NONE', ( #6039 ), #14293, .F. ) ;
#3526 = CARTESIAN_POINT ( 'NONE',  ( -2.438548951736695170, 3.267716535433071279, 0.1574803149606286423 ) ) ;
#3527 = AXIS2_PLACEMENT_3D ( 'NONE', #1928, #49626, #25413 ) ;
#3528 = DIRECTION ( 'NONE',  ( 0.000000000000000000, 0.000000000000000000, 1.000000000000000000 ) ) ;
#3529 = LINE ( 'NONE', #7159, #22167 ) ;
#3530 = ORIENTED_EDGE ( 'NONE', *, *, #49862, .F. ) ;
#3531 = LINE ( 'NONE', #19268, #5197 ) ;
#3532 = LINE ( 'NONE', #3277, #44800 ) ;
#3533 = VECTOR ( 'NONE', #13915, 39.37007874015748143 ) ;
#3534 = PLANE ( 'NONE',  #37566 ) ;
#3535 = DIRECTION ( 'NONE',  ( 1.000000000000000000, 0.000000000000000000, 0.000000000000000000 ) ) ;
#3536 = CONICAL_SURFACE ( 'NONE', #29894, 3.033577403570480779, 1.554780866114618743 ) ;
#3537 = VECTOR ( 'NONE', #8739, 39.37007874015748143 ) ;
#3538 = VERTEX_POINT ( 'NONE', #38315 ) ;
#3539 = CARTESIAN_POINT ( 'NONE',  ( -0.5455278134075214336, 0.000000000000000000, -0.9448818897637762948 ) ) ;
#3540 = EDGE_CURVE ( 'NONE', #10643, #2988, #49866, .T. ) ;
#3541 = ADVANCED_FACE ( 'NONE', ( #30554 ), #42417, .F. ) ;
#3542 = CARTESIAN_POINT ( 'NONE',  ( -2.221680436774566392, 1.680589266716277397, -1.525485796625656087 ) ) ;
#3543 = ORIENTED_EDGE ( 'NONE', *, *, #2114, .T. ) ;
#3544 = DIRECTION ( 'NONE',  ( 1.734723475976806848E-16, 0.000000000000000000, 1.000000000000000000 ) ) ;
#3545 = CARTESIAN_POINT ( 'NONE',  ( 2.437180031585944207, 1.757239404341893518, -1.667735833703099191 ) ) ;
#3546 = AXIS2_PLACEMENT_3D ( 'NONE', #45049, #9452, #25194 ) ;
#3547 = EDGE_CURVE ( 'NONE', #35065, #1059, #22304, .T. ) ;
#3548 = CARTESIAN_POINT ( 'NONE',  ( 2.706338173250262269, 5.118110236220475784, -1.181102362204724310 ) ) ;
#3549 = ORIENTED_EDGE ( 'NONE', *, *, #28158, .T. ) ;
#3550 = CARTESIAN_POINT ( 'NONE',  ( 0.5455278134075217666, 3.346456692913386100, 2.204724409448808764 ) ) ;
#3551 = DIRECTION ( 'NONE',  ( -0.01601477604151182663, 0.9998717552508123996, -0.000000000000000000 ) ) ;
#3552 = FACE_OUTER_BOUND ( 'NONE', #11455, .T. ) ;
#3553 = DIRECTION ( 'NONE',  ( -1.000000000000000000, -0.000000000000000000, -0.000000000000000000 ) ) ;
#3554 = EDGE_LOOP ( 'NONE', ( #48173, #3583, #23201, #8706 ) ) ;
#3555 = VERTEX_POINT ( 'NONE', #42165 ) ;
#3556 = VERTEX_POINT ( 'NONE', #34184 ) ;
#3557 = CARTESIAN_POINT ( 'NONE',  ( -0.6214413264104945434, 3.346456692913386100, 0.1574803149606285035 ) ) ;
#3558 = ORIENTED_EDGE ( 'NONE', *, *, #22776, .F. ) ;
#3559 = LINE ( 'NONE', #15933, #33742 ) ;
#3560 = CARTESIAN_POINT ( 'NONE',  ( -1.647545174055839556, 0.001531214329375737114, 0.5870650656849111249 ) ) ;
#3561 = EDGE_CURVE ( 'NONE', #38385, #47240, #6803, .T. ) ;
#3562 = ORIENTED_EDGE ( 'NONE', *, *, #12927, .F. ) ;
#3563 = CARTESIAN_POINT ( 'NONE',  ( -1.091055626815042645, 3.267716535433071279, 1.692913385826762873 ) ) ;
#3564 = ORIENTED_EDGE ( 'NONE', *, *, #45234, .T. ) ;
#3565 = DIRECTION ( 'NONE',  ( 1.000000000000000000, 0.000000000000000000, 0.000000000000000000 ) ) ;
#3566 = ORIENTED_EDGE ( 'NONE', *, *, #21671, .T. ) ;
#3567 = VERTEX_POINT ( 'NONE', #7061 ) ;
#3568 = PLANE ( 'NONE',  #38882 ) ;
#3569 = AXIS2_PLACEMENT_3D ( 'NONE', #31877, #13015, #27983 ) ;
#3570 = ORIENTED_EDGE ( 'NONE', *, *, #42491, .F. ) ;
#3571 = VECTOR ( 'NONE', #5429, 39.37007874015748143 ) ;
#3572 = AXIS2_PLACEMENT_3D ( 'NONE', #50770, #8231, #39470 ) ;
#3573 = LINE ( 'NONE', #42806, #31171 ) ;
#3574 = B_SPLINE_CURVE_WITH_KNOTS ( 'NONE', 3,
 ( #48348, #15680, #27040, #27549 ),
 .UNSPECIFIED., .F., .F.,
 ( 4, 4 ),
 ( 0.06640258829275558217, 0.1134071559262696122 ),
 .UNSPECIFIED. ) ;
#3575 = EDGE_LOOP ( 'NONE', ( #27214, #47899, #22258, #36873 ) ) ;
#3576 = VERTEX_POINT ( 'NONE', #22548 ) ;
#3577 = DIRECTION ( 'NONE',  ( 0.9510565162951544194, 3.583074652439903135E-17, -0.3090169943749447312 ) ) ;
#3578 = CIRCLE ( 'NONE', #15119, 1.850107469027523432 ) ;
#3579 = EDGE_CURVE ( 'NONE', #31373, #16654, #1643, .T. ) ;
#3580 = CARTESIAN_POINT ( 'NONE',  ( 2.793030215715258446, 1.664308485742666877, 0.9592557174602684977 ) ) ;
#3581 = ORIENTED_EDGE ( 'NONE', *, *, #4699, .T. ) ;
#3582 = CARTESIAN_POINT ( 'NONE',  ( 1.236813753895252832, 5.905511811023623991, -2.681693691597563767 ) ) ;
#3583 = ORIENTED_EDGE ( 'NONE', *, *, #26390, .T. ) ;
#3584 = DIRECTION ( 'NONE',  ( -0.5773502691896253980, 0.5773502691896246208, 0.5773502691896272854 ) ) ;
#3585 = EDGE_CURVE ( 'NONE', #18861, #32922, #34434, .T. ) ;
#3586 = LINE ( 'NONE', #7710, #7729 ) ;
#3587 = EDGE_CURVE ( 'NONE', #11648, #28908, #23015, .T. ) ;
#3588 = EDGE_CURVE ( 'NONE', #20835, #34165, #10426, .T. ) ;
#3589 = LINE ( 'NONE', #30959, #17324 ) ;
#3590 = ORIENTED_EDGE ( 'NONE', *, *, #10962, .F. ) ;
#3591 = ORIENTED_EDGE ( 'NONE', *, *, #22148, .T. ) ;
#3592 = CARTESIAN_POINT ( 'NONE',  ( -0.2834077913992259501, 2.755905511811024056, -0.2440651625074179987 ) ) ;
#3593 = DIRECTION ( 'NONE',  ( 1.000000000000000000, 0.000000000000000000, -3.469446951953613696E-16 ) ) ;
#3594 = DIRECTION ( 'NONE',  ( -0.000000000000000000, 1.000000000000000000, -0.000000000000000000 ) ) ;
#3595 = PLANE ( 'NONE',  #47412 ) ;
#3596 = DIRECTION ( 'NONE',  ( -3.986037398843765983E-20, -1.000000000000000000, -1.160734090543304660E-16 ) ) ;
#3597 = CARTESIAN_POINT ( 'NONE',  ( 0.2727639067037604392, 3.346456692913386100, -0.6692913385826760875 ) ) ;
#3598 = EDGE_CURVE ( 'NONE', #9322, #23592, #38688, .T. ) ;
#3599 = LINE ( 'NONE', #7979, #16022 ) ;
#3600 = VECTOR ( 'NONE', #19696, 39.37007874015748143 ) ;
#3601 = ORIENTED_EDGE ( 'NONE', *, *, #43604, .F. ) ;
#3602 = DIRECTION ( 'NONE',  ( -3.469446951953613696E-16, 0.000000000000000000, -1.000000000000000000 ) ) ;
#3603 = EDGE_CURVE ( 'NONE', #10927, #39048, #49616, .T. ) ;
#3604 = AXIS2_PLACEMENT_3D ( 'NONE', #47384, #50475, #15426 ) ;
#3605 = ORIENTED_EDGE ( 'NONE', *, *, #50952, .T. ) ;
#3606 = AXIS2_PLACEMENT_3D ( 'NONE', #28510, #21035, #40913 ) ;
#3607 = ORIENTED_EDGE ( 'NONE', *, *, #23937, .F. ) ;
#3609 = VECTOR ( 'NONE', #39850, 39.37007874015748143 ) ;
#3608 = DIRECTION ( 'NONE',  ( 0.000000000000000000, 0.000000000000000000, -1.000000000000000000 ) ) ;
#3610 = FACE_OUTER_BOUND ( 'NONE', #25420, .T. ) ;
#3611 = ORIENTED_EDGE ( 'NONE', *, *, #39705, .T. ) ;
#3612 = EDGE_CURVE ( 'NONE', #7991, #42344, #27933, .T. ) ;
#3613 = VECTOR ( 'NONE', #45933, 39.37007874015748143 ) ;
#3614 = DIRECTION ( 'NONE',  ( -0.000000000000000000, 1.000000000000000000, -0.000000000000000000 ) ) ;
#3615 = ORIENTED_EDGE ( 'NONE', *, *, #6256, .T. ) ;
#3616 = CARTESIAN_POINT ( 'NONE',  ( 1.287906020515830141, 3.346456692913386100, -0.3149606299212596716 ) ) ;
#3617 = EDGE_CURVE ( 'NONE', #45769, #23504, #16428, .T. ) ;
#3618 = ORIENTED_EDGE ( 'NONE', *, *, #32168, .F. ) ;
#3619 = CARTESIAN_POINT ( 'NONE',  ( 1.560669927219590747, 3.267716535433071279, 0.1574803149606283648 ) ) ;
#3620 = CARTESIAN_POINT ( 'NONE',  ( 1.091055626815043311, 3.267716535433071279, 1.801691980386208591 ) ) ;
#3621 = EDGE_LOOP ( 'NONE', ( #25946, #12998, #32695, #4252 ) ) ;
#3622 = DIRECTION ( 'NONE',  ( 1.086719731106949452E-16, -1.000000000000000000, -4.078527368698568598E-17 ) ) ;
#3623 = VERTEX_POINT ( 'NONE', #8064 ) ;
#3624 = ORIENTED_EDGE ( 'NONE', *, *, #3018, .F. ) ;
#3625 = EDGE_CURVE ( 'NONE', #2745, #9409, #3943, .T. ) ;
#3626 = DIRECTION ( 'NONE',  ( 1.734723475976806848E-16, 0.000000000000000000, 1.000000000000000000 ) ) ;
#3627 = LINE ( 'NONE', #50805, #21570 ) ;
#3628 = PLANE ( 'NONE',  #27657 ) ;
#3629 = ADVANCED_FACE ( 'NONE', ( #47520 ), #57, .F. ) ;
#3630 = VERTEX_POINT ( 'NONE', #46763 ) ;
#3631 = DIRECTION ( 'NONE',  ( -0.000000000000000000, 1.000000000000000000, -0.000000000000000000 ) ) ;
#3632 = CARTESIAN_POINT ( 'NONE',  ( 2.099568260077707027, 5.118110236220475784, -0.5296909464895783737 ) ) ;
#3633 = ORIENTED_EDGE ( 'NONE', *, *, #35346, .T. ) ;
#3634 = CARTESIAN_POINT ( 'NONE',  ( -0.9104082785719770365, 1.697261530667331764, 2.285716913819229923 ) ) ;
#3635 =( GEOMETRIC_REPRESENTATION_CONTEXT ( 3 ) GLOBAL_UNCERTAINTY_ASSIGNED_CONTEXT ( ( #9692 ) ) GLOBAL_UNIT_ASSIGNED_CONTEXT ( ( #40606, #40097, #4471 ) ) REPRESENTATION_CONTEXT ( 'NONE', 'WORKASPACE' ) );
#3636 = CIRCLE ( 'NONE', #32514, 2.106299212598425008 ) ;
#3637 = ORIENTED_EDGE ( 'NONE', *, *, #17816, .F. ) ;
#3638 = AXIS2_PLACEMENT_3D ( 'NONE', #40107, #32888, #13503 ) ;
#3639 = ORIENTED_EDGE ( 'NONE', *, *, #36140, .F. ) ;
#3640 = AXIS2_PLACEMENT_3D ( 'NONE', #11990, #366, #31879 ) ;
#3641 = EDGE_LOOP ( 'NONE', ( #22144, #21599, #17873, #31217 ) ) ;
#3642 = FACE_OUTER_BOUND ( 'NONE', #11191, .T. ) ;
#3643 = ADVANCED_FACE ( 'NONE', ( #313 ), #47006, .F. ) ;
#3644 = VECTOR ( 'NONE', #6973, 39.37007874015748143 ) ;
#3645 = FACE_OUTER_BOUND ( 'NONE', #6197, .T. ) ;
#3646 = DIRECTION ( 'NONE',  ( 1.734723475976806848E-16, -0.000000000000000000, 1.000000000000000000 ) ) ;
#3647 = EDGE_CURVE ( 'NONE', #22357, #12775, #13959, .T. ) ;
#3648 = DIRECTION ( 'NONE',  ( 0.000000000000000000, 0.000000000000000000, -1.000000000000000000 ) ) ;
#3649 = ORIENTED_EDGE ( 'NONE', *, *, #50062, .F. ) ;
#3650 = ORIENTED_EDGE ( 'NONE', *, *, #5987, .T. ) ;
#3651 = AXIS2_PLACEMENT_3D ( 'NONE', #25769, #18974, #50413 ) ;
#3652 = SURFACE_STYLE_USAGE ( .BOTH. , #19134 ) ;
#3653 = DIRECTION ( 'NONE',  ( -0.9998717552508122886, -0.01601477604151180928, 0.000000000000000000 ) ) ;
#3654 = VERTEX_POINT ( 'NONE', #11683 ) ;
#3655 = CARTESIAN_POINT ( 'NONE',  ( 0.000000000000000000, 3.267716535433071279, 1.535433070866133898 ) ) ;
#3656 = DIRECTION ( 'NONE',  ( -1.000000000000000000, -0.000000000000000000, -0.000000000000000000 ) ) ;
#3657 = DIRECTION ( 'NONE',  ( 0.000000000000000000, 0.000000000000000000, 1.000000000000000000 ) ) ;
#3658 = DIRECTION ( 'NONE',  ( 0.000000000000000000, -1.000000000000000000, -0.000000000000000000 ) ) ;
#3659 = DIRECTION ( 'NONE',  ( 0.000000000000000000, 0.000000000000000000, 1.000000000000000000 ) ) ;
#3660 = EDGE_LOOP ( 'NONE', ( #47399, #50190, #35334, #34817 ) ) ;
#3661 = PLANE ( 'NONE',  #4422 ) ;
#3662 = LINE ( 'NONE', #40314, #23565 ) ;
#3663 = ORIENTED_EDGE ( 'NONE', *, *, #34769, .T. ) ;
#3664 = CARTESIAN_POINT ( 'NONE',  ( -2.365769827427975258, 1.048560651377708153, -0.9576591258817255259 ) ) ;
#3665 = LINE ( 'NONE', #42891, #48406 ) ;
#3666 = CARTESIAN_POINT ( 'NONE',  ( 1.091055626815042645, 0.000000000000000000, -0.5118110236220471121 ) ) ;
#3667 = B_SPLINE_CURVE_WITH_KNOTS ( 'NONE', 3,
 ( #48983, #21158, #29407, #21660 ),
 .UNSPECIFIED., .F., .F.,
 ( 4, 4 ),
 ( 0.1211775127643062444, 0.1625894504277921315 ),
 .UNSPECIFIED. ) ;
#3668 = ORIENTED_EDGE ( 'NONE', *, *, #19340, .T. ) ;
#3669 = EDGE_CURVE ( 'NONE', #36331, #3242, #4192, .T. ) ;
#3670 = VECTOR ( 'NONE', #30014, 39.37007874015748854 ) ;
#3671 = EDGE_LOOP ( 'NONE', ( #2580, #45277, #17784, #49267 ) ) ;
#3672 = AXIS2_PLACEMENT_3D ( 'NONE', #44920, #41330, #45930 ) ;
#3673 = CARTESIAN_POINT ( 'NONE',  ( -2.258024766633058622, 3.267716535433071279, 0.1574803149606286423 ) ) ;
#3674 = ORIENTED_EDGE ( 'NONE', *, *, #4993, .T. ) ;
#3675 = PLANE ( 'NONE',  #12219 ) ;
#3676 = EDGE_CURVE ( 'NONE', #1152, #23942, #43512, .T. ) ;
#3677 = AXIS2_PLACEMENT_3D ( 'NONE', #42783, #38675, #22669 ) ;
#3678 = VERTEX_POINT ( 'NONE', #39050 ) ;
#3679 = DIRECTION ( 'NONE',  ( -3.469446951953613696E-16, 0.000000000000000000, -1.000000000000000000 ) ) ;
#3680 = DIRECTION ( 'NONE',  ( -3.469446951953613696E-16, 0.000000000000000000, -1.000000000000000000 ) ) ;
#3681 = DIRECTION ( 'NONE',  ( -0.000000000000000000, 0.000000000000000000, 1.000000000000000000 ) ) ;
#3682 = EDGE_CURVE ( 'NONE', #472, #10946, #12195, .T. ) ;
#3683 = ADVANCED_FACE ( 'NONE', ( #43162 ), #3689, .F. ) ;
#3684 = ORIENTED_EDGE ( 'NONE', *, *, #12782, .F. ) ;
#3685 = ORIENTED_EDGE ( 'NONE', *, *, #14361, .F. ) ;
#3686 = ORIENTED_EDGE ( 'NONE', *, *, #42836, .F. ) ;
#3687 = CARTESIAN_POINT ( 'NONE',  ( -1.675725316865139813, 1.615445346360514733, 1.399291623245470184 ) ) ;
#3688 = VECTOR ( 'NONE', #3553, 39.37007874015748143 ) ;
#3689 = PLANE ( 'NONE',  #34561 ) ;
#3690 = VERTEX_POINT ( 'NONE', #7812 ) ;
#3691 = EDGE_LOOP ( 'NONE', ( #24160, #4989, #38301, #44971 ) ) ;
#3692 = DIRECTION ( 'NONE',  ( 1.734723475976806848E-16, -0.000000000000000000, 1.000000000000000000 ) ) ;
#3693 = CARTESIAN_POINT ( 'NONE',  ( 1.909347346926324462, 3.346456692913386100, -0.9842519685039348154 ) ) ;
#3694 = CARTESIAN_POINT ( 'NONE',  ( 0.07982360342473591996, 1.709180471932028711, 0.000000000000000000 ) ) ;
#3695 = VERTEX_POINT ( 'NONE', #23551 ) ;
#3696 = ORIENTED_EDGE ( 'NONE', *, *, #36115, .F. ) ;
#3697 = DIRECTION ( 'NONE',  ( 1.000000000000000000, 0.000000000000000000, 0.000000000000000000 ) ) ;
#3698 = CARTESIAN_POINT ( 'NONE',  ( -0.4788131938641533303, 1.525670379232220375, 2.914091152102185944 ) ) ;
#3699 = DIRECTION ( 'NONE',  ( -0.000000000000000000, 1.000000000000000000, -0.000000000000000000 ) ) ;
#3700 = ADVANCED_FACE ( 'NONE', ( #35689 ), #39485, .F. ) ;
#3701 = EDGE_LOOP ( 'NONE', ( #43866, #27919, #49186, #28211 ) ) ;
#3702 = LINE ( 'NONE', #35198, #21595 ) ;
#3703 = LINE ( 'NONE', #7828, #19443 ) ;
#3704 = ORIENTED_EDGE ( 'NONE', *, *, #9337, .F. ) ;
#3705 = CARTESIAN_POINT ( 'NONE',  ( 0.000000000000000000, 6.692913385826772199, 0.000000000000000000 ) ) ;
#3706 = EDGE_LOOP ( 'NONE', ( #21359, #40431, #26582, #33419 ) ) ;
#3707 = ORIENTED_EDGE ( 'NONE', *, *, #9473, .T. ) ;
#3708 = CARTESIAN_POINT ( 'NONE',  ( -1.068402561569948617, 1.205361022782829114E-17, -1.884154513482188431 ) ) ;
#3709 = FACE_OUTER_BOUND ( 'NONE', #33870, .T. ) ;
#3710 = ADVANCED_FACE ( 'NONE', ( #8320 ), #4445, .T. ) ;
#3711 = LINE ( 'NONE', #47288, #13233 ) ;
#3712 = CARTESIAN_POINT ( 'NONE',  ( 1.560669927219590303, 3.346456692913386100, -1.732283464566923170 ) ) ;
#3713 = ADVANCED_FACE ( 'NONE', ( #24068 ), #20184, .F. ) ;
#3714 = DIRECTION ( 'NONE',  ( 1.000000000000000000, -0.000000000000000000, 0.000000000000000000 ) ) ;
#3715 = EDGE_LOOP ( 'NONE', ( #30235, #14422, #22333, #17458 ) ) ;
#3716 = VERTEX_POINT ( 'NONE', #38807 ) ;
#3717 = AXIS2_PLACEMENT_3D ( 'NONE', #37204, #33080, #48766 ) ;
#3718 = VECTOR ( 'NONE', #4453, 39.37007874015748143 ) ;
#3719 = VECTOR ( 'NONE', #35606, 39.37007874015748143 ) ;
#3720 = VERTEX_POINT ( 'NONE', #3436 ) ;
#3721 = DIRECTION ( 'NONE',  ( -3.469446951953613696E-16, 0.000000000000000000, -1.000000000000000000 ) ) ;
#3722 = CARTESIAN_POINT ( 'NONE',  ( -2.919165122154194769, 1.575328909575085090, 0.4450898352768660748 ) ) ;
#3723 = AXIS2_PLACEMENT_3D ( 'NONE', #37097, #44815, #1715 ) ;
#3724 = CARTESIAN_POINT ( 'NONE',  ( 0.1155636338427008941, -0.5222242541845523167, 0.000000000000000000 ) ) ;
#3725 = CARTESIAN_POINT ( 'NONE',  ( 0.8182917201112817063, 3.267716535433071279, -1.417322834645664331 ) ) ;
#3726 = AXIS2_PLACEMENT_3D ( 'NONE', #24646, #40900, #378 ) ;
#3727 = ORIENTED_EDGE ( 'NONE', *, *, #16699, .F. ) ;
#3728 = DIRECTION ( 'NONE',  ( -3.469446951953613696E-16, 0.000000000000000000, -1.000000000000000000 ) ) ;
#3729 = CARTESIAN_POINT ( 'NONE',  ( 1.887300604142603921, 1.205361022782829114E-17, 0.9597141752041703500 ) ) ;
#3730 = ORIENTED_EDGE ( 'NONE', *, *, #49685, .F. ) ;
#3731 = LINE ( 'NONE', #39100, #38885 ) ;
#3732 = DIRECTION ( 'NONE',  ( -0.000000000000000000, 1.000000000000000000, -0.000000000000000000 ) ) ;
#3733 = CARTESIAN_POINT ( 'NONE',  ( 2.164823134740036625, 2.755905511811027164, -0.04796011690015051371 ) ) ;
#3734 = ORIENTED_EDGE ( 'NONE', *, *, #24644, .T. ) ;
#3735 = CARTESIAN_POINT ( 'NONE',  ( -2.258024766633058622, 3.267716535433071279, 7.834097144030835427E-16 ) ) ;
#3736 = CARTESIAN_POINT ( 'NONE',  ( 0.000000000000000000, 1.574803149606302854, 0.000000000000000000 ) ) ;
#3737 = DIRECTION ( 'NONE',  ( 0.7071067811865466846, 0.000000000000000000, 0.7071067811865483499 ) ) ;
#3738 = ORIENTED_EDGE ( 'NONE', *, *, #19711, .F. ) ;
#3739 = DIRECTION ( 'NONE',  ( -3.469446951953613696E-16, 0.000000000000000000, -1.000000000000000000 ) ) ;
#3740 = ORIENTED_EDGE ( 'NONE', *, *, #27137, .F. ) ;
#3741 = DIRECTION ( 'NONE',  ( -0.000000000000000000, 1.000000000000000000, -0.000000000000000000 ) ) ;
#3742 = DIRECTION ( 'NONE',  ( -0.000000000000000000, 1.000000000000000000, -0.000000000000000000 ) ) ;
#3743 = CARTESIAN_POINT ( 'NONE',  ( -0.07591351300297348448, 3.267716535433071279, 2.633779063002574070E-17 ) ) ;
#3744 = ADVANCED_FACE ( 'NONE', ( #34931 ), #22220, .F. ) ;
#3745 = EDGE_CURVE ( 'NONE', #41713, #17882, #47698, .T. ) ;
#3746 = EDGE_CURVE ( 'NONE', #31869, #50064, #28185, .T. ) ;
#3747 = ORIENTED_EDGE ( 'NONE', *, *, #17184, .F. ) ;
#3748 = ORIENTED_EDGE ( 'NONE', *, *, #30790, .T. ) ;
#3749 = DIRECTION ( 'NONE',  ( 0.000000000000000000, 0.000000000000000000, -1.000000000000000000 ) ) ;
#3750 = VECTOR ( 'NONE', #4048, 39.37007874015748143 ) ;
#3751 = CARTESIAN_POINT ( 'NONE',  ( 2.168245791271197209, 1.654581109258766558, -2.004968704497248400 ) ) ;
#3752 = AXIS2_PLACEMENT_3D ( 'NONE', #20387, #47713, #4388 ) ;
#3753 = ORIENTED_EDGE ( 'NONE', *, *, #19086, .F. ) ;
#3754 = DIRECTION ( 'NONE',  ( -1.000000000000000000, -0.000000000000000000, -0.000000000000000000 ) ) ;
#3755 = CARTESIAN_POINT ( 'NONE',  ( -1.091055626815042201, 3.346456692913386100, 1.377952755905504256 ) ) ;
#3756 = DIRECTION ( 'NONE',  ( -0.000000000000000000, 1.000000000000000000, -0.000000000000000000 ) ) ;
#3757 = CIRCLE ( 'NONE', #11972, 2.164630168518208109 ) ;
#3758 = EDGE_CURVE ( 'NONE', #39512, #39570, #9341, .T. ) ;
#3759 = DIRECTION ( 'NONE',  ( 1.734723475976806848E-16, -0.000000000000000000, 1.000000000000000000 ) ) ;
#3760 = EDGE_LOOP ( 'NONE', ( #49814, #40533, #15984, #36563 ) ) ;
#3761 = DIRECTION ( 'NONE',  ( -0.000000000000000000, 1.000000000000000000, -0.000000000000000000 ) ) ;
#3762 = CARTESIAN_POINT ( 'NONE',  ( -1.330011864698828816, 1.686599376747761614, -1.746878811320646152 ) ) ;
#3763 = AXIS2_PLACEMENT_3D ( 'NONE', #36663, #28644, #43870 ) ;
#3764 = CARTESIAN_POINT ( 'NONE',  ( -0.8942052331142547050, 0.000000000000000000, 0.7480314960629874665 ) ) ;
#3765 = AXIS2_PLACEMENT_3D ( 'NONE', #50856, #39044, #15797 ) ;
#3766 = ORIENTED_EDGE ( 'NONE', *, *, #19246, .T. ) ;
#3767 = DIRECTION ( 'NONE',  ( 0.2660368455666826115, 1.118798511145731007E-16, -0.9639628606958511314 ) ) ;
#3768 = ORIENTED_EDGE ( 'NONE', *, *, #19726, .F. ) ;
#3769 = VERTEX_POINT ( 'NONE', #41103 ) ;
#3770 = EDGE_CURVE ( 'NONE', #35404, #47863, #5209, .T. ) ;
#3771 = PLANE ( 'NONE',  #39908 ) ;
#3772 = EDGE_CURVE ( 'NONE', #19191, #34229, #11523, .T. ) ;
#3773 = ORIENTED_EDGE ( 'NONE', *, *, #50240, .F. ) ;
#3774 = EDGE_LOOP ( 'NONE', ( #12550, #6789, #27025, #48731 ) ) ;
#3775 = LINE ( 'NONE', #27255, #40948 ) ;
#3776 = EDGE_CURVE ( 'NONE', #25971, #20686, #17599, .T. ) ;
#3777 = ORIENTED_EDGE ( 'NONE', *, *, #27813, .T. ) ;
#3778 = EDGE_CURVE ( 'NONE', #45969, #47335, #12968, .T. ) ;
#3779 = DIRECTION ( 'NONE',  ( 1.000000000000000000, 0.000000000000000000, -3.469446951953613696E-16 ) ) ;
#3780 = EDGE_CURVE ( 'NONE', #4026, #14569, #28699, .T. ) ;
#3781 = LINE ( 'NONE', #50958, #30181 ) ;
#3782 = CARTESIAN_POINT ( 'NONE',  ( -0.8221900955658363319, -2.487559435141135932E-16, 2.050660405798877317 ) ) ;
#3783 = FACE_OUTER_BOUND ( 'NONE', #42562, .T. ) ;
#3784 = CARTESIAN_POINT ( 'NONE',  ( 0.000000000000000000, 6.692913385826772199, 0.000000000000000000 ) ) ;
#3785 = CARTESIAN_POINT ( 'NONE',  ( 2.121469926805689354, 1.574803149606302854, -0.4337334748181394528 ) ) ;
#3786 = CIRCLE ( 'NONE', #45811, 2.165354330708661568 ) ;
#3787 = VERTEX_POINT ( 'NONE', #830 ) ;
#3788 = LINE ( 'NONE', #26510, #8486 ) ;
#3789 = VECTOR ( 'NONE', #42313, 39.37007874015748143 ) ;
#3790 = CARTESIAN_POINT ( 'NONE',  ( 0.9914495361338622192, 1.493354361723550294, 2.781765111341823360 ) ) ;
#3791 = CONICAL_SURFACE ( 'NONE', #30185, 2.165354330708661568, 0.2617993877991570129 ) ;
#3792 = PLANE ( 'NONE',  #34747 ) ;
#3793 = EDGE_LOOP ( 'NONE', ( #29626, #45828, #5865, #26585 ) ) ;
#3794 = CARTESIAN_POINT ( 'NONE',  ( 2.437180031585944207, 1.459818316683583639, -1.667735833703099191 ) ) ;
#3795 = CARTESIAN_POINT ( 'NONE',  ( 2.099568260077706583, 1.574803149606302854, -0.5296909464895790398 ) ) ;
#3796 = ORIENTED_EDGE ( 'NONE', *, *, #28196, .T. ) ;
#3797 = DIRECTION ( 'NONE',  ( 1.734723475976806848E-16, -0.000000000000000000, 1.000000000000000000 ) ) ;
#3798 = VECTOR ( 'NONE', #39322, 39.37007874015748143 ) ;
#3799 = CARTESIAN_POINT ( 'NONE',  ( 0.9319704666822036243, 0.04284687812831378811, 1.655805649632502430 ) ) ;
#3800 = CIRCLE ( 'NONE', #5459, 2.246510896728926010 ) ;
#3801 = CARTESIAN_POINT ( 'NONE',  ( 0.2727639067037610499, 0.000000000000000000, 2.047244094488179567 ) ) ;
#3802 = EDGE_LOOP ( 'NONE', ( #46498, #34553, #37375, #19055 ) ) ;
#3803 = DIRECTION ( 'NONE',  ( 1.734723475976806848E-16, -0.000000000000000000, 1.000000000000000000 ) ) ;
#3804 = DIRECTION ( 'NONE',  ( 0.01601477604151182663, -0.9998717552508123996, 0.000000000000000000 ) ) ;
#3805 = DIRECTION ( 'NONE',  ( 0.000000000000000000, -1.000000000000000000, 0.000000000000000000 ) ) ;
#3806 = DIRECTION ( 'NONE',  ( 1.734723475976806848E-16, -0.000000000000000000, 1.000000000000000000 ) ) ;
#3807 = VERTEX_POINT ( 'NONE', #5727 ) ;
#3808 = EDGE_CURVE ( 'NONE', #30118, #50026, #1596, .T. ) ;
#3809 = ORIENTED_EDGE ( 'NONE', *, *, #45756, .T. ) ;
#3810 = ORIENTED_EDGE ( 'NONE', *, *, #41193, .T. ) ;
#3811 = EDGE_CURVE ( 'NONE', #28015, #21029, #44446, .T. ) ;
#3812 = B_SPLINE_CURVE_WITH_KNOTS ( 'NONE', 3,
 ( #47102, #45659, #15650, #29693 ),
 .UNSPECIFIED., .F., .F.,
 ( 4, 4 ),
 ( 6.235017842663103921E-07, 0.001940962322214974823 ),
 .UNSPECIFIED. ) ;
#3813 = VERTEX_POINT ( 'NONE', #16841 ) ;
#3814 = CARTESIAN_POINT ( 'NONE',  ( -0.2727639067037607723, 3.346456692913386100, -0.7874015748031470974 ) ) ;
#3815 = CARTESIAN_POINT ( 'NONE',  ( -0.8182917201112819283, 0.000000000000000000, -1.417322834645664331 ) ) ;
#3816 = EDGE_LOOP ( 'NONE', ( #43733, #22905, #38181, #38699 ) ) ;
#3817 = ADVANCED_FACE ( 'NONE', ( #32599 ), #33110, .F. ) ;
#3818 = CARTESIAN_POINT ( 'NONE',  ( 0.7423782071083085965, 3.267716535433071279, -2.575641807848709701E-16 ) ) ;
#3819 = ORIENTED_EDGE ( 'NONE', *, *, #34136, .T. ) ;
#3820 = FACE_OUTER_BOUND ( 'NONE', #48296, .T. ) ;
#3821 = AXIS2_PLACEMENT_3D ( 'NONE', #10400, #46736, #26143 ) ;
#3822 = CIRCLE ( 'NONE', #1353, 2.246510896728926010 ) ;
#3823 = ORIENTED_EDGE ( 'NONE', *, *, #40980, .T. ) ;
#3824 = EDGE_LOOP ( 'NONE', ( #2343, #47409, #48934, #14906 ) ) ;
#3825 = VECTOR ( 'NONE', #28028, 39.37007874015748143 ) ;
#3826 = CARTESIAN_POINT ( 'NONE',  ( -1.363819533518803029, 0.000000000000000000, 0.4724409448818871482 ) ) ;
#3827 = ORIENTED_EDGE ( 'NONE', *, *, #17562, .T. ) ;
#3828 = AXIS2_PLACEMENT_3D ( 'NONE', #2368, #33368, #21736 ) ;
#3829 = CARTESIAN_POINT ( 'NONE',  ( -2.770917298715281252, 0.6859011407150840123, -3.558318873518431680 ) ) ;
#3830 = ADVANCED_FACE ( 'NONE', ( #8574 ), #40587, .T. ) ;
#3831 = AXIS2_PLACEMENT_3D ( 'NONE', #34207, #26196, #49894 ) ;
#3832 = VERTEX_POINT ( 'NONE', #36207 ) ;
#3833 = ORIENTED_EDGE ( 'NONE', *, *, #33179, .F. ) ;
#3834 = LINE ( 'NONE', #27310, #28126 ) ;
#3835 = B_SPLINE_CURVE_WITH_KNOTS ( 'NONE', 3,
 ( #13251, #37259, #49075, #1874 ),
 .UNSPECIFIED., .F., .F.,
 ( 4, 4 ),
 ( 0.01136448766669267627, 0.03073633765498568968 ),
 .UNSPECIFIED. ) ;
#3836 = VECTOR ( 'NONE', #16591, 39.37007874015748143 ) ;
#3837 = ADVANCED_FACE ( 'NONE', ( #44689 ), #25090, .F. ) ;
#3838 = CARTESIAN_POINT ( 'NONE',  ( -2.151809081513409438, 6.692913385826772199, 0.2418202932658334581 ) ) ;
#3839 = EDGE_CURVE ( 'NONE', #36975, #47775, #2290, .T. ) ;
#3840 = ORIENTED_EDGE ( 'NONE', *, *, #2709, .T. ) ;
#3841 = CARTESIAN_POINT ( 'NONE',  ( -3.346456692913385211, 0.000000000000000000, -4.133858267716536083 ) ) ;
#3842 = ORIENTED_EDGE ( 'NONE', *, *, #49454, .F. ) ;
#3843 = CARTESIAN_POINT ( 'NONE',  ( 1.698224779224786429, 1.735102128624146811, -1.555582603516539875 ) ) ;
#3844 = CARTESIAN_POINT ( 'NONE',  ( -1.672606463373382590, 0.000000000000000000, 0.4917175957957677923 ) ) ;
#3845 = CARTESIAN_POINT ( 'NONE',  ( 0.000000000000000000, 3.267716535433071279, -1.259842519685034468 ) ) ;
#3846 = ORIENTED_EDGE ( 'NONE', *, *, #8624, .F. ) ;
#3847 = ORIENTED_EDGE ( 'NONE', *, *, #35594, .T. ) ;
#3848 =( REPRESENTATION_RELATIONSHIP ('NONE','NONE', #50198, #34429 ) REPRESENTATION_RELATIONSHIP_WITH_TRANSFORMATION ( #19876 )SHAPE_REPRESENTATION_RELATIONSHIP( ) );
#3849 = CARTESIAN_POINT ( 'NONE',  ( -0.3486774197067340486, 3.346456692913386100, 2.007874015748021268 ) ) ;
#3850 = LINE ( 'NONE', #50274, #13802 ) ;
#3851 = DIRECTION ( 'NONE',  ( 1.734723475976806848E-16, -0.000000000000000000, 1.000000000000000000 ) ) ;
#3852 = LINE ( 'NONE', #35352, #48226 ) ;
#3853 = CARTESIAN_POINT ( 'NONE',  ( -2.875073865529052419, 1.576011620654163226, -0.6730429436919832531 ) ) ;
#3854 = CARTESIAN_POINT ( 'NONE',  ( -0.2483447015969799665, 1.715384992028094358, -2.942339451689540031 ) ) ;
#3855 = ORIENTED_EDGE ( 'NONE', *, *, #38524, .T. ) ;
#3856 = AXIS2_PLACEMENT_3D ( 'NONE', #9770, #10022, #16813 ) ;
#3857 = CARTESIAN_POINT ( 'NONE',  ( -1.712496953225537188, 3.267716535433071279, 0.4724409448818871482 ) ) ;
#3858 = ORIENTED_EDGE ( 'NONE', *, *, #43191, .T. ) ;
#3859 = VECTOR ( 'NONE', #47105, 39.37007874015748143 ) ;
#3860 = DIRECTION ( 'NONE',  ( 1.000000000000000000, 0.000000000000000000, 0.000000000000000000 ) ) ;
#3861 = ORIENTED_EDGE ( 'NONE', *, *, #42894, .T. ) ;
#3862 = DIRECTION ( 'NONE',  ( -1.000000000000000000, -0.000000000000000000, -0.000000000000000000 ) ) ;
#3863 = FACE_OUTER_BOUND ( 'NONE', #36099, .T. ) ;
#3864 = VECTOR ( 'NONE', #13498, 39.37007874015748143 ) ;
#3865 = ORIENTED_EDGE ( 'NONE', *, *, #16176, .T. ) ;
#3866 = VECTOR ( 'NONE', #2369, 39.37007874015748854 ) ;
#3867 = EDGE_CURVE ( 'NONE', #42867, #24046, #40843, .T. ) ;
#3868 = LINE ( 'NONE', #12123, #41938 ) ;
#3869 = EDGE_CURVE ( 'NONE', #28527, #6610, #3474, .T. ) ;
#3870 = ORIENTED_EDGE ( 'NONE', *, *, #31340, .T. ) ;
#3871 = CARTESIAN_POINT ( 'NONE',  ( -1.363819533518803029, 0.000000000000000000, 1.417322834645662777 ) ) ;
#3872 = ORIENTED_EDGE ( 'NONE', *, *, #32213, .T. ) ;
#3873 = EDGE_CURVE ( 'NONE', #39604, #32922, #48030, .T. ) ;
#3874 = CARTESIAN_POINT ( 'NONE',  ( 0.5455278134075212115, 0.000000000000000000, -6.146657985744592735E-16 ) ) ;
#3875 = CARTESIAN_POINT ( 'NONE',  ( -0.5455278134075217666, 3.267716535433071279, 9.463399047163231808E-17 ) ) ;
#3876 = EDGE_CURVE ( 'NONE', #9331, #2040, #17853, .T. ) ;
#3877 = EDGE_CURVE ( 'NONE', #32968, #13111, #6494, .T. ) ;
#3878 = VERTEX_POINT ( 'NONE', #26356 ) ;
#3879 = CARTESIAN_POINT ( 'NONE',  ( 2.919426793319799707, 1.448220119383965443, 0.4451252810446820196 ) ) ;
#3880 = ORIENTED_EDGE ( 'NONE', *, *, #12937, .T. ) ;
#3881 = ORIENTED_EDGE ( 'NONE', *, *, #627, .F. ) ;
#3882 = FACE_OUTER_BOUND ( 'NONE', #42788, .T. ) ;
#3883 = DIRECTION ( 'NONE',  ( 0.1938878870612536220, 0.000000000000000000, 0.9810236935216818388 ) ) ;
#3884 = DIRECTION ( 'NONE',  ( -0.000000000000000000, -1.000000000000000000, -0.000000000000000000 ) ) ;
#3885 = ORIENTED_EDGE ( 'NONE', *, *, #29445, .T. ) ;
#3886 = PLANE ( 'NONE',  #27023 ) ;
#3887 = EDGE_CURVE ( 'NONE', #1038, #1681, #18362, .T. ) ;
#3888 = LINE ( 'NONE', #8267, #42325 ) ;
#3889 = VECTOR ( 'NONE', #2029, 39.37007874015748143 ) ;
#3890 = AXIS2_PLACEMENT_3D ( 'NONE', #7105, #22850, #38603 ) ;
#3891 = ORIENTED_EDGE ( 'NONE', *, *, #26620, .T. ) ;
#3892 = DIRECTION ( 'NONE',  ( -1.000000000000000000, 0.000000000000000000, 0.000000000000000000 ) ) ;
#3893 = AXIS2_PLACEMENT_3D ( 'NONE', #36818, #13579, #41703 ) ;
#3894 = EDGE_CURVE ( 'NONE', #9591, #32984, #2364, .T. ) ;
#3895 = ORIENTED_EDGE ( 'NONE', *, *, #33238, .T. ) ;
#3896 = EDGE_LOOP ( 'NONE', ( #1827, #1530, #6855, #28080 ) ) ;
#3897 = ORIENTED_EDGE ( 'NONE', *, *, #32265, .T. ) ;
#3898 = CARTESIAN_POINT ( 'NONE',  ( -1.636583440222564301, 3.346456692913386100, 1.377952755905504256 ) ) ;
#3899 = LINE ( 'NONE', #39518, #24988 ) ;
#3900 = EDGE_CURVE ( 'NONE', #10170, #19859, #37992, .T. ) ;
#3901 = FACE_OUTER_BOUND ( 'NONE', #34242, .T. ) ;
#3902 = CARTESIAN_POINT ( 'NONE',  ( -2.889674983507169337, 1.575792602931942232, -0.6090712660038034576 ) ) ;
#3903 = ORIENTED_EDGE ( 'NONE', *, *, #19551, .F. ) ;
#3904 = ORIENTED_EDGE ( 'NONE', *, *, #29954, .T. ) ;
#3905 = DIRECTION ( 'NONE',  ( -0.9749279121818259508, -2.578990239907041302E-17, 0.2225209339563041788 ) ) ;
#3906 = FACE_OUTER_BOUND ( 'NONE', #30984, .T. ) ;
#3907 = VECTOR ( 'NONE', #49773, 39.37007874015748143 ) ;
#3908 = ORIENTED_EDGE ( 'NONE', *, *, #34418, .T. ) ;
#3909 = CARTESIAN_POINT ( 'NONE',  ( -0.8182917201112814842, 0.000000000000000000, 1.535433070866133898 ) ) ;
#3910 = EDGE_CURVE ( 'NONE', #42214, #28697, #34115, .T. ) ;
#3911 = DIRECTION ( 'NONE',  ( 0.01601477604151182663, -0.9998717552508123996, 0.000000000000000000 ) ) ;
#3912 = LINE ( 'NONE', #14330, #46996 ) ;
#3913 = DIRECTION ( 'NONE',  ( -0.000000000000000000, 1.000000000000000000, -0.000000000000000000 ) ) ;
#3914 = LINE ( 'NONE', #16559, #42549 ) ;
#3915 = CARTESIAN_POINT ( 'NONE',  ( 0.9587803188866059756, 1.007227695720354754, 2.414603754317795392 ) ) ;
#3916 = ORIENTED_EDGE ( 'NONE', *, *, #7955, .F. ) ;
#3917 = CARTESIAN_POINT ( 'NONE',  ( 1.412396057062171861, 6.692913385826772199, 1.691415513056039988 ) ) ;
#3918 = CARTESIAN_POINT ( 'NONE',  ( -0.3739466299075467348, 0.000000000000000000, -1.120342228065320134 ) ) ;
#3919 = ORIENTED_EDGE ( 'NONE', *, *, #49429, .T. ) ;
#3920 = ORIENTED_EDGE ( 'NONE', *, *, #47904, .T. ) ;
#3921 = CARTESIAN_POINT ( 'NONE',  ( 1.363819533518803029, 3.267716535433071279, -1.102362204724405714 ) ) ;
#3922 = DIRECTION ( 'NONE',  ( -3.469446951953613696E-16, 0.000000000000000000, -1.000000000000000000 ) ) ;
#3923 = DIRECTION ( 'NONE',  ( -0.000000000000000000, -1.000000000000000000, 0.000000000000000000 ) ) ;
#3924 = AXIS2_PLACEMENT_3D ( 'NONE', #44499, #40641, #29011 ) ;
#3925 = ORIENTED_EDGE ( 'NONE', *, *, #42786, .T. ) ;
#3926 = VECTOR ( 'NONE', #46440, 39.37007874015748143 ) ;
#3927 = ORIENTED_EDGE ( 'NONE', *, *, #3877, .T. ) ;
#3928 = DIRECTION ( 'NONE',  ( -3.469446951953613696E-16, 0.000000000000000000, -1.000000000000000000 ) ) ;
#3929 = VECTOR ( 'NONE', #18063, 39.37007874015748143 ) ;
#3930 = ORIENTED_EDGE ( 'NONE', *, *, #46196, .F. ) ;
#3931 = LINE ( 'NONE', #19406, #1494 ) ;
#3932 = ORIENTED_EDGE ( 'NONE', *, *, #16184, .T. ) ;
#3933 = EDGE_CURVE ( 'NONE', #10525, #37287, #17016, .T. ) ;
#3934 = CARTESIAN_POINT ( 'NONE',  ( -0.8942052331142547050, 0.000000000000000000, 1.377952755905504256 ) ) ;
#3935 = DIRECTION ( 'NONE',  ( 1.000000000000000000, 0.000000000000000000, 0.000000000000000000 ) ) ;
#3936 = DIRECTION ( 'NONE',  ( -5.207613805428889878E-18, -1.000000000000000000, 1.159565308550899675E-16 ) ) ;
#3937 = EDGE_CURVE ( 'NONE', #43163, #47500, #21986, .T. ) ;
#3938 = VECTOR ( 'NONE', #37700, 39.37007874015748143 ) ;
#3939 = VERTEX_POINT ( 'NONE', #45443 ) ;
#3940 = EDGE_LOOP ( 'NONE', ( #40661, #48022, #4146, #35435 ) ) ;
#3941 = ORIENTED_EDGE ( 'NONE', *, *, #16193, .F. ) ;
#3942 = DIRECTION ( 'NONE',  ( -1.000000000000000000, 0.000000000000000000, 1.734723475976806848E-16 ) ) ;
#3943 = LINE ( 'NONE', #39813, #15607 ) ;
#3944 = VERTEX_POINT ( 'NONE', #34371 ) ;
#3945 = ORIENTED_EDGE ( 'NONE', *, *, #28787, .F. ) ;
#3946 = CARTESIAN_POINT ( 'NONE',  ( 1.636583440222563635, 0.000000000000000000, -0.9448818897637765168 ) ) ;
#3947 = LINE ( 'NONE', #19679, #27733 ) ;
#3948 = CARTESIAN_POINT ( 'NONE',  ( -1.166969139818015755, 3.346456692913386100, -0.03937007874015868020 ) ) ;
#3949 = CONICAL_SURFACE ( 'NONE', #29494, 1.850107469027523210, 0.6386652850508578450 ) ;
#3950 = EDGE_LOOP ( 'NONE', ( #20624, #45570, #50015, #38903 ) ) ;
#3951 = ORIENTED_EDGE ( 'NONE', *, *, #47694, .F. ) ;
#3952 = CARTESIAN_POINT ( 'NONE',  ( 0.000000000000000000, 3.267716535433071279, 0.000000000000000000 ) ) ;
#3953 = CARTESIAN_POINT ( 'NONE',  ( -0.7572931579105153244, 1.049866565877818125, 1.877743133795977792 ) ) ;
#3954 = LINE ( 'NONE', #27433, #18752 ) ;
#3955 = EDGE_LOOP ( 'NONE', ( #2573, #39036, #34564, #5801 ) ) ;
#3956 = PLANE ( 'NONE',  #23233 ) ;
#3957 = FACE_OUTER_BOUND ( 'NONE', #17099, .T. ) ;
#3958 = VERTEX_POINT ( 'NONE', #34618 ) ;
#3959 = CARTESIAN_POINT ( 'NONE',  ( 0.2727639067037610499, 3.267716535433071279, 2.362204724409437961 ) ) ;
#3960 = VERTEX_POINT ( 'NONE', #30491 ) ;
#3961 = ORIENTED_EDGE ( 'NONE', *, *, #47366, .T. ) ;
#3962 = DIRECTION ( 'NONE',  ( 1.000000000000000000, 0.000000000000000000, 0.000000000000000000 ) ) ;
#3963 = DIRECTION ( 'NONE',  ( 0.04486483035050446017, 0.000000000000000000, 0.9989930665413151445 ) ) ;
#3964 = DIRECTION ( 'NONE',  ( -0.000000000000000000, 1.000000000000000000, -0.000000000000000000 ) ) ;
#3965 = VECTOR ( 'NONE', #19290, 39.37007874015748143 ) ;
#3966 = VECTOR ( 'NONE', #2033, 39.37007874015748143 ) ;
#3967 = ADVANCED_FACE ( 'NONE', ( #6992 ), #49801, .F. ) ;
#3968 = CARTESIAN_POINT ( 'NONE',  ( -1.004926760980926481, 2.755905511811024056, -0.6205843980233154422 ) ) ;
#3969 = DIRECTION ( 'NONE',  ( 1.734723475976806848E-16, -0.000000000000000000, 1.000000000000000000 ) ) ;
#3970 = EDGE_LOOP ( 'NONE', ( #33240, #8455, #14326, #5955 ) ) ;
#3971 = ORIENTED_EDGE ( 'NONE', *, *, #25858, .F. ) ;
#3972 = AXIS2_PLACEMENT_3D ( 'NONE', #19439, #27193, #35205 ) ;
#3973 = ORIENTED_EDGE ( 'NONE', *, *, #41734, .F. ) ;
#3974 = DIRECTION ( 'NONE',  ( 1.000000000000000000, 0.000000000000000000, -3.469446951953613696E-16 ) ) ;
#3975 = ADVANCED_FACE ( 'NONE', ( #2106 ), #8166, .T. ) ;
#3976 = DIRECTION ( 'NONE',  ( 8.741157232058247392E-17, -1.000000000000000000, -7.636919086868415696E-17 ) ) ;
#3977 = AXIS2_PLACEMENT_3D ( 'NONE', #36450, #28943, #33609 ) ;
#3978 = EDGE_CURVE ( 'NONE', #45979, #45433, #23822, .T. ) ;
#3979 = VECTOR ( 'NONE', #43515, 39.37007874015748143 ) ;
#3980 = DIRECTION ( 'NONE',  ( 0.000000000000000000, 0.000000000000000000, -1.000000000000000000 ) ) ;
#3981 = DIRECTION ( 'NONE',  ( -1.000000000000000000, 0.000000000000000000, -0.000000000000000000 ) ) ;
#3982 = ORIENTED_EDGE ( 'NONE', *, *, #44828, .T. ) ;
#3983 = FACE_OUTER_BOUND ( 'NONE', #48661, .T. ) ;
#3984 = EDGE_CURVE ( 'NONE', #20840, #1905, #42349, .T. ) ;
#3985 = AXIS2_PLACEMENT_3D ( 'NONE', #41141, #37268, #17635 ) ;
#3986 = FACE_OUTER_BOUND ( 'NONE', #10959, .T. ) ;
#3987 = EDGE_CURVE ( 'NONE', #721, #6366, #13731, .T. ) ;
#3988 = ORIENTED_EDGE ( 'NONE', *, *, #29359, .T. ) ;
#3989 = CARTESIAN_POINT ( 'NONE',  ( 0.1968503937007878568, 3.346456692913386100, 2.204724409448808764 ) ) ;
#3990 = DIRECTION ( 'NONE',  ( 1.734723475976806848E-16, 0.000000000000000000, 1.000000000000000000 ) ) ;
#3991 = DIRECTION ( 'NONE',  ( -0.01601477604151182663, 0.9998717552508123996, -0.000000000000000000 ) ) ;
#3992 = ORIENTED_EDGE ( 'NONE', *, *, #39130, .F. ) ;
#3993 = LINE ( 'NONE', #19724, #14384 ) ;
#3994 = CARTESIAN_POINT ( 'NONE',  ( -0.3486774197067339376, 0.000000000000000000, -0.3149606299212593941 ) ) ;
#3995 = DIRECTION ( 'NONE',  ( -0.000000000000000000, 1.000000000000000000, -0.000000000000000000 ) ) ;
#3996 = ORIENTED_EDGE ( 'NONE', *, *, #10396, .T. ) ;
#3997 = DIRECTION ( 'NONE',  ( 0.000000000000000000, 0.000000000000000000, -1.000000000000000000 ) ) ;
#3998 = ORIENTED_EDGE ( 'NONE', *, *, #40975, .T. ) ;
#3999 = CARTESIAN_POINT ( 'NONE',  ( 0.9914495361338622192, 1.493354361723550294, 2.781765111341823360 ) ) ;
#4000 = ADVANCED_FACE ( 'NONE', ( #22742 ), #25594, .F. ) ;
#4001 = LINE ( 'NONE', #1139, #10322 ) ;
#4002 = CARTESIAN_POINT ( 'NONE',  ( 0.8182917201112824834, 3.267716535433071279, 2.004783788421103718 ) ) ;
#4003 = AXIS2_PLACEMENT_3D ( 'NONE', #15120, #41733, #30108 ) ;
#4004 = EDGE_CURVE ( 'NONE', #17434, #48626, #9054, .T. ) ;
#4005 = VERTEX_POINT ( 'NONE', #38246 ) ;
#4006 = ORIENTED_EDGE ( 'NONE', *, *, #43960, .T. ) ;
#4007 = CARTESIAN_POINT ( 'NONE',  ( 1.287906020515830141, 3.267716535433071279, -4.468321617281355077E-16 ) ) ;
#4008 = ADVANCED_FACE ( 'NONE', ( #45695 ), #41602, .T. ) ;
#4009 = DIRECTION ( 'NONE',  ( -0.9909497617679352555, 0.000000000000000000, 0.1342332658176522697 ) ) ;
#4010 = VERTEX_POINT ( 'NONE', #11616 ) ;
#4011 = DIRECTION ( 'NONE',  ( -1.000000000000000000, 0.000000000000000000, 0.000000000000000000 ) ) ;
#4012 = VECTOR ( 'NONE', #43087, 39.37007874015748143 ) ;
#4013 = DIRECTION ( 'NONE',  ( -0.9998717552508122886, -0.01601477604151180928, 0.000000000000000000 ) ) ;
#4014 = CARTESIAN_POINT ( 'NONE',  ( -1.405431157298717260, 1.652583001446659816, 1.683443543830524414 ) ) ;
#4015 = CARTESIAN_POINT ( 'NONE',  ( 1.472697644137372697, 1.731489898814932316, 1.760436233057293354 ) ) ;
#4016 = VECTOR ( 'NONE', #36539, 39.37007874015748143 ) ;
#4017 = CIRCLE ( 'NONE', #32894, 2.952755905511811552 ) ;
#4018 = VERTEX_POINT ( 'NONE', #23236 ) ;
#4019 = DIRECTION ( 'NONE',  ( 1.000000000000000000, 0.000000000000000000, 0.000000000000000000 ) ) ;
#4020 = CARTESIAN_POINT ( 'NONE',  ( 0.2727639067037610499, 3.267716535433071279, 1.417322834645662777 ) ) ;
#4021 = ADVANCED_FACE ( 'NONE', ( #46947 ), #44055, .T. ) ;
#4022 = VECTOR ( 'NONE', #10588, 39.37007874015748143 ) ;
#4023 = LINE ( 'NONE', #47598, #18270 ) ;
#4024 = VERTEX_POINT ( 'NONE', #27357 ) ;
#4025 = CARTESIAN_POINT ( 'NONE',  ( -0.07591351300297359550, 3.346456692913386100, -2.047244094488181343 ) ) ;
#4026 = VERTEX_POINT ( 'NONE', #47457 ) ;
#4027 = VERTEX_POINT ( 'NONE', #12131 ) ;
#4028 = VECTOR ( 'NONE', #38410, 39.37007874015748143 ) ;
#4029 = CARTESIAN_POINT ( 'NONE',  ( 0.4696143004045479352, 3.346456692913386100, -0.7874015748031473194 ) ) ;
#4030 = ORIENTED_EDGE ( 'NONE', *, *, #7842, .T. ) ;
#4032 = EDGE_LOOP ( 'NONE', ( #21578, #15959, #12852, #31525 ) ) ;
#4031 = EDGE_CURVE ( 'NONE', #41056, #26744, #26853, .T. ) ;
#4033 = CARTESIAN_POINT ( 'NONE',  ( 0.1968503937007874405, 3.346456692913386100, 0.000000000000000000 ) ) ;
#4034 = B_SPLINE_CURVE_WITH_KNOTS ( 'NONE', 3,
 ( #6490, #50297, #33612, #38244 ),
 .UNSPECIFIED., .F., .F.,
 ( 4, 4 ),
 ( 6.486800511562401857E-07, 0.004335704572669431961 ),
 .UNSPECIFIED. ) ;
#4035 = ORIENTED_EDGE ( 'NONE', *, *, #8635, .T. ) ;
#4036 = DIRECTION ( 'NONE',  ( 1.000000000000000000, 0.000000000000000000, -3.469446951953613696E-16 ) ) ;
#4037 = PLANE ( 'NONE',  #37634 ) ;
#4038 = DIRECTION ( 'NONE',  ( 0.9989930665413144784, 0.000000000000000000, 0.04486483035051863633 ) ) ;
#4039 = EDGE_CURVE ( 'NONE', #25208, #18779, #43098, .T. ) ;
#4040 = VECTOR ( 'NONE', #50426, 39.37007874015748854 ) ;
#4041 = EDGE_CURVE ( 'NONE', #36033, #23187, #24000, .T. ) ;
#4042 = DIRECTION ( 'NONE',  ( 0.000000000000000000, 0.000000000000000000, -1.000000000000000000 ) ) ;
#4043 = EDGE_CURVE ( 'NONE', #10848, #31608, #35123, .T. ) ;
#4044 = CARTESIAN_POINT ( 'NONE',  ( 1.833433833923351353, 3.346456692913386100, -1.036830145017913596 ) ) ;
#4045 = CARTESIAN_POINT ( 'NONE',  ( 1.386843392441768241, 1.730114785850798587, -1.825100698618727257 ) ) ;
#4046 = ORIENTED_EDGE ( 'NONE', *, *, #20099, .F. ) ;
#4047 = DIRECTION ( 'NONE',  ( -0.01601477604151182663, 0.9998717552508123996, -0.000000000000000000 ) ) ;
#4048 = DIRECTION ( 'NONE',  ( 1.000000000000000000, -0.000000000000000000, 0.000000000000000000 ) ) ;
#4049 = DIRECTION ( 'NONE',  ( 0.000000000000000000, 0.000000000000000000, -1.000000000000000000 ) ) ;
#4050 = B_SPLINE_CURVE_WITH_KNOTS ( 'NONE', 3,
 ( #22443, #34068, #39393, #35518 ),
 .UNSPECIFIED., .F., .F.,
 ( 4, 4 ),
 ( 6.183086360362561446E-07, 0.001526023582687786959 ),
 .UNSPECIFIED. ) ;
#4051 = AXIS2_PLACEMENT_3D ( 'NONE', #37497, #18117, #13482 ) ;
#4052 = VECTOR ( 'NONE', #9368, 39.37007874015748143 ) ;
#4053 = ORIENTED_EDGE ( 'NONE', *, *, #15996, .T. ) ;
#4054 = CARTESIAN_POINT ( 'NONE',  ( 0.000000000000000000, 3.267716535433071279, -0.7874015748031473194 ) ) ;
#4055 = FACE_OUTER_BOUND ( 'NONE', #23077, .T. ) ;
#4056 = EDGE_LOOP ( 'NONE', ( #43439, #30094, #557, #43054 ) ) ;
#4057 = DIRECTION ( 'NONE',  ( 1.000000000000000000, -0.000000000000000000, 0.000000000000000000 ) ) ;
#4058 = CARTESIAN_POINT ( 'NONE',  ( -1.062992125984251635, 0.5905511811023621549, -1.062992125984252079 ) ) ;
#4059 = AXIS2_PLACEMENT_3D ( 'NONE', #46751, #46256, #14543 ) ;
#4060 = CARTESIAN_POINT ( 'NONE',  ( -1.775400203342670347, 1.593155925640307835, -2.359903268218729089 ) ) ;
#4061 = LINE ( 'NONE', #47380, #44682 ) ;
#4062 = EDGE_CURVE ( 'NONE', #27577, #8496, #42605, .T. ) ;
#4063 = VECTOR ( 'NONE', #47311, 39.37007874015748143 ) ;
#4064 = ORIENTED_EDGE ( 'NONE', *, *, #26659, .T. ) ;
#4065 = DIRECTION ( 'NONE',  ( 1.734723475976806848E-16, 0.000000000000000000, 1.000000000000000000 ) ) ;
#4066 = CARTESIAN_POINT ( 'NONE',  ( -1.166969139818015533, 3.267716535433071279, 4.048737525165544183E-16 ) ) ;
#4067 = EDGE_CURVE ( 'NONE', #11914, #44591, #23484, .T. ) ;
#4068 = FACE_OUTER_BOUND ( 'NONE', #17287, .T. ) ;
#4069 = DIRECTION ( 'NONE',  ( 1.734723475976806848E-16, -0.000000000000000000, 1.000000000000000000 ) ) ;
#4070 = ORIENTED_EDGE ( 'NONE', *, *, #17207, .F. ) ;
#4071 = EDGE_CURVE ( 'NONE', #6252, #14452, #48961, .T. ) ;
#4072 = EDGE_LOOP ( 'NONE', ( #15699, #44834, #5868, #20971 ) ) ;
#4073 = VERTEX_POINT ( 'NONE', #31252 ) ;
#4074 = DIRECTION ( 'NONE',  ( -1.000000000000000000, -0.000000000000000000, -0.000000000000000000 ) ) ;
#4075 = EDGE_CURVE ( 'NONE', #43798, #10470, #13901, .T. ) ;
#4076 = ORIENTED_EDGE ( 'NONE', *, *, #41516, .T. ) ;
#4077 = CARTESIAN_POINT ( 'NONE',  ( -1.574237088929739459, 0.000000000000000000, 0.7912475138866331692 ) ) ;
#4078 = CARTESIAN_POINT ( 'NONE',  ( -2.029373727807297634, 0.5254167564079418318, 0.7111286833828837084 ) ) ;
#4079 = ORIENTED_EDGE ( 'NONE', *, *, #14437, .T. ) ;
#4080 = DIRECTION ( 'NONE',  ( 1.000000000000000000, 0.000000000000000000, 0.000000000000000000 ) ) ;
#4081 = VECTOR ( 'NONE', #22240, 39.37007874015748143 ) ;
#4082 = ORIENTED_EDGE ( 'NONE', *, *, #37733, .T. ) ;
#4083 = CARTESIAN_POINT ( 'NONE',  ( -0.8182917201112819283, 0.000000000000000000, -0.6692913385826760875 ) ) ;
#4084 = CARTESIAN_POINT ( 'NONE',  ( 0.000000000000000000, 5.118110236220475784, 0.000000000000000000 ) ) ;
#4085 = ORIENTED_EDGE ( 'NONE', *, *, #19872, .T. ) ;
#4086 = ORIENTED_EDGE ( 'NONE', *, *, #2884, .F. ) ;
#4087 = CARTESIAN_POINT ( 'NONE',  ( -1.909347346926324462, 0.000000000000000000, 0.9055118110236167750 ) ) ;
#4088 = ORIENTED_EDGE ( 'NONE', *, *, #28864, .F. ) ;
#4089 = B_SPLINE_CURVE_WITH_KNOTS ( 'NONE', 3,
 ( #20871, #16752, #12359, #23977 ),
 .UNSPECIFIED., .F., .F.,
 ( 4, 4 ),
 ( 0.1211873102087489551, 0.1625992483279400103 ),
 .UNSPECIFIED. ) ;
#4090 = VECTOR ( 'NONE', #2387, 39.37007874015748854 ) ;
#4091 = CARTESIAN_POINT ( 'NONE',  ( 1.636583440222563857, 3.267716535433071279, 0.1181102362204701633 ) ) ;
#4092 = ORIENTED_EDGE ( 'NONE', *, *, #12545, .F. ) ;
#4093 = VERTEX_POINT ( 'NONE', #27607 ) ;
#4094 = CARTESIAN_POINT ( 'NONE',  ( 1.015142113812069091, 0.000000000000000000, -1.732283464566923614 ) ) ;
#4095 = DIRECTION ( 'NONE',  ( 0.000000000000000000, 0.000000000000000000, -1.000000000000000000 ) ) ;
#4096 = ORIENTED_EDGE ( 'NONE', *, *, #26659, .F. ) ;
#4097 = CIRCLE ( 'NONE', #45278, 2.165354330708661568 ) ;
#4098 = CARTESIAN_POINT ( 'NONE',  ( -0.2727639067037602172, 3.346456692913386100, 0.7874015748031456541 ) ) ;
#4099 = ORIENTED_EDGE ( 'NONE', *, *, #43031, .F. ) ;
#4100 = LINE ( 'NONE', #8477, #6304 ) ;
#4101 = DIRECTION ( 'NONE',  ( 0.000000000000000000, 1.000000000000000000, 0.000000000000000000 ) ) ;
#4102 = DIRECTION ( 'NONE',  ( -0.000000000000000000, -1.000000000000000000, -0.000000000000000000 ) ) ;
#4103 = EDGE_LOOP ( 'NONE', ( #50125, #2228, #13862, #12884, #9667, #2772, #15477, #18382, #19379, #46321, #49552 ) ) ;
#4104 = EDGE_LOOP ( 'NONE', ( #8643, #44794, #35310, #17285 ) ) ;
#4105 = EDGE_CURVE ( 'NONE', #28109, #42832, #14994, .T. ) ;
#4106 = CARTESIAN_POINT ( 'NONE',  ( 1.015142113812069313, 0.000000000000000000, -0.7874015748031473194 ) ) ;
#4107 = CARTESIAN_POINT ( 'NONE',  ( 0.000000000000000000, 3.267716535433071279, 1.692913385826762873 ) ) ;
#4108 = EDGE_CURVE ( 'NONE', #12775, #7408, #41601, .T. ) ;
#4109 = LINE ( 'NONE', #19830, #242 ) ;
#4110 = DIRECTION ( 'NONE',  ( 0.04486483035051863633, -1.160734090543304660E-16, -0.9989930665413144784 ) ) ;
#4111 = EDGE_CURVE ( 'NONE', #23557, #42367, #247, .T. ) ;
#4112 = DIRECTION ( 'NONE',  ( -3.469446951953613696E-16, 0.000000000000000000, -1.000000000000000000 ) ) ;
#4113 = CARTESIAN_POINT ( 'NONE',  ( 0.3530705266098149164, 2.755905511811024056, -0.1234057657284599735 ) ) ;
#4114 = VECTOR ( 'NONE', #47597, 39.37007874015748143 ) ;
#4115 = VERTEX_POINT ( 'NONE', #27107 ) ;
#4116 = FACE_OUTER_BOUND ( 'NONE', #49295, .T. ) ;
#4117 = VERTEX_POINT ( 'NONE', #7497 ) ;
#4118 = LINE ( 'NONE', #36123, #10223 ) ;
#4119 = ORIENTED_EDGE ( 'NONE', *, *, #42928, .F. ) ;
#4120 = DIRECTION ( 'NONE',  ( 1.241861098869888840E-16, 1.000000000000000000, -3.427318860986102267E-17 ) ) ;
#4121 = CONICAL_SURFACE ( 'NONE', #31318, 3.483074324928249421, 1.244861948955335196 ) ;
#4122 = DIRECTION ( 'NONE',  ( 0.9998717552508121775, 0.01601477604151182663, 0.000000000000000000 ) ) ;
#4123 = EDGE_CURVE ( 'NONE', #1865, #36153, #35434, .T. ) ;
#4124 = ORIENTED_EDGE ( 'NONE', *, *, #32936, .F. ) ;
#4125 = LINE ( 'NONE', #11861, #50931 ) ;
#4126 = EDGE_CURVE ( 'NONE', #19249, #42663, #14804, .T. ) ;
#4127 = ORIENTED_EDGE ( 'NONE', *, *, #7056, .F. ) ;
#4128 = CARTESIAN_POINT ( 'NONE',  ( 0.6150616064519864867, 0.03777100275179151589, 1.778883059170359493 ) ) ;
#4129 = VECTOR ( 'NONE', #8057, 39.37007874015748143 ) ;
#4130 = ORIENTED_EDGE ( 'NONE', *, *, #8855, .T. ) ;
#4131 = CARTESIAN_POINT ( 'NONE',  ( -2.182111253630085734, 3.346456692913386100, -0.8267716535433052849 ) ) ;
#4132 = CARTESIAN_POINT ( 'NONE',  ( 1.363819533518803251, 0.000000000000000000, -0.6692913385826764205 ) ) ;
#4133 = VERTEX_POINT ( 'NONE', #19106 ) ;
#4134 = DIRECTION ( 'NONE',  ( -1.000000000000000000, -0.000000000000000000, -0.000000000000000000 ) ) ;
#4135 = ORIENTED_EDGE ( 'NONE', *, *, #1568, .T. ) ;
#4136 = VERTEX_POINT ( 'NONE', #50547 ) ;
#4137 = CARTESIAN_POINT ( 'NONE',  ( 0.000000000000000000, 2.755905511811024056, 0.000000000000000000 ) ) ;
#4138 = PLANE ( 'NONE',  #32254 ) ;
#4139 = FACE_OUTER_BOUND ( 'NONE', #44805, .T. ) ;
#4140 = ORIENTED_EDGE ( 'NONE', *, *, #15173, .F. ) ;
#4141 = FACE_OUTER_BOUND ( 'NONE', #49980, .T. ) ;
#4142 = CARTESIAN_POINT ( 'NONE',  ( -0.5455278134075208785, 3.267716535433071279, 1.062992125984246083 ) ) ;
#4143 = ORIENTED_EDGE ( 'NONE', *, *, #12176, .T. ) ;
#4144 = CARTESIAN_POINT ( 'NONE',  ( -2.182111253630085734, 3.346456692913386100, -0.9448818897637762948 ) ) ;
#4145 = ORIENTED_EDGE ( 'NONE', *, *, #47823, .F. ) ;
#4146 = ORIENTED_EDGE ( 'NONE', *, *, #38884, .T. ) ;
#4147 = ORIENTED_EDGE ( 'NONE', *, *, #6845, .T. ) ;
#4148 = DIRECTION ( 'NONE',  ( -0.5773502691896259531, 0.5773502691896245098, -0.5773502691896270633 ) ) ;
#4149 = VECTOR ( 'NONE', #18770, 39.37007874015748143 ) ;
#4150 = CARTESIAN_POINT ( 'NONE',  ( -2.576863348864732117, 5.905511811023623991, 1.442554885838411849 ) ) ;
#4151 = VECTOR ( 'NONE', #21889, 39.37007874015748143 ) ;
#4152 = FACE_OUTER_BOUND ( 'NONE', #40839, .T. ) ;
#4153 = LINE ( 'NONE', #24289, #9875 ) ;
#4154 = ORIENTED_EDGE ( 'NONE', *, *, #42271, .T. ) ;
#4155 = ORIENTED_EDGE ( 'NONE', *, *, #48945, .F. ) ;
#4156 = ADVANCED_FACE ( 'NONE', ( #15243 ), #30994, .F. ) ;
#4157 = FACE_OUTER_BOUND ( 'NONE', #6053, .T. ) ;
#4158 = EDGE_CURVE ( 'NONE', #16832, #4956, #17041, .T. ) ;
#4159 = DIRECTION ( 'NONE',  ( 1.000000000000000000, -0.000000000000000000, 0.000000000000000000 ) ) ;
#4160 = AXIS2_PLACEMENT_3D ( 'NONE', #19854, #7493, #244 ) ;
#4161 = ORIENTED_EDGE ( 'NONE', *, *, #50443, .F. ) ;
#4162 = DIRECTION ( 'NONE',  ( 1.000000000000000000, -0.000000000000000000, 0.000000000000000000 ) ) ;
#4163 = EDGE_CURVE ( 'NONE', #29523, #13784, #4898, .T. ) ;
#4164 = DIRECTION ( 'NONE',  ( 0.01601477604151182663, -0.9998717552508123996, 0.000000000000000000 ) ) ;
#4165 = LINE ( 'NONE', #19385, #41577 ) ;
#4166 = DIRECTION ( 'NONE',  ( 0.000000000000000000, 0.000000000000000000, 1.000000000000000000 ) ) ;
#4167 = CARTESIAN_POINT ( 'NONE',  ( 0.000000000000000000, 2.755905511811027164, 0.000000000000000000 ) ) ;
#4168 = ORIENTED_EDGE ( 'NONE', *, *, #44598, .T. ) ;
#4169 = CARTESIAN_POINT ( 'NONE',  ( 0.8182917201112819283, 3.346456692913386100, -0.7874015748031473194 ) ) ;
#4170 = ORIENTED_EDGE ( 'NONE', *, *, #621, .F. ) ;
#4171 = VERTEX_POINT ( 'NONE', #29152 ) ;
#4172 = DIRECTION ( 'NONE',  ( 1.000000000000000000, 0.000000000000000000, 0.000000000000000000 ) ) ;
#4173 = DIRECTION ( 'NONE',  ( 8.673617379884035472E-17, 0.000000000000000000, 1.000000000000000000 ) ) ;
#4174 = EDGE_CURVE ( 'NONE', #37363, #31047, #50767, .T. ) ;
#4175 = CARTESIAN_POINT ( 'NONE',  ( 0.000000000000000000, 5.905511811023623991, 0.000000000000000000 ) ) ;
#4176 = ORIENTED_EDGE ( 'NONE', *, *, #20331, .F. ) ;
#4177 = EDGE_CURVE ( 'NONE', #50925, #37890, #46500, .T. ) ;
#4178 = ORIENTED_EDGE ( 'NONE', *, *, #22215, .T. ) ;
#4179 = CARTESIAN_POINT ( 'NONE',  ( 0.5665031287202806354, 0.01222701028677279297, -1.867693841696119517 ) ) ;
#4180 = ORIENTED_EDGE ( 'NONE', *, *, #45242, .T. ) ;
#4181 = DIRECTION ( 'NONE',  ( 0.000000000000000000, 1.000000000000000000, 0.000000000000000000 ) ) ;
#4182 = ORIENTED_EDGE ( 'NONE', *, *, #43505, .F. ) ;
#4183 = AXIS2_PLACEMENT_3D ( 'NONE', #19581, #30967, #46177 ) ;
#4184 = CARTESIAN_POINT ( 'NONE',  ( 1.443330927545150910, 3.346456692913386100, -1.614173228346452715 ) ) ;
#4185 = CARTESIAN_POINT ( 'NONE',  ( -0.3486774197067334935, 3.267716535433071279, 1.209717811016577352E-16 ) ) ;
#4186 = DIRECTION ( 'NONE',  ( -1.000000000000000000, 0.000000000000000000, 0.000000000000000000 ) ) ;
#4187 = CONICAL_SURFACE ( 'NONE', #3343, 1.850107469027523210, 0.6386652850508578450 ) ;
#4188 = ORIENTED_EDGE ( 'NONE', *, *, #13638, .T. ) ;
#4189 = VERTEX_POINT ( 'NONE', #25029 ) ;
#4190 = ORIENTED_EDGE ( 'NONE', *, *, #41792, .T. ) ;
#4191 = CARTESIAN_POINT ( 'NONE',  ( 0.000000000000000000, 1.574803149606302854, 0.000000000000000000 ) ) ;
#4192 = LINE ( 'NONE', #47773, #32918 ) ;
#4193 = VERTEX_POINT ( 'NONE', #4646 ) ;
#4194 = VERTEX_POINT ( 'NONE', #16258 ) ;
#4195 = FACE_OUTER_BOUND ( 'NONE', #2202, .T. ) ;
#4196 = DIRECTION ( 'NONE',  ( -0.01601477604151182663, 0.9998717552508123996, -0.000000000000000000 ) ) ;
#4197 = VECTOR ( 'NONE', #8456, 39.37007874015748143 ) ;
#4198 = CARTESIAN_POINT ( 'NONE',  ( -1.091055626815042201, 0.000000000000000000, 0.3149606299212580063 ) ) ;
#4199 = B_SPLINE_CURVE_WITH_KNOTS ( 'NONE', 3,
 ( #22328, #14830, #13117, #26441 ),
 .UNSPECIFIED., .F., .F.,
 ( 4, 4 ),
 ( 2.471583195156979454E-07, 0.002500589363332148332 ),
 .UNSPECIFIED. ) ;
#4200 = ADVANCED_FACE ( 'NONE', ( #1278 ), #13185, .T. ) ;
#4201 = ORIENTED_EDGE ( 'NONE', *, *, #32144, .F. ) ;
#4202 = ORIENTED_EDGE ( 'NONE', *, *, #7548, .T. ) ;
#4203 = DIRECTION ( 'NONE',  ( 1.000000000000000000, -0.000000000000000000, 0.000000000000000000 ) ) ;
#4204 = DIRECTION ( 'NONE',  ( -3.469446951953613696E-16, 0.000000000000000000, -1.000000000000000000 ) ) ;
#4205 = VERTEX_POINT ( 'NONE', #32018 ) ;
#4206 = PLANE ( 'NONE',  #27353 ) ;
#4207 = CARTESIAN_POINT ( 'NONE',  ( -1.025452293874513199, 0.4349011127721511549, 1.051609096396380005 ) ) ;
#4208 = ORIENTED_EDGE ( 'NONE', *, *, #34073, .T. ) ;
#4209 = CARTESIAN_POINT ( 'NONE',  ( -0.8244711865321519006, 0.01471425056033665718, -1.598608591632243892 ) ) ;
#4210 = EDGE_LOOP ( 'NONE', ( #24378, #44238, #9921, #46517 ) ) ;
#4211 = EDGE_LOOP ( 'NONE', ( #23107, #32326, #33615 ) ) ;
#4212 = CARTESIAN_POINT ( 'NONE',  ( 0.000000000000000000, 2.755905511811024056, 0.000000000000000000 ) ) ;
#4213 = CARTESIAN_POINT ( 'NONE',  ( 2.138597145901430352, 1.574803149606302854, 0.3393547186367255608 ) ) ;
#4214 = CARTESIAN_POINT ( 'NONE',  ( -0.04921259842519758176, 5.905511811023623103, 2.952755905511810663 ) ) ;
#4215 = CARTESIAN_POINT ( 'NONE',  ( 0.7423782071083085965, 3.267716535433071279, -0.5118110236220467790 ) ) ;
#4216 = ORIENTED_EDGE ( 'NONE', *, *, #42960, .T. ) ;
#4217 = ORIENTED_EDGE ( 'NONE', *, *, #51006, .T. ) ;
#4218 = AXIS2_PLACEMENT_3D ( 'NONE', #36097, #28078, #40481 ) ;
#4219 = ORIENTED_EDGE ( 'NONE', *, *, #17462, .F. ) ;
#4220 = CARTESIAN_POINT ( 'NONE',  ( -1.909347346926324462, 3.346456692913386100, 0.4724409448818871482 ) ) ;
#4221 = LINE ( 'NONE', #20481, #17694 ) ;
#4222 = ADVANCED_FACE ( 'NONE', ( #36656 ), #9865, .T. ) ;
#4223 = VECTOR ( 'NONE', #38600, 39.37007874015748143 ) ;
#4224 = VECTOR ( 'NONE', #44692, 39.37007874015748143 ) ;
#4225 = EDGE_CURVE ( 'NONE', #31499, #42563, #9048, .T. ) ;
#4226 = EDGE_CURVE ( 'NONE', #4194, #42469, #43864, .T. ) ;
#4227 = DIRECTION ( 'NONE',  ( 0.000000000000000000, -1.000000000000000000, 0.000000000000000000 ) ) ;
#4228 = DIRECTION ( 'NONE',  ( -1.000000000000000000, -0.000000000000000000, -0.000000000000000000 ) ) ;
#4229 = ORIENTED_EDGE ( 'NONE', *, *, #49705, .F. ) ;
#4230 = CARTESIAN_POINT ( 'NONE',  ( 1.560669927219590747, 3.267716535433071279, 0.7874015748031454320 ) ) ;
#4231 = DIRECTION ( 'NONE',  ( -0.5773502691896265082, 0.5773502691896255090, -0.5773502691896251759 ) ) ;
#4232 = EDGE_LOOP ( 'NONE', ( #22749, #21481, #45871, #26634 ) ) ;
#4233 = VECTOR ( 'NONE', #27784, 39.37007874015748143 ) ;
#4234 = LINE ( 'NONE', #48075, #5939 ) ;
#4235 = CARTESIAN_POINT ( 'NONE',  ( -1.146850602398337360, 0.5249316475426863970, -1.494778961359568337 ) ) ;
#4236 = EDGE_CURVE ( 'NONE', #20947, #27229, #36396, .T. ) ;
#4237 = LINE ( 'NONE', #28230, #6539 ) ;
#4238 = ORIENTED_EDGE ( 'NONE', *, *, #21310, .F. ) ;
#4239 = CARTESIAN_POINT ( 'NONE',  ( 0.000000000000000000, 3.267716535433071279, 0.1181102362204703021 ) ) ;
#4240 = CARTESIAN_POINT ( 'NONE',  ( 2.059921668671832240, -8.380087113460787161E-17, 0.7210543110491615115 ) ) ;
#4241 = FACE_OUTER_BOUND ( 'NONE', #6102, .T. ) ;
#4242 = VERTEX_POINT ( 'NONE', #16521 ) ;
#4243 = CARTESIAN_POINT ( 'NONE',  ( 0.2727639067037602172, 3.346456692913386100, -2.047244094488182231 ) ) ;
#4244 = CARTESIAN_POINT ( 'NONE',  ( -1.439733046521776139, 3.267716535433071279, 0.9448818897637749625 ) ) ;
#4245 = VERTEX_POINT ( 'NONE', #28379 ) ;
#4246 = CARTESIAN_POINT ( 'NONE',  ( 1.091055626815042645, 0.000000000000000000, -0.1968503937007883287 ) ) ;
#4247 = DIRECTION ( 'NONE',  ( -1.000000000000000000, 0.000000000000000000, 1.734723475976806848E-16 ) ) ;
#4248 = CARTESIAN_POINT ( 'NONE',  ( 0.5455278134075211005, 0.000000000000000000, 0.1181102362204701633 ) ) ;
#4249 = DIRECTION ( 'NONE',  ( -3.469446951953613696E-16, 0.000000000000000000, -1.000000000000000000 ) ) ;
#4250 = EDGE_CURVE ( 'NONE', #38635, #16977, #48225, .T. ) ;
#4251 = ORIENTED_EDGE ( 'NONE', *, *, #22247, .F. ) ;
#4252 = ORIENTED_EDGE ( 'NONE', *, *, #18350, .F. ) ;
#4253 = DIRECTION ( 'NONE',  ( -1.000000000000000000, -0.000000000000000000, -0.000000000000000000 ) ) ;
#4254 = CARTESIAN_POINT ( 'NONE',  ( 2.139229417893225182, 6.692913385826772199, -0.3394403656973405958 ) ) ;
#4255 = ORIENTED_EDGE ( 'NONE', *, *, #7491, .T. ) ;
#4256 = CARTESIAN_POINT ( 'NONE',  ( 0.1968503937007877735, 0.000000000000000000, 1.062992125984246083 ) ) ;
#4257 = DIRECTION ( 'NONE',  ( -0.9749279121818227312, 2.586762438145473843E-17, -0.2225209339563184452 ) ) ;
#4258 = CARTESIAN_POINT ( 'NONE',  ( 1.287906020515829919, 3.346456692913386100, -1.574803149606294417 ) ) ;
#4259 = EDGE_CURVE ( 'NONE', #18093, #40146, #25593, .T. ) ;
#4260 = AXIS2_PLACEMENT_3D ( 'NONE', #17896, #14021, #29767 ) ;
#4261 = CARTESIAN_POINT ( 'NONE',  ( -1.775400203342670347, 1.691590761327236958, -2.359903268218729089 ) ) ;
#4262 = ORIENTED_EDGE ( 'NONE', *, *, #13481, .F. ) ;
#4263 = AXIS2_PLACEMENT_3D ( 'NONE', #33698, #22563, #33942 ) ;
#4264 = VERTEX_POINT ( 'NONE', #13412 ) ;
#4265 = LINE ( 'NONE', #39634, #8954 ) ;
#4266 = CARTESIAN_POINT ( 'NONE',  ( 0.8182917201112819283, 3.267716535433071279, -0.7874015748031473194 ) ) ;
#4267 = CARTESIAN_POINT ( 'NONE',  ( -3.927031490892378253E-16, 0.000000000000000000, -1.889763779527552146 ) ) ;
#4268 = DIRECTION ( 'NONE',  ( -0.000000000000000000, 0.000000000000000000, 1.000000000000000000 ) ) ;
#4269 = VECTOR ( 'NONE', #20769, 39.37007874015748143 ) ;
#4270 = FACE_BOUND ( 'NONE', #38038, .T. ) ;
#4271 = ORIENTED_EDGE ( 'NONE', *, *, #43186, .T. ) ;
#4272 = EDGE_CURVE ( 'NONE', #25200, #36052, #32274, .T. ) ;
#4273 = LINE ( 'NONE', #35264, #38949 ) ;
#4274 = ORIENTED_EDGE ( 'NONE', *, *, #51035, .T. ) ;
#4275 = VECTOR ( 'NONE', #12336, 39.37007874015748143 ) ;
#4276 = EDGE_LOOP ( 'NONE', ( #9969, #35120, #9857, #37603 ) ) ;
#4277 = PLANE ( 'NONE',  #18462 ) ;
#4278 = EDGE_CURVE ( 'NONE', #21187, #13750, #49402, .T. ) ;
#4279 = CIRCLE ( 'NONE', #39729, 2.165354330708661568 ) ;
#4280 = ORIENTED_EDGE ( 'NONE', *, *, #28499, .T. ) ;
#4281 = VERTEX_POINT ( 'NONE', #47968 ) ;
#4282 = CARTESIAN_POINT ( 'NONE',  ( -2.165354330708661568, 1.673228346456695492, -4.271103535670736336E-20 ) ) ;
#4283 = VERTEX_POINT ( 'NONE', #40009 ) ;
#4284 = CARTESIAN_POINT ( 'NONE',  ( -2.165354330708661568, 1.673228346456695492, -4.271103535670736336E-20 ) ) ;
#4285 = CARTESIAN_POINT ( 'NONE',  ( -0.2042174104418111591, 2.755905511811024056, -0.3133417129078099328 ) ) ;
#4286 = CARTESIAN_POINT ( 'NONE',  ( -2.951990591674674480, 5.905511811023623991, -0.08331184815402592481 ) ) ;
#4287 = EDGE_CURVE ( 'NONE', #48480, #42546, #5668, .T. ) ;
#4288 = CARTESIAN_POINT ( 'NONE',  ( 1.363819533518803251, 3.346456692913386100, 0.5905511811023579360 ) ) ;
#4289 = ADVANCED_FACE ( 'NONE', ( #47709 ), #12385, .F. ) ;
#4290 = EDGE_CURVE ( 'NONE', #34106, #45399, #24522, .T. ) ;
#4291 = CARTESIAN_POINT ( 'NONE',  ( -0.5455270741695672498, 1.205361022782829114E-17, -1.791688814994948808 ) ) ;
#4292 = LINE ( 'NONE', #12814, #7235 ) ;
#4293 = VERTEX_POINT ( 'NONE', #17793 ) ;
#4294 = CARTESIAN_POINT ( 'NONE',  ( 1.236813753895252166, 1.487789312410982445, -2.681693691597563767 ) ) ;
#4295 = DIRECTION ( 'NONE',  ( -3.469446951953613696E-16, 0.000000000000000000, -1.000000000000000000 ) ) ;
#4296 = LINE ( 'NONE', #7914, #41342 ) ;
#4297 = ORIENTED_EDGE ( 'NONE', *, *, #48309, .T. ) ;
#4298 = VECTOR ( 'NONE', #15008, 39.37007874015748143 ) ;
#4299 = LINE ( 'NONE', #12046, #4233 ) ;
#4300 = LINE ( 'NONE', #36829, #45881 ) ;
#4301 = ORIENTED_EDGE ( 'NONE', *, *, #12217, .T. ) ;
#4302 = DIRECTION ( 'NONE',  ( 0.000000000000000000, -1.000000000000000000, 0.000000000000000000 ) ) ;
#4303 = CARTESIAN_POINT ( 'NONE',  ( -0.8942052331142552601, 3.346456692913386100, -1.771653543307081025 ) ) ;
#4304 = FACE_OUTER_BOUND ( 'NONE', #8787, .T. ) ;
#4305 = VECTOR ( 'NONE', #2300, 39.37007874015748143 ) ;
#4306 = AXIS2_PLACEMENT_3D ( 'NONE', #10504, #14882, #42495 ) ;
#4307 = DIRECTION ( 'NONE',  ( 1.734723475976806848E-16, -0.000000000000000000, 1.000000000000000000 ) ) ;
#4308 = VERTEX_POINT ( 'NONE', #41544 ) ;
#4309 = CARTESIAN_POINT ( 'NONE',  ( -0.2727639067037610499, 3.346456692913386100, -2.047244094488181343 ) ) ;
#4310 = DIRECTION ( 'NONE',  ( -3.469446951953613696E-16, 0.000000000000000000, -1.000000000000000000 ) ) ;
#4311 = VECTOR ( 'NONE', #35045, 39.37007874015748143 ) ;
#4312 = CARTESIAN_POINT ( 'NONE',  ( 1.636583440222563857, 3.267716535433071279, -0.1968503937007886062 ) ) ;
#4313 = CARTESIAN_POINT ( 'NONE',  ( 2.531258147843939089E-16, 2.755905511811023612, 2.066929133858268042 ) ) ;
#4314 = ORIENTED_EDGE ( 'NONE', *, *, #26071, .F. ) ;
#4315 = B_SPLINE_CURVE_WITH_KNOTS ( 'NONE', 3,
 ( #32011, #31244, #4637, #23228 ),
 .UNSPECIFIED., .F., .F.,
 ( 4, 4 ),
 ( 0.001317995325350678881, 0.003818249576796051148 ),
 .UNSPECIFIED. ) ;
#4316 = EDGE_CURVE ( 'NONE', #23504, #9482, #14171, .T. ) ;
#4317 = VERTEX_POINT ( 'NONE', #21670 ) ;
#4318 = ORIENTED_EDGE ( 'NONE', *, *, #44772, .F. ) ;
#4319 = LINE ( 'NONE', #16456, #3149 ) ;
#4320 = ORIENTED_EDGE ( 'NONE', *, *, #48554, .T. ) ;
#4321 = DIRECTION ( 'NONE',  ( 1.000000000000000000, 0.000000000000000000, 0.000000000000000000 ) ) ;
#4322 = ORIENTED_EDGE ( 'NONE', *, *, #40942, .F. ) ;
#4323 = ADVANCED_FACE ( 'NONE', ( #46151 ), #49748, .F. ) ;
#4324 = LINE ( 'NONE', #34808, #5829 ) ;
#4325 = ADVANCED_FACE ( 'NONE', ( #38193 ), #18564, .F. ) ;
#4326 = VERTEX_POINT ( 'NONE', #6177 ) ;
#4327 = CARTESIAN_POINT ( 'NONE',  ( -1.798122294034776969, 1.683198194172631279, -1.651094407303121070 ) ) ;
#4328 = EDGE_CURVE ( 'NONE', #3209, #26202, #6434, .T. ) ;
#4329 = CARTESIAN_POINT ( 'NONE',  ( -0.3542690518128642219, 0.000000000000000000, 1.859817525206697075 ) ) ;
#4330 = EDGE_LOOP ( 'NONE', ( #34319, #32586, #45334 ) ) ;
#4331 = FACE_OUTER_BOUND ( 'NONE', #8715, .T. ) ;
#4332 = ORIENTED_EDGE ( 'NONE', *, *, #28935, .F. ) ;
#4333 = VECTOR ( 'NONE', #34072, 39.37007874015748143 ) ;
#4334 = CARTESIAN_POINT ( 'NONE',  ( 0.3303541855028671037, 0.3937007874015748254, -1.220472440944881942 ) ) ;
#4335 = ORIENTED_EDGE ( 'NONE', *, *, #50061, .T. ) ;
#4336 = ORIENTED_EDGE ( 'NONE', *, *, #14243, .F. ) ;
#4337 = EDGE_CURVE ( 'NONE', #47004, #2534, #9600, .T. ) ;
#4338 = CARTESIAN_POINT ( 'NONE',  ( 0.8182917201112824834, 3.346456692913386100, 1.417322834645662777 ) ) ;
#4339 = AXIS2_PLACEMENT_3D ( 'NONE', #24969, #32739, #47911 ) ;
#4340 = DIRECTION ( 'NONE',  ( -3.469446951953613696E-16, 0.000000000000000000, -1.000000000000000000 ) ) ;
#4341 = ORIENTED_EDGE ( 'NONE', *, *, #32965, .F. ) ;
#4342 = VECTOR ( 'NONE', #44875, 39.37007874015748143 ) ;
#4343 = CARTESIAN_POINT ( 'NONE',  ( 2.889674983507178219, 1.764288196056212454, -0.6090712660037608250 ) ) ;
#4344 = EDGE_LOOP ( 'NONE', ( #44004, #46277, #43108, #24705 ) ) ;
#4345 = LINE ( 'NONE', #4861, #13673 ) ;
#4346 = VECTOR ( 'NONE', #18651, 39.37007874015748143 ) ;
#4347 = EDGE_CURVE ( 'NONE', #45218, #45413, #37172, .T. ) ;
#4348 = VECTOR ( 'NONE', #799, 39.37007874015748143 ) ;
#4349 = DIRECTION ( 'NONE',  ( -1.000000000000000000, 0.000000000000000000, 0.000000000000000000 ) ) ;
#4351 = EDGE_CURVE ( 'NONE', #21756, #17988, #1788, .T. ) ;
#4350 = CYLINDRICAL_SURFACE ( 'NONE', #16507, 2.066929133858268042 ) ;
#4352 = B_SPLINE_CURVE_WITH_KNOTS ( 'NONE', 3,
 ( #2917, #46499, #15989, #25898 ),
 .UNSPECIFIED., .F., .F.,
 ( 4, 4 ),
 ( 2.396517271797282383E-07, 0.002500331769455057130 ),
 .UNSPECIFIED. ) ;
#4353 = EDGE_CURVE ( 'NONE', #24511, #32825, #25536, .T. ) ;
#4354 = VERTEX_POINT ( 'NONE', #14431 ) ;
#4355 = EDGE_LOOP ( 'NONE', ( #10570, #34602, #20342, #27729 ) ) ;
#4356 = CARTESIAN_POINT ( 'NONE',  ( -1.636583440222563635, 3.346456692913386100, -4.780733988912460139E-16 ) ) ;
#4357 = CARTESIAN_POINT ( 'NONE',  ( 2.339241080213585899, 5.905511811023623991, 1.802537235681918037 ) ) ;
#4358 = ADVANCED_FACE ( 'NONE', ( #10804 ), #45640, .F. ) ;
#4359 = EDGE_CURVE ( 'NONE', #358, #46032, #22182, .T. ) ;
#4360 = CARTESIAN_POINT ( 'NONE',  ( -1.909347346926324462, 3.346456692913386100, 0.5905511811023582691 ) ) ;
#4361 = DIRECTION ( 'NONE',  ( -1.000000000000000000, -0.000000000000000000, -0.000000000000000000 ) ) ;
#4362 = DIRECTION ( 'NONE',  ( 1.000000000000000000, 0.000000000000000000, -3.469446951953613696E-16 ) ) ;
#4363 = DIRECTION ( 'NONE',  ( 0.000000000000000000, 0.000000000000000000, -1.000000000000000000 ) ) ;
#4364 = ORIENTED_EDGE ( 'NONE', *, *, #18295, .F. ) ;
#4365 = DIRECTION ( 'NONE',  ( -3.469446951953613696E-16, 0.000000000000000000, -1.000000000000000000 ) ) ;
#4366 = ORIENTED_EDGE ( 'NONE', *, *, #24690, .F. ) ;
#4367 = CARTESIAN_POINT ( 'NONE',  ( 0.1968503937007871074, 3.267716535433071279, -6.829619984160646953E-17 ) ) ;
#4368 = ORIENTED_EDGE ( 'NONE', *, *, #1328, .F. ) ;
#4369 = DIRECTION ( 'NONE',  ( -3.469446951953613696E-16, 0.000000000000000000, -1.000000000000000000 ) ) ;
#4370 = CARTESIAN_POINT ( 'NONE',  ( -1.363819533518803473, 0.000000000000000000, 1.732283464566920950 ) ) ;
#4371 = LINE ( 'NONE', #757, #10281 ) ;
#4372 = VERTEX_POINT ( 'NONE', #14686 ) ;
#4373 = VECTOR ( 'NONE', #25167, 39.37007874015748143 ) ;
#4374 = LINE ( 'NONE', #19597, #13087 ) ;
#4375 = ORIENTED_EDGE ( 'NONE', *, *, #18637, .T. ) ;
#4376 = DIRECTION ( 'NONE',  ( 0.000000000000000000, 0.000000000000000000, -1.000000000000000000 ) ) ;
#4377 = ORIENTED_EDGE ( 'NONE', *, *, #11605, .T. ) ;
#4378 = AXIS2_PLACEMENT_3D ( 'NONE', #38212, #45915, #45155 ) ;
#4379 = VECTOR ( 'NONE', #12877, 39.37007874015748143 ) ;
#4380 = DIRECTION ( 'NONE',  ( 0.000000000000000000, -1.000000000000000000, 0.000000000000000000 ) ) ;
#4381 = DIRECTION ( 'NONE',  ( 0.000000000000000000, 1.160734090543304660E-16, -1.000000000000000000 ) ) ;
#4382 = EDGE_CURVE ( 'NONE', #33806, #43121, #37689, .T. ) ;
#4383 = ADVANCED_FACE ( 'NONE', ( #30177 ), #45896, .F. ) ;
#4384 = VECTOR ( 'NONE', #14902, 39.37007874015748143 ) ;
#4385 = CARTESIAN_POINT ( 'NONE',  ( -2.182111253630085734, 0.000000000000000000, -0.9448818897637762948 ) ) ;
#4386 = ORIENTED_EDGE ( 'NONE', *, *, #41782, .T. ) ;
#4387 = ORIENTED_EDGE ( 'NONE', *, *, #35758, .T. ) ;
#4388 = DIRECTION ( 'NONE',  ( -3.469446951953613696E-16, 0.000000000000000000, -1.000000000000000000 ) ) ;
#4389 = DIRECTION ( 'NONE',  ( 1.734723475976806848E-16, -0.000000000000000000, 1.000000000000000000 ) ) ;
#4390 = LINE ( 'NONE', #28899, #14485 ) ;
#4391 = VERTEX_POINT ( 'NONE', #26303 ) ;
#4392 = CARTESIAN_POINT ( 'NONE',  ( -2.867773316779185677, 1.574658946938755522, -0.7050287376752426560 ) ) ;
#4393 = CARTESIAN_POINT ( 'NONE',  ( 1.928732080931637505, 3.267716535433071279, -0.9842519685039348154 ) ) ;
#4394 = ORIENTED_EDGE ( 'NONE', *, *, #48750, .T. ) ;
#4395 = CARTESIAN_POINT ( 'NONE',  ( 0.000000000000000000, 5.118110236220475784, 0.000000000000000000 ) ) ;
#4396 = ORIENTED_EDGE ( 'NONE', *, *, #16620, .F. ) ;
#4397 = ORIENTED_EDGE ( 'NONE', *, *, #36947, .F. ) ;
#4398 = EDGE_CURVE ( 'NONE', #35324, #54, #33561, .T. ) ;
#4399 = PRODUCT_CONTEXT ( 'NONE', #9120, 'mechanical' ) ;
#4400 = ORIENTED_EDGE ( 'NONE', *, *, #31199, .F. ) ;
#4401 = DIRECTION ( 'NONE',  ( 0.000000000000000000, 0.000000000000000000, 1.000000000000000000 ) ) ;
#4402 = CARTESIAN_POINT ( 'NONE',  ( 0.5455278134075208785, 3.346456692913386100, -1.771653543307081025 ) ) ;
#4403 = EDGE_CURVE ( 'NONE', #34006, #2513, #50004, .T. ) ;
#4404 = CARTESIAN_POINT ( 'NONE',  ( 0.2304536187852652684, 1.049866565877818347, -2.011542525805705139 ) ) ;
#4405 = DIRECTION ( 'NONE',  ( -1.000000000000000000, -0.000000000000000000, -1.734839586111147395E-16 ) ) ;
#4406 = EDGE_CURVE ( 'NONE', #26900, #23170, #48960, .T. ) ;
#4407 = ORIENTED_EDGE ( 'NONE', *, *, #5980, .F. ) ;
#4408 = ORIENTED_EDGE ( 'NONE', *, *, #15177, .F. ) ;
#4409 = CARTESIAN_POINT ( 'NONE',  ( -2.138597145901436125, 1.574803149606302854, 0.3393547186366939750 ) ) ;
#4410 = DIRECTION ( 'NONE',  ( 1.000000000000000000, 0.000000000000000000, -3.469446951953613696E-16 ) ) ;
#4411 = EDGE_CURVE ( 'NONE', #2304, #32620, #41296, .T. ) ;
#4412 = CARTESIAN_POINT ( 'NONE',  ( 2.295325967725798222, 1.744665796922353351, 0.3605850800666594580 ) ) ;
#4413 = AXIS2_PLACEMENT_3D ( 'NONE', #10729, #5583, #1966 ) ;
#4414 = ORIENTED_EDGE ( 'NONE', *, *, #4259, .T. ) ;
#4415 = FACE_OUTER_BOUND ( 'NONE', #22786, .T. ) ;
#4416 = AXIS2_PLACEMENT_3D ( 'NONE', #26818, #23709, #34338 ) ;
#4417 = PLANE ( 'NONE',  #34674 ) ;
#4418 = VECTOR ( 'NONE', #6652, 39.37007874015748143 ) ;
#4419 = DIRECTION ( 'NONE',  ( 0.000000000000000000, 0.000000000000000000, -1.000000000000000000 ) ) ;
#4420 = DIRECTION ( 'NONE',  ( 0.000000000000000000, 0.000000000000000000, 1.000000000000000000 ) ) ;
#4421 = DIRECTION ( 'NONE',  ( -0.000000000000000000, 1.000000000000000000, -0.000000000000000000 ) ) ;
#4422 = AXIS2_PLACEMENT_3D ( 'NONE', #26644, #41896, #14782 ) ;
#4423 = ORIENTED_EDGE ( 'NONE', *, *, #26996, .T. ) ;
#4424 = DIRECTION ( 'NONE',  ( 0.9990914673551315461, 0.000000000000000000, -0.04261736568783054679 ) ) ;
#4425 = ORIENTED_EDGE ( 'NONE', *, *, #46859, .F. ) ;
#4426 = ORIENTED_EDGE ( 'NONE', *, *, #20054, .F. ) ;
#4427 = LINE ( 'NONE', #50840, #47126 ) ;
#4428 = CARTESIAN_POINT ( 'NONE',  ( 4.439252989704605840E-17, 3.267716535433071279, -7.700876377040806239E-33 ) ) ;
#4429 = FACE_OUTER_BOUND ( 'NONE', #13558, .T. ) ;
#4430 = EDGE_LOOP ( 'NONE', ( #50784, #19816, #19898, #41367 ) ) ;
#4431 = ORIENTED_EDGE ( 'NONE', *, *, #8411, .T. ) ;
#4432 = DIRECTION ( 'NONE',  ( 0.000000000000000000, 0.000000000000000000, -1.000000000000000000 ) ) ;
#4433 = ORIENTED_EDGE ( 'NONE', *, *, #48477, .F. ) ;
#4434 = CARTESIAN_POINT ( 'NONE',  ( 1.019791434298717325, 0.5230628772194416687, -2.004195265303256868 ) ) ;
#4435 = ORIENTED_EDGE ( 'NONE', *, *, #25989, .F. ) ;
#4436 = CARTESIAN_POINT ( 'NONE',  ( 0.9914495361338625523, 1.636256239573039117, 2.781765111341823360 ) ) ;
#4437 = CARTESIAN_POINT ( 'NONE',  ( 0.6769013455170100890, 1.726104531401197351, -2.637681086482273063 ) ) ;
#4438 = CARTESIAN_POINT ( 'NONE',  ( -0.8182917201112814842, 3.346456692913386100, 1.732283464566921172 ) ) ;
#4439 = ORIENTED_EDGE ( 'NONE', *, *, #9993, .F. ) ;
#4440 = VECTOR ( 'NONE', #46537, 39.37007874015748143 ) ;
#4441 = ADVANCED_FACE ( 'NONE', ( #907 ), #38440, .F. ) ;
#4442 = EDGE_LOOP ( 'NONE', ( #12704, #50473, #29299, #46664 ) ) ;
#4443 = VERTEX_POINT ( 'NONE', #20531 ) ;
#4444 = FACE_OUTER_BOUND ( 'NONE', #11122, .T. ) ;
#4445 = CYLINDRICAL_SURFACE ( 'NONE', #11484, 0.3740157480314960647 ) ;
#4446 = VECTOR ( 'NONE', #5941, 39.37007874015748143 ) ;
#4447 = ADVANCED_FACE ( 'NONE', ( #15882 ), #30683, .F. ) ;
#4448 = B_SPLINE_CURVE_WITH_KNOTS ( 'NONE', 3,
 ( #22263, #38268, #19130, #41626 ),
 .UNSPECIFIED., .F., .F.,
 ( 4, 4 ),
 ( 0.1211873102087489551, 0.1625992483279400380 ),
 .UNSPECIFIED. ) ;
#4449 = EDGE_LOOP ( 'NONE', ( #19705, #22223, #42604, #15059 ) ) ;
#4450 = VERTEX_POINT ( 'NONE', #27752 ) ;
#4451 = VECTOR ( 'NONE', #44869, 39.37007874015748143 ) ;
#4452 = DIRECTION ( 'NONE',  ( 1.000000000000000000, 0.000000000000000000, -3.469446951953613696E-16 ) ) ;
#4453 = DIRECTION ( 'NONE',  ( -0.000000000000000000, 1.000000000000000000, -0.000000000000000000 ) ) ;
#4454 = FACE_OUTER_BOUND ( 'NONE', #12224, .T. ) ;
#4455 = EDGE_CURVE ( 'NONE', #7592, #728, #20000, .T. ) ;
#4456 = VECTOR ( 'NONE', #24118, 39.37007874015748143 ) ;
#4457 = VECTOR ( 'NONE', #19142, 39.37007874015748143 ) ;
#4458 = VERTEX_POINT ( 'NONE', #20267 ) ;
#4459 = CYLINDRICAL_SURFACE ( 'NONE', #48520, 0.8858267716535433989 ) ;
#4460 = CARTESIAN_POINT ( 'NONE',  ( -0.2727639067037607723, 0.000000000000000000, 2.362204724409437961 ) ) ;
#4461 = LINE ( 'NONE', #39822, #37737 ) ;
#4462 = ORIENTED_EDGE ( 'NONE', *, *, #8893, .T. ) ;
#4463 = CARTESIAN_POINT ( 'NONE',  ( 0.8949303405208896001, 1.574803149606302854, -1.971765468592530102 ) ) ;
#4464 = LINE ( 'NONE', #13239, #511 ) ;
#4465 = VECTOR ( 'NONE', #26834, 39.37007874015748143 ) ;
#4466 = ORIENTED_EDGE ( 'NONE', *, *, #1730, .F. ) ;
#4467 = CARTESIAN_POINT ( 'NONE',  ( 2.069752515245542046, 1.205361022782829114E-17, -0.5228856972975560735 ) ) ;
#4468 = ORIENTED_EDGE ( 'NONE', *, *, #29204, .F. ) ;
#4469 = ORIENTED_EDGE ( 'NONE', *, *, #16035, .T. ) ;
#4470 = CARTESIAN_POINT ( 'NONE',  ( 0.000000000000000000, 3.267716535433071279, 0.000000000000000000 ) ) ;
#4471 =( NAMED_UNIT ( * ) SI_UNIT ( $, .STERADIAN. ) SOLID_ANGLE_UNIT ( ) );
#4472 = CARTESIAN_POINT ( 'NONE',  ( -0.07591351300297363713, 3.346456692913386100, -2.164023224473873963 ) ) ;
#4473 = EDGE_CURVE ( 'NONE', #30518, #49043, #35765, .T. ) ;
#4474 = CARTESIAN_POINT ( 'NONE',  ( -0.4120130461783780840, 1.024878400823626245, 2.545991998580761084 ) ) ;
#4475 = CARTESIAN_POINT ( 'NONE',  ( -1.775400203342670347, 1.552775173289138166, -2.359903268218729089 ) ) ;
#4476 = ORIENTED_EDGE ( 'NONE', *, *, #30434, .F. ) ;
#4477 = EDGE_LOOP ( 'NONE', ( #27767, #31917, #9478, #40036 ) ) ;
#4478 = EDGE_CURVE ( 'NONE', #15500, #596, #47339, .T. ) ;
#4479 = ORIENTED_EDGE ( 'NONE', *, *, #40507, .T. ) ;
#4480 = DIRECTION ( 'NONE',  ( -3.469446951953613696E-16, 0.000000000000000000, -1.000000000000000000 ) ) ;
#4481 = CARTESIAN_POINT ( 'NONE',  ( 0.1067246931122726866, 0.02962905676920215767, 0.000000000000000000 ) ) ;
#4482 = CARTESIAN_POINT ( 'NONE',  ( 1.909347346926324684, 3.346456692913386100, 0.7874015748031456541 ) ) ;
#4483 =( GEOMETRIC_REPRESENTATION_CONTEXT ( 3 ) GLOBAL_UNCERTAINTY_ASSIGNED_CONTEXT ( ( #21565 ) ) GLOBAL_UNIT_ASSIGNED_CONTEXT ( ( #25362, #33386, #6515 ) ) REPRESENTATION_CONTEXT ( 'NONE', 'WORKASPACE' ) );
#4484 = DIRECTION ( 'NONE',  ( 1.558091277195270436E-17, -1.000000000000000000, -1.150229170499806500E-16 ) ) ;
#4485 = CARTESIAN_POINT ( 'NONE',  ( 2.623503965249849301, 1.760141956857387724, 1.355882097269874187 ) ) ;
#4486 = ORIENTED_EDGE ( 'NONE', *, *, #7459, .T. ) ;
#4487 = VECTOR ( 'NONE', #37585, 39.37007874015748143 ) ;
#4488 = DIRECTION ( 'NONE',  ( -3.469446951953613696E-16, 0.000000000000000000, -1.000000000000000000 ) ) ;
#4489 = AXIS2_PLACEMENT_3D ( 'NONE', #45316, #2490, #34239 ) ;
#4490 = EDGE_CURVE ( 'NONE', #16195, #8210, #17843, .T. ) ;
#4491 = LINE ( 'NONE', #16628, #24045 ) ;
#4492 = VECTOR ( 'NONE', #26532, 39.37007874015748854 ) ;
#4493 = VECTOR ( 'NONE', #36064, 39.37007874015748143 ) ;
#4494 = VERTEX_POINT ( 'NONE', #8145 ) ;
#4495 = CARTESIAN_POINT ( 'NONE',  ( 3.927031490892378253E-16, 0.000000000000000000, 0.7480314960629874665 ) ) ;
#4496 = FACE_OUTER_BOUND ( 'NONE', #49725, .T. ) ;
#4497 = CARTESIAN_POINT ( 'NONE',  ( 1.929629134066521701, 2.755905511811027164, 0.9824921284572420976 ) ) ;
#4498 = VERTEX_POINT ( 'NONE', #44008 ) ;
#4499 = CARTESIAN_POINT ( 'NONE',  ( -1.775400203342670347, 1.552775173289138166, -2.359903268218729089 ) ) ;
#4500 = CARTESIAN_POINT ( 'NONE',  ( 0.7423782071083090406, 3.267716535433071279, -2.575641807848711180E-16 ) ) ;
#4501 = CARTESIAN_POINT ( 'NONE',  ( -0.1516866087075746383, 1.607047215343822222, -2.234383150555500297 ) ) ;
#4502 = ORIENTED_EDGE ( 'NONE', *, *, #17563, .F. ) ;
#4503 = DIRECTION ( 'NONE',  ( -3.469446951953613696E-16, 0.000000000000000000, -1.000000000000000000 ) ) ;
#4504 = CARTESIAN_POINT ( 'NONE',  ( 0.000000000000000000, 3.267716535433071279, -0.9448818897637760728 ) ) ;
#4505 = ORIENTED_EDGE ( 'NONE', *, *, #49246, .T. ) ;
#4506 = CARTESIAN_POINT ( 'NONE',  ( 0.7148041136150538044, 5.905511811023623991, -2.044646019095610168 ) ) ;
#4507 = DIRECTION ( 'NONE',  ( 0.000000000000000000, 0.000000000000000000, -1.000000000000000000 ) ) ;
#4508 = DIRECTION ( 'NONE',  ( 1.000000000000000000, 0.000000000000000000, -3.469446951953613696E-16 ) ) ;
#4509 = DIRECTION ( 'NONE',  ( -0.01601477604151182663, 0.9998717552508123996, -0.000000000000000000 ) ) ;
#4510 = ORIENTED_EDGE ( 'NONE', *, *, #32632, .T. ) ;
#4511 = ORIENTED_EDGE ( 'NONE', *, *, #25455, .F. ) ;
#4512 = CARTESIAN_POINT ( 'NONE',  ( -0.8182917201112819283, 3.346456692913386100, -1.929133858267710000 ) ) ;
#4513 = DIRECTION ( 'NONE',  ( 0.000000000000000000, 0.000000000000000000, -1.000000000000000000 ) ) ;
#4514 = ADVANCED_FACE ( 'NONE', ( #38691 ), #1607, .T. ) ;
#4515 = ORIENTED_EDGE ( 'NONE', *, *, #23402, .F. ) ;
#4516 = DIRECTION ( 'NONE',  ( -0.000000000000000000, 0.000000000000000000, 1.000000000000000000 ) ) ;
#4517 = LINE ( 'NONE', #645, #39232 ) ;
#4518 = LINE ( 'NONE', #40657, #19517 ) ;
#4519 = EDGE_CURVE ( 'NONE', #22792, #29967, #23891, .T. ) ;
#4520 = DIRECTION ( 'NONE',  ( -0.000000000000000000, 1.000000000000000000, -0.000000000000000000 ) ) ;
#4521 = VERTEX_POINT ( 'NONE', #39637 ) ;
#4522 = VERTEX_POINT ( 'NONE', #3311 ) ;
#4523 = EDGE_CURVE ( 'NONE', #40819, #42, #48622, .T. ) ;
#4524 = LINE ( 'NONE', #48616, #32893 ) ;
#4525 = DIRECTION ( 'NONE',  ( -0.000000000000000000, 1.000000000000000000, -0.000000000000000000 ) ) ;
#4526 = DIRECTION ( 'NONE',  ( -0.000000000000000000, 1.000000000000000000, -0.000000000000000000 ) ) ;
#4527 = EDGE_CURVE ( 'NONE', #3556, #19885, #39893, .T. ) ;
#4528 = CARTESIAN_POINT ( 'NONE',  ( -0.8942052331142549271, 3.267716535433071279, 3.102397620449222481E-16 ) ) ;
#4529 = FACE_BOUND ( 'NONE', #20717, .T. ) ;
#4530 = CIRCLE ( 'NONE', #8655, 1.850107469027523432 ) ;
#4531 = VERTEX_POINT ( 'NONE', #24406 ) ;
#4532 = CARTESIAN_POINT ( 'NONE',  ( 0.4696143004045478797, 3.346456692913386100, -1.299212598425193210 ) ) ;
#4533 = VECTOR ( 'NONE', #47486, 39.37007874015748143 ) ;
#4534 = VERTEX_POINT ( 'NONE', #12788 ) ;
#4535 = ORIENTED_EDGE ( 'NONE', *, *, #51038, .F. ) ;
#4536 = DIRECTION ( 'NONE',  ( -0.000000000000000000, -1.000000000000000000, -0.000000000000000000 ) ) ;
#4537 = AXIS2_PLACEMENT_3D ( 'NONE', #10986, #31371, #47064 ) ;
#4538 = EDGE_CURVE ( 'NONE', #44975, #13922, #36030, .T. ) ;
#4539 = EDGE_LOOP ( 'NONE', ( #649, #30828, #44912, #45581 ) ) ;
#4540 = ORIENTED_EDGE ( 'NONE', *, *, #42347, .F. ) ;
#4541 = DIRECTION ( 'NONE',  ( 1.734723475976806848E-16, 0.000000000000000000, 1.000000000000000000 ) ) ;
#4542 = VERTEX_POINT ( 'NONE', #7197 ) ;
#4543 = VECTOR ( 'NONE', #5428, 39.37007874015748143 ) ;
#4544 = EDGE_CURVE ( 'NONE', #46747, #30154, #32161, .T. ) ;
#4545 = FACE_OUTER_BOUND ( 'NONE', #36474, .T. ) ;
#4546 = DIRECTION ( 'NONE',  ( 0.000000000000000000, 0.000000000000000000, 1.000000000000000000 ) ) ;
#4547 = FACE_OUTER_BOUND ( 'NONE', #15560, .T. ) ;
#4548 = EDGE_CURVE ( 'NONE', #38358, #19280, #50250, .T. ) ;
#4549 = LINE ( 'NONE', #151, #6635 ) ;
#4550 = CARTESIAN_POINT ( 'NONE',  ( 1.636583440222563857, 0.000000000000000000, -1.161035397307311917E-15 ) ) ;
#4551 = CARTESIAN_POINT ( 'NONE',  ( 0.2727639067037604947, 3.346456692913386100, -0.4724409448818886470 ) ) ;
#4552 = ORIENTED_EDGE ( 'NONE', *, *, #49393, .F. ) ;
#4553 = LINE ( 'NONE', #40183, #20037 ) ;
#4554 = SURFACE_STYLE_USAGE ( .BOTH. , #26147 ) ;
#4555 = EDGE_CURVE ( 'NONE', #13306, #41806, #11066, .T. ) ;
#4556 = PLANE ( 'NONE',  #31462 ) ;
#4557 = VERTEX_POINT ( 'NONE', #22936 ) ;
#4558 = CARTESIAN_POINT ( 'NONE',  ( 1.219594629708742994, 0.01552060224298149917, -1.594902525371822533 ) ) ;
#4559 = CARTESIAN_POINT ( 'NONE',  ( -1.733853452330418987, 0.0001488292986583184614, 0.1852043564780690432 ) ) ;
#4560 = VERTEX_POINT ( 'NONE', #19053 ) ;
#4561 = CARTESIAN_POINT ( 'NONE',  ( 0.000000000000000000, 0.000000000000000000, 0.000000000000000000 ) ) ;
#4562 = LINE ( 'NONE', #9200, #33372 ) ;
#4563 = CARTESIAN_POINT ( 'NONE',  ( 1.084824920504545324E-16, 2.755905511811023612, 0.8858267716535433989 ) ) ;
#4564 = VECTOR ( 'NONE', #12878, 39.37007874015748143 ) ;
#4565 = CIRCLE ( 'NONE', #40828, 2.165354330708661568 ) ;
#4566 = ADVANCED_FACE ( 'NONE', ( #35511 ), #48618, .T. ) ;
#4567 = AXIS2_PLACEMENT_3D ( 'NONE', #49464, #29644, #44857 ) ;
#4568 = ORIENTED_EDGE ( 'NONE', *, *, #4999, .T. ) ;
#4569 = CARTESIAN_POINT ( 'NONE',  ( 2.164658444855302122, 5.905511811023623991, -0.04795272066889885720 ) ) ;
#4570 = ORIENTED_EDGE ( 'NONE', *, *, #38283, .F. ) ;
#4571 = CARTESIAN_POINT ( 'NONE',  ( 0.8182917201112819283, 0.000000000000000000, 0.2755905511810994302 ) ) ;
#4572 = AXIS2_PLACEMENT_3D ( 'NONE', #34111, #42602, #37986 ) ;
#4573 = CARTESIAN_POINT ( 'NONE',  ( 1.636583440222563857, 0.000000000000000000, -0.6299212598425181220 ) ) ;
#4574 = LINE ( 'NONE', #700, #30081 ) ;
#4575 = CARTESIAN_POINT ( 'NONE',  ( -0.6214413264104945434, 3.267716535433071279, 1.850393700787391849 ) ) ;
#4576 = VECTOR ( 'NONE', #46325, 39.37007874015748143 ) ;
#4577 = ORIENTED_EDGE ( 'NONE', *, *, #20236, .T. ) ;
#4578 = ORIENTED_EDGE ( 'NONE', *, *, #47765, .T. ) ;
#4579 = LINE ( 'NONE', #43290, #41928 ) ;
#4580 = ORIENTED_EDGE ( 'NONE', *, *, #16038, .F. ) ;
#4581 = CARTESIAN_POINT ( 'NONE',  ( 2.926032761125787029, 5.905511811023623991, 0.3963580683592528575 ) ) ;
#4582 = VERTEX_POINT ( 'NONE', #45269 ) ;
#4583 = EDGE_CURVE ( 'NONE', #21352, #2302, #17931, .T. ) ;
#4584 = CARTESIAN_POINT ( 'NONE',  ( 2.141071258218635531, 0.000000000000000000, -0.04689341889560144638 ) ) ;
#4585 = ORIENTED_EDGE ( 'NONE', *, *, #34516, .F. ) ;
#4586 = CARTESIAN_POINT ( 'NONE',  ( 2.255357468390372322, 1.645600431408117847, -0.5652488166673508285 ) ) ;
#4587 = EDGE_CURVE ( 'NONE', #30787, #38385, #5800, .T. ) ;
#4588 = DIRECTION ( 'NONE',  ( 1.734723475976806848E-16, -0.000000000000000000, 1.000000000000000000 ) ) ;
#4589 = ORIENTED_EDGE ( 'NONE', *, *, #11000, .T. ) ;
#4590 = FACE_OUTER_BOUND ( 'NONE', #18175, .T. ) ;
#4591 = ORIENTED_EDGE ( 'NONE', *, *, #30071, .F. ) ;
#4592 = LINE ( 'NONE', #50141, #38621 ) ;
#4593 = ORIENTED_EDGE ( 'NONE', *, *, #12916, .T. ) ;
#4594 = VERTEX_POINT ( 'NONE', #13300 ) ;
#4595 = DIRECTION ( 'NONE',  ( 0.000000000000000000, 1.000000000000000000, 0.000000000000000000 ) ) ;
#4596 = CARTESIAN_POINT ( 'NONE',  ( 0.4696143004045484903, 3.346456692913386100, 1.417322834645662777 ) ) ;
#4597 = AXIS2_PLACEMENT_3D ( 'NONE', #29691, #26321, #5692 ) ;
#4598 = ORIENTED_EDGE ( 'NONE', *, *, #28757, .T. ) ;
#4599 = FACE_OUTER_BOUND ( 'NONE', #24311, .T. ) ;
#4600 = VECTOR ( 'NONE', #49680, 39.37007874015748143 ) ;
#4601 = ORIENTED_EDGE ( 'NONE', *, *, #1670, .F. ) ;
#4602 = CARTESIAN_POINT ( 'NONE',  ( -0.2727639067037608278, 3.267716535433071279, -1.929133858267710000 ) ) ;
#4603 = DIRECTION ( 'NONE',  ( -0.000000000000000000, 1.000000000000000000, -0.000000000000000000 ) ) ;
#4604 = AXIS2_PLACEMENT_3D ( 'NONE', #11127, #7257, #38750 ) ;
#4605 = EDGE_CURVE ( 'NONE', #47393, #3807, #9678, .T. ) ;
#4606 = CARTESIAN_POINT ( 'NONE',  ( -0.2431224069213033800, 1.205361022782829114E-17, 2.152304290637669926 ) ) ;
#4607 = ORIENTED_EDGE ( 'NONE', *, *, #50282, .F. ) ;
#4608 = ORIENTED_EDGE ( 'NONE', *, *, #1514, .F. ) ;
#4609 = CONICAL_SURFACE ( 'NONE', #47425, 2.246510896728926010, 0.01601546068027819014 ) ;
#4610 = DIRECTION ( 'NONE',  ( 0.000000000000000000, -1.000000000000000000, 0.000000000000000000 ) ) ;
#4611 = LINE ( 'NONE', #12875, #33601 ) ;
#4612 = LINE ( 'NONE', #24492, #38981 ) ;
#4613 = CARTESIAN_POINT ( 'NONE',  ( 0.000000000000000000, 3.267716535433071279, 1.102362204724404160 ) ) ;
#4614 = EDGE_CURVE ( 'NONE', #45913, #41125, #1418, .T. ) ;
#4615 = CARTESIAN_POINT ( 'NONE',  ( 0.4518890234970225350, 1.682331384353711101, 2.214500778602899178 ) ) ;
#4616 = EDGE_CURVE ( 'NONE', #767, #37842, #48561, .T. ) ;
#4617 = DIRECTION ( 'NONE',  ( -0.000000000000000000, 1.000000000000000000, -0.000000000000000000 ) ) ;
#4618 = ORIENTED_EDGE ( 'NONE', *, *, #42271, .F. ) ;
#4619 = EDGE_CURVE ( 'NONE', #38729, #35081, #5547, .T. ) ;
#4620 = CARTESIAN_POINT ( 'NONE',  ( -1.014069264286641570, 0.4724409448818898127, 1.014069264286641570 ) ) ;
#4621 = ORIENTED_EDGE ( 'NONE', *, *, #6100, .F. ) ;
#4622 = CARTESIAN_POINT ( 'NONE',  ( 0.7521025634872258170, 1.621523052975431867, 2.144027383376515328 ) ) ;
#4623 = EDGE_CURVE ( 'NONE', #16455, #42424, #29289, .T. ) ;
#4624 = ORIENTED_EDGE ( 'NONE', *, *, #17940, .T. ) ;
#4625 = ADVANCED_FACE ( 'NONE', ( #1929 ), #32939, .F. ) ;
#4626 = CARTESIAN_POINT ( 'NONE',  ( 0.4696143004045484903, 3.346456692913386100, 1.732283464566921172 ) ) ;
#4627 = LINE ( 'NONE', #31239, #44315 ) ;
#4628 = DIRECTION ( 'NONE',  ( 5.779879058770898378E-18, 1.000000000000000000, 1.286990067732318227E-16 ) ) ;
#4629 = CARTESIAN_POINT ( 'NONE',  ( -1.779568955232874394, 6.692913385826772199, -1.233650562797313999 ) ) ;
#4630 = EDGE_LOOP ( 'NONE', ( #49682, #44069, #5586, #18424 ) ) ;
#4631 = AXIS2_PLACEMENT_3D ( 'NONE', #32636, #25376, #40624 ) ;
#4632 = DIRECTION ( 'NONE',  ( -3.986037398843765983E-20, -1.000000000000000000, -1.160734090543304660E-16 ) ) ;
#4633 = VECTOR ( 'NONE', #42318, 39.37007874015748143 ) ;
#4634 = FACE_BOUND ( 'NONE', #1357, .T. ) ;
#4635 = CIRCLE ( 'NONE', #32708, 2.164630168518208109 ) ;
#4636 = ORIENTED_EDGE ( 'NONE', *, *, #30917, .F. ) ;
#4637 = CARTESIAN_POINT ( 'NONE',  ( -0.9148539695939212901, 1.627632094643381988, -2.013137310660124690 ) ) ;
#4638 = AXIS2_PLACEMENT_3D ( 'NONE', #28443, #16589, #23817 ) ;
#4639 = ORIENTED_EDGE ( 'NONE', *, *, #6480, .F. ) ;
#4640 = EDGE_CURVE ( 'NONE', #15732, #49030, #5289, .T. ) ;
#4641 = DIRECTION ( 'NONE',  ( -0.000000000000000000, 1.000000000000000000, -0.000000000000000000 ) ) ;
#4642 = CARTESIAN_POINT ( 'NONE',  ( -1.909347346926324462, 0.000000000000000000, 0.7874015748031456541 ) ) ;
#4643 = VECTOR ( 'NONE', #19186, 39.37007874015748143 ) ;
#4644 = EDGE_CURVE ( 'NONE', #26747, #16466, #21299, .T. ) ;
#4645 = AXIS2_PLACEMENT_3D ( 'NONE', #9981, #38372, #21863 ) ;
#4646 = CARTESIAN_POINT ( 'NONE',  ( 0.2727639067037604947, 3.346456692913386100, -1.417322834645664331 ) ) ;
#4647 = EDGE_CURVE ( 'NONE', #12127, #31145, #37309, .T. ) ;
#4648 = ORIENTED_EDGE ( 'NONE', *, *, #11157, .T. ) ;
#4649 = ORIENTED_EDGE ( 'NONE', *, *, #42333, .F. ) ;
#4650 = CARTESIAN_POINT ( 'NONE',  ( -1.091055626815042645, 3.267716535433071279, 1.892679809432644882E-16 ) ) ;
#4651 = CARTESIAN_POINT ( 'NONE',  ( 1.062992125984251413, 0.5905511811023621549, 1.062992125984251413 ) ) ;
#4652 = FACE_BOUND ( 'NONE', #16284, .T. ) ;
#4653 = PLANE ( 'NONE',  #8051 ) ;
#4654 = DIRECTION ( 'NONE',  ( 1.000000000000000000, 0.000000000000000000, -3.469446951953613696E-16 ) ) ;
#4655 = ORIENTED_EDGE ( 'NONE', *, *, #41993, .T. ) ;
#4656 = LINE ( 'NONE', #4910, #38145 ) ;
#4657 = VERTEX_POINT ( 'NONE', #14056 ) ;
#4658 = EDGE_LOOP ( 'NONE', ( #23084, #488, #50548, #21795 ) ) ;
#4659 = APPLICATION_PROTOCOL_DEFINITION ( 'draft international standard', 'automotive_design', 1998, #26605 ) ;
#4660 = ORIENTED_EDGE ( 'NONE', *, *, #5059, .F. ) ;
#4661 = LINE ( 'NONE', #44651, #33418 ) ;
#4662 = LINE ( 'NONE', #40805, #3571 ) ;
#4664 = CARTESIAN_POINT ( 'NONE',  ( 1.769879628650530723, 0.05626752682809384870, -0.8100022834900426627 ) ) ;
#4663 = CONICAL_SURFACE ( 'NONE', #31052, 2.165354330708661568, 0.2617993877991570129 ) ;
#4665 = CARTESIAN_POINT ( 'NONE',  ( 0.000000000000000000, 6.692913385826772199, 0.000000000000000000 ) ) ;
#4666 = EDGE_LOOP ( 'NONE', ( #6025, #42875, #14834, #956, #15069 ) ) ;
#4667 = ORIENTED_EDGE ( 'NONE', *, *, #26158, .T. ) ;
#4669 = VECTOR ( 'NONE', #35092, 39.37007874015748854 ) ;
#4668 = CARTESIAN_POINT ( 'NONE',  ( 1.473258485933809592, 1.698690484189727901, 1.761078168145147727 ) ) ;
#4670 = CARTESIAN_POINT ( 'NONE',  ( -0.7874015748031496509, 1.172985819482486924, -0.9842519685039370358 ) ) ;
#4671 = VECTOR ( 'NONE', #41444, 39.37007874015748143 ) ;
#4672 = DIRECTION ( 'NONE',  ( -0.000000000000000000, 1.000000000000000000, -0.000000000000000000 ) ) ;
#4673 = CARTESIAN_POINT ( 'NONE',  ( -1.166969139818015977, 3.346456692913386100, 2.047244094488179567 ) ) ;
#4674 = DIRECTION ( 'NONE',  ( 3.986037398843765983E-20, 1.000000000000000000, 1.160734090543304660E-16 ) ) ;
#4675 = EDGE_CURVE ( 'NONE', #14034, #20924, #25252, .T. ) ;
#4676 = LINE ( 'NONE', #31095, #28393 ) ;
#4677 = VECTOR ( 'NONE', #16158, 39.37007874015748143 ) ;
#4678 = EDGE_CURVE ( 'NONE', #40155, #17243, #9423, .T. ) ;
#4679 = CARTESIAN_POINT ( 'NONE',  ( 0.000000000000000000, 5.905511811023623991, 0.000000000000000000 ) ) ;
#4680 = EDGE_CURVE ( 'NONE', #12101, #48279, #35122, .T. ) ;
#4681 = DIRECTION ( 'NONE',  ( -0.000000000000000000, 1.000000000000000000, -0.000000000000000000 ) ) ;
#4682 = VECTOR ( 'NONE', #21803, 39.37007874015748143 ) ;
#4683 = ORIENTED_EDGE ( 'NONE', *, *, #28707, .T. ) ;
#4684 = LINE ( 'NONE', #23523, #332 ) ;
#4685 =( LENGTH_UNIT ( ) NAMED_UNIT ( * ) SI_UNIT ( $, .METRE. ) );
#4686 = EDGE_LOOP ( 'NONE', ( #18293, #28561, #25726, #19918 ) ) ;
#4687 = ORIENTED_EDGE ( 'NONE', *, *, #20066, .T. ) ;
#4688 = DIRECTION ( 'NONE',  ( 1.734723475976806848E-16, -0.000000000000000000, 1.000000000000000000 ) ) ;
#4689 = DIRECTION ( 'NONE',  ( 0.6910626489868684219, 8.386971787576741778E-17, -0.7227948638273878901 ) ) ;
#4690 = CARTESIAN_POINT ( 'NONE',  ( 0.000000000000000000, 6.692913385826772199, 0.000000000000000000 ) ) ;
#4691 = ORIENTED_EDGE ( 'NONE', *, *, #27332, .T. ) ;
#4692 = ORIENTED_EDGE ( 'NONE', *, *, #5980, .T. ) ;
#4693 = DIRECTION ( 'NONE',  ( 0.000000000000000000, -1.000000000000000000, 0.000000000000000000 ) ) ;
#4695 = ORIENTED_EDGE ( 'NONE', *, *, #29732, .F. ) ;
#4694 = EDGE_CURVE ( 'NONE', #39809, #45998, #24664, .T. ) ;
#4696 = CARTESIAN_POINT ( 'NONE',  ( 1.636583440222563857, 3.346456692913386100, 0.9448818897637746295 ) ) ;
#4697 = VERTEX_POINT ( 'NONE', #48362 ) ;
#4698 = FACE_OUTER_BOUND ( 'NONE', #48020, .T. ) ;
#4699 = EDGE_CURVE ( 'NONE', #33287, #23952, #39360, .T. ) ;
#4700 = CARTESIAN_POINT ( 'NONE',  ( -2.325586279745288643, 1.674843395074420149, 0.7038835993775438560 ) ) ;
#4701 = DIRECTION ( 'NONE',  ( -3.469446951953613696E-16, 0.000000000000000000, -1.000000000000000000 ) ) ;
#4702 = VECTOR ( 'NONE', #48332, 39.37007874015748143 ) ;
#4703 = EDGE_CURVE ( 'NONE', #13831, #26074, #2185, .T. ) ;
#4704 = ORIENTED_EDGE ( 'NONE', *, *, #3327, .F. ) ;
#4705 = EDGE_LOOP ( 'NONE', ( #23065, #5618, #6144, #25093 ) ) ;
#4706 = ORIENTED_EDGE ( 'NONE', *, *, #2561, .T. ) ;
#4707 = VECTOR ( 'NONE', #39660, 39.37007874015748143 ) ;
#4708 = CARTESIAN_POINT ( 'NONE',  ( 0.9989521216866641407, 0.000000000000000000, 1.767914056614194651 ) ) ;
#4710 = VERTEX_POINT ( 'NONE', #46280 ) ;
#4709 = EDGE_CURVE ( 'NONE', #36526, #41290, #38069, .T. ) ;
#4711 = ORIENTED_EDGE ( 'NONE', *, *, #9306, .F. ) ;
#4712 = CARTESIAN_POINT ( 'NONE',  ( 1.015142113812069979, 0.000000000000000000, 2.047244094488179567 ) ) ;
#4713 = DIRECTION ( 'NONE',  ( 1.000000000000000000, 0.000000000000000000, 0.000000000000000000 ) ) ;
#4714 = LINE ( 'NONE', #28958, #17040 ) ;
#4715 = ORIENTED_EDGE ( 'NONE', *, *, #49401, .T. ) ;
#4716 = LINE ( 'NONE', #32869, #24658 ) ;
#4717 =( BOUNDED_CURVE ( )  B_SPLINE_CURVE ( 3, ( #7106, #18730, #10974, #30855 ),
 .UNSPECIFIED., .F., .F. ) 
 B_SPLINE_CURVE_WITH_KNOTS ( ( 4, 4 ),
 ( 3.480195768903311837, 3.530968440970385203 ),
 .UNSPECIFIED. ) 
 CURVE ( )  GEOMETRIC_REPRESENTATION_ITEM ( )  RATIONAL_B_SPLINE_CURVE ( ( 1.000000000000000000, 0.9997851895178078152, 0.9997851895178078152, 1.000000000000000000 ) ) 
 REPRESENTATION_ITEM ( '' )  );
#4718 = CARTESIAN_POINT ( 'NONE',  ( -2.684503303748676739, 1.574886512437883246, -0.1698233845712802670 ) ) ;
#4719 = DIRECTION ( 'NONE',  ( 1.734723475976806848E-16, 0.000000000000000000, 1.000000000000000000 ) ) ;
#4720 = VERTEX_POINT ( 'NONE', #26430 ) ;
#4721 = PLANE ( 'NONE',  #36443 ) ;
#4722 = PLANE ( 'NONE',  #11211 ) ;
#4723 = ORIENTED_EDGE ( 'NONE', *, *, #17860, .T. ) ;
#4724 = PLANE ( 'NONE',  #22481 ) ;
#4725 = VERTEX_POINT ( 'NONE', #49877 ) ;
#4726 = ORIENTED_EDGE ( 'NONE', *, *, #34442, .F. ) ;
#4727 = CARTESIAN_POINT ( 'NONE',  ( -0.8942052331142552601, 3.346456692913386100, -1.259842519685034690 ) ) ;
#4728 = CONICAL_SURFACE ( 'NONE', #15557, 3.483074324928249421, 1.244861948955335196 ) ;
#4729 = DIRECTION ( 'NONE',  ( 0.000000000000000000, 0.000000000000000000, -1.000000000000000000 ) ) ;
#4730 = PLANE ( 'NONE',  #44253 ) ;
#4731 = CARTESIAN_POINT ( 'NONE',  ( 2.803168581536171100, 1.664457329461095592, 0.9280530358793855905 ) ) ;
#4732 = B_SPLINE_CURVE_WITH_KNOTS ( 'NONE', 3,
 ( #26076, #14199, #41827, #37962 ),
 .UNSPECIFIED., .F., .F.,
 ( 4, 4 ),
 ( 2.136331377199711613E-07, 0.01867141251301646793 ),
 .UNSPECIFIED. ) ;
#4733 = ORIENTED_EDGE ( 'NONE', *, *, #33318, .F. ) ;
#4734 = ORIENTED_EDGE ( 'NONE', *, *, #4806, .T. ) ;
#4735 = LINE ( 'NONE', #12735, #5304 ) ;
#4736 = ORIENTED_EDGE ( 'NONE', *, *, #46551, .F. ) ;
#4737 = DIRECTION ( 'NONE',  ( -0.6234898018587431423, -9.072499293938425721E-17, 0.7818314824680221431 ) ) ;
#4738 = DIRECTION ( 'NONE',  ( 0.000000000000000000, 0.000000000000000000, -1.000000000000000000 ) ) ;
#4739 = VECTOR ( 'NONE', #8586, 39.37007874015748143 ) ;
#4740 = VECTOR ( 'NONE', #8813, 39.37007874015748143 ) ;
#4741 = CARTESIAN_POINT ( 'NONE',  ( 1.293618082698028804, 0.000000000000000000, -1.168738992012442246 ) ) ;
#4742 = ADVANCED_FACE ( 'NONE', ( #26932 ), #10940, .F. ) ;
#4743 = CARTESIAN_POINT ( 'NONE',  ( 2.932638728931774352, 1.764957438482779528, 0.3475908556738225297 ) ) ;
#4744 = PLANE ( 'NONE',  #48457 ) ;
#4745 = ORIENTED_EDGE ( 'NONE', *, *, #48073, .T. ) ;
#4746 = ADVANCED_FACE ( 'NONE', ( #2941 ), #30059, .F. ) ;
#4747 = LINE ( 'NONE', #16880, #43955 ) ;
#4748 = CARTESIAN_POINT ( 'NONE',  ( -1.636583440222563635, 3.346456692913386100, -4.780733988912460139E-16 ) ) ;
#4749 = EDGE_CURVE ( 'NONE', #51046, #26290, #3446, .T. ) ;
#4750 = VERTEX_POINT ( 'NONE', #18184 ) ;
#4751 = CARTESIAN_POINT ( 'NONE',  ( 0.8182917201112819283, 0.000000000000000000, -0.9842519685039348154 ) ) ;
#4752 = CARTESIAN_POINT ( 'NONE',  ( 1.091055626815042645, 3.346456692913386100, -8.878505979408855953E-16 ) ) ;
#4753 = DIRECTION ( 'NONE',  ( 1.734723475976806848E-16, -0.000000000000000000, 1.000000000000000000 ) ) ;
#4754 = ORIENTED_EDGE ( 'NONE', *, *, #34362, .T. ) ;
#4755 = CARTESIAN_POINT ( 'NONE',  ( -1.316980176754435350, 0.5242972887528047909, -1.728942231640760330 ) ) ;
#4756 = CARTESIAN_POINT ( 'NONE',  ( 2.339241080213585899, 1.462148010760873307, 1.802537235681917815 ) ) ;
#4757 = CARTESIAN_POINT ( 'NONE',  ( -2.164823134740035737, 1.574811347331577016, -0.04796011690018289753 ) ) ;
#4758 = ORIENTED_EDGE ( 'NONE', *, *, #16062, .F. ) ;
#4759 = FACE_BOUND ( 'NONE', #20727, .T. ) ;
#4760 = CARTESIAN_POINT ( 'NONE',  ( -1.511286805986099546, 0.000000000000000000, 0.8691436966266951059 ) ) ;
#4761 = EDGE_LOOP ( 'NONE', ( #26551, #13226, #22270, #34587 ) ) ;
#4762 = CONICAL_SURFACE ( 'NONE', #26212, 2.246510896728926010, 0.01601546068027819014 ) ;
#4763 = CARTESIAN_POINT ( 'NONE',  ( 0.2727639067037604947, 3.346456692913386100, -1.102362204724405714 ) ) ;
#4764 = DIRECTION ( 'NONE',  ( 0.000000000000000000, 0.000000000000000000, -1.000000000000000000 ) ) ;
#4765 = EDGE_CURVE ( 'NONE', #25411, #1059, #2687, .T. ) ;
#4766 = CARTESIAN_POINT ( 'NONE',  ( -0.2431224069213033800, 1.205361022782829114E-17, 2.152304290637669926 ) ) ;
#4767 = DIRECTION ( 'NONE',  ( 1.000000000000000000, 0.000000000000000000, 0.000000000000000000 ) ) ;
#4768 = ORIENTED_EDGE ( 'NONE', *, *, #28064, .T. ) ;
#4769 = ORIENTED_EDGE ( 'NONE', *, *, #494, .T. ) ;
#4770 = LINE ( 'NONE', #24650, #39721 ) ;
#4771 = DIRECTION ( 'NONE',  ( 0.5773502691896268413, -0.5773502691896258421, -0.5773502691896243988 ) ) ;
#4772 = ADVANCED_FACE ( 'NONE', ( #30817 ), #41929, .F. ) ;
#4773 = ORIENTED_EDGE ( 'NONE', *, *, #42061, .T. ) ;
#4774 = CARTESIAN_POINT ( 'NONE',  ( 2.182111253630085290, 3.267716535433071279, 0.4330708661417287386 ) ) ;
#4775 = CARTESIAN_POINT ( 'NONE',  ( 0.7423782071083084855, 3.346456692913386100, -1.889763779527552812 ) ) ;
#4776 = DIRECTION ( 'NONE',  ( 1.086719731106949452E-16, -1.000000000000000000, -4.078527368698568598E-17 ) ) ;
#4777 = CARTESIAN_POINT ( 'NONE',  ( -1.166969139818015977, 0.000000000000000000, -0.1574803149606300023 ) ) ;
#4778 = VERTEX_POINT ( 'NONE', #22561 ) ;
#4779 = ORIENTED_EDGE ( 'NONE', *, *, #48601, .F. ) ;
#4780 = LINE ( 'NONE', #40417, #17217 ) ;
#4781 = DIRECTION ( 'NONE',  ( 0.000000000000000000, 0.7071067811865466846, -0.7071067811865483499 ) ) ;
#4782 = CIRCLE ( 'NONE', #3924, 2.165354330708661568 ) ;
#4783 = AXIS2_PLACEMENT_3D ( 'NONE', #1773, #17023, #28624 ) ;
#4784 = DIRECTION ( 'NONE',  ( -0.000000000000000000, 1.000000000000000000, -0.000000000000000000 ) ) ;
#4785 = DIRECTION ( 'NONE',  ( -0.9998717552508122886, -0.01601477604151181275, 0.000000000000000000 ) ) ;
#4786 = FACE_BOUND ( 'NONE', #11575, .T. ) ;
#4787 = VERTEX_POINT ( 'NONE', #18696 ) ;
#4788 = LINE ( 'NONE', #20788, #43868 ) ;
#4789 = EDGE_LOOP ( 'NONE', ( #40226, #11929, #47735, #7814 ) ) ;
#4791 = ORIENTED_EDGE ( 'NONE', *, *, #25202, .T. ) ;
#4790 = AXIS2_PLACEMENT_3D ( 'NONE', #20127, #36150, #32029 ) ;
#4792 = LINE ( 'NONE', #915, #41567 ) ;
#4793 = CIRCLE ( 'NONE', #22957, 2.165354330708661568 ) ;
#4794 = EDGE_LOOP ( 'NONE', ( #31580, #12070, #23326, #33820 ) ) ;
#4795 = EDGE_LOOP ( 'NONE', ( #9962, #24972, #5751, #19182 ) ) ;
#4796 = DIRECTION ( 'NONE',  ( 0.000000000000000000, 1.000000000000000000, 0.000000000000000000 ) ) ;
#4797 = VECTOR ( 'NONE', #23190, 39.37007874015748143 ) ;
#4798 = EDGE_LOOP ( 'NONE', ( #33515, #45814, #10272, #15915 ) ) ;
#4800 = CARTESIAN_POINT ( 'NONE',  ( -2.182111253630085290, 3.346456692913386100, 0.1181102362204704270 ) ) ;
#4799 = VECTOR ( 'NONE', #20488, 39.37007874015748143 ) ;
#4801 = B_SPLINE_CURVE_WITH_KNOTS ( 'NONE', 3,
 ( #21541, #25666, #6044, #41418 ),
 .UNSPECIFIED., .F., .F.,
 ( 4, 4 ),
 ( 2.558223320794676908E-07, 0.002500373615005052706 ),
 .UNSPECIFIED. ) ;
#4802 = CARTESIAN_POINT ( 'NONE',  ( 1.352759075253495258, 2.755905511811024056, 0.2762566512555730269 ) ) ;
#4803 = CARTESIAN_POINT ( 'NONE',  ( -2.770917298715283028, 0.6859011407150841233, 1.589814936510556720 ) ) ;
#4804 = CARTESIAN_POINT ( 'NONE',  ( 0.4787700707360283414, 1.205361022782829114E-17, -1.919768535593459724 ) ) ;
#4805 = B_SPLINE_CURVE_WITH_KNOTS ( 'NONE', 3,
 ( #27926, #12698, #48023, #4436 ),
 .UNSPECIFIED., .F., .F.,
 ( 4, 4 ),
 ( 0.01343717635322695669, 0.03074301205234334158 ),
 .UNSPECIFIED. ) ;
#4806 = EDGE_CURVE ( 'NONE', #29472, #6874, #45773, .T. ) ;
#4807 = CARTESIAN_POINT ( 'NONE',  ( -0.5455278134075214336, 3.346456692913386100, -0.1968503937007883287 ) ) ;
#4808 = LINE ( 'NONE', #416, #22891 ) ;
#4809 = ORIENTED_EDGE ( 'NONE', *, *, #45684, .T. ) ;
#4810 = ADVANCED_FACE ( 'NONE', ( #14819 ), #26681, .T. ) ;
#4811 = DIRECTION ( 'NONE',  ( 1.000000000000000000, 0.000000000000000000, 0.000000000000000000 ) ) ;
#4812 = DIRECTION ( 'NONE',  ( -1.000000000000000000, 0.000000000000000000, -0.000000000000000000 ) ) ;
#4813 = CARTESIAN_POINT ( 'NONE',  ( -1.636583440222563635, 3.267716535433071279, 0.9448818897637749625 ) ) ;
#4814 = ADVANCED_FACE ( 'NONE', ( #38570 ), #22315, .F. ) ;
#4815 = PRODUCT_DEFINITION ( 'UNKNOWN', '', #36630, #34459 ) ;
#4816 = ORIENTED_EDGE ( 'NONE', *, *, #1617, .F. ) ;
#4817 = LINE ( 'NONE', #39668, #42158 ) ;
#4818 = CARTESIAN_POINT ( 'NONE',  ( 1.833433833923351353, 0.000000000000000000, -0.3149606299212596716 ) ) ;
#4819 = ORIENTED_EDGE ( 'NONE', *, *, #6838, .F. ) ;
#4820 = DIRECTION ( 'NONE',  ( 0.000000000000000000, -1.000000000000000000, 0.000000000000000000 ) ) ;
#4821 = AXIS2_PLACEMENT_3D ( 'NONE', #27546, #44058, #8705 ) ;
#4822 = ADVANCED_FACE ( 'NONE', ( #34944 ), #34693, .T. ) ;
#4823 = DIRECTION ( 'NONE',  ( 1.734723475976806848E-16, -0.000000000000000000, 1.000000000000000000 ) ) ;
#4824 = LINE ( 'NONE', #43274, #42481 ) ;
#4825 = EDGE_LOOP ( 'NONE', ( #34619, #13350, #25148, #7372 ) ) ;
#4826 = VECTOR ( 'NONE', #42932, 39.37007874015748143 ) ;
#4827 = CARTESIAN_POINT ( 'NONE',  ( -1.909347346926324462, 3.346456692913386100, -0.3543307086614171930 ) ) ;
#4828 = ORIENTED_EDGE ( 'NONE', *, *, #13224, .F. ) ;
#4829 = FACE_BOUND ( 'NONE', #48392, .T. ) ;
#4830 = FACE_OUTER_BOUND ( 'NONE', #19761, .T. ) ;
#4831 = VECTOR ( 'NONE', #41423, 39.37007874015747433 ) ;
#4832 = VECTOR ( 'NONE', #49293, 39.37007874015748143 ) ;
#4833 = CARTESIAN_POINT ( 'NONE',  ( -1.536664496436148184E-16, 3.346456692913386100, -1.141732283464564013 ) ) ;
#4834 = ADVANCED_FACE ( 'NONE', ( #46528 ), #25930, .F. ) ;
#4835 = DIRECTION ( 'NONE',  ( 1.000000000000000000, 0.000000000000000000, 0.000000000000000000 ) ) ;
#4836 = ORIENTED_EDGE ( 'NONE', *, *, #10212, .T. ) ;
#4837 = ORIENTED_EDGE ( 'NONE', *, *, #28460, .F. ) ;
#4838 = LINE ( 'NONE', #23419, #26230 ) ;
#4839 = ORIENTED_EDGE ( 'NONE', *, *, #42619, .F. ) ;
#4840 = EDGE_CURVE ( 'NONE', #6948, #30730, #2442, .T. ) ;
#4841 = CARTESIAN_POINT ( 'NONE',  ( 0.04921259842519689481, -2.508534783339706724E-16, 2.213282802432568808 ) ) ;
#4842 = ORIENTED_EDGE ( 'NONE', *, *, #25364, .F. ) ;
#4843 = CARTESIAN_POINT ( 'NONE',  ( 1.083317450960588735, 1.005119572744525236, -2.362955334258993290 ) ) ;
#4844 = VECTOR ( 'NONE', #741, 39.37007874015748143 ) ;
#4845 = ORIENTED_EDGE ( 'NONE', *, *, #45343, .T. ) ;
#4846 = EDGE_CURVE ( 'NONE', #17653, #49899, #38820, .T. ) ;
#4847 = DIRECTION ( 'NONE',  ( -0.000000000000000000, 1.000000000000000000, -0.000000000000000000 ) ) ;
#4848 = CARTESIAN_POINT ( 'NONE',  ( -1.598949219967723101, 0.5249316475426858419, -0.9964897588581769217 ) ) ;
#4849 = ORIENTED_EDGE ( 'NONE', *, *, #5408, .F. ) ;
#4850 = FACE_OUTER_BOUND ( 'NONE', #5432, .T. ) ;
#4851 = VERTEX_POINT ( 'NONE', #41678 ) ;
#4852 = EDGE_CURVE ( 'NONE', #4778, #1584, #22060, .T. ) ;
#4853 = CARTESIAN_POINT ( 'NONE',  ( 1.015142113812069313, 3.346456692913386100, -0.6692913385826764205 ) ) ;
#4854 = AXIS2_PLACEMENT_3D ( 'NONE', #3244, #14360, #10491 ) ;
#4855 = ORIENTED_EDGE ( 'NONE', *, *, #14244, .T. ) ;
#4856 = VERTEX_POINT ( 'NONE', #28197 ) ;
#4857 = CARTESIAN_POINT ( 'NONE',  ( -1.632855683316659867, 1.205361022782829114E-17, -0.6443965869051290207 ) ) ;
#4858 = ORIENTED_EDGE ( 'NONE', *, *, #29604, .F. ) ;
#4859 = LINE ( 'NONE', #20601, #46838 ) ;
#4860 = ORIENTED_EDGE ( 'NONE', *, *, #19366, .F. ) ;
#4861 = CARTESIAN_POINT ( 'NONE',  ( 0.000000000000000000, 3.267716535433071279, -1.574803149606294417 ) ) ;
#4862 = CARTESIAN_POINT ( 'NONE',  ( -2.182111253630085734, 0.000000000000000000, -0.8267716535433052849 ) ) ;
#4863 = VECTOR ( 'NONE', #42173, 39.37007874015748143 ) ;
#4864 = VECTOR ( 'NONE', #34557, 39.37007874015748143 ) ;
#4865 = CARTESIAN_POINT ( 'NONE',  ( -0.07591351300297333182, 3.346456692913386100, -1.417322834645664331 ) ) ;
#4866 = ORIENTED_EDGE ( 'NONE', *, *, #49393, .T. ) ;
#4867 = CARTESIAN_POINT ( 'NONE',  ( 2.017116292511733189, 3.346456692913386100, -0.7874015748031473194 ) ) ;
#4868 = FACE_OUTER_BOUND ( 'NONE', #6174, .T. ) ;
#4869 = CARTESIAN_POINT ( 'NONE',  ( -0.6214413264104945434, 3.267716535433071279, 2.156057715732901026E-16 ) ) ;
#4870 = CARTESIAN_POINT ( 'NONE',  ( 0.5284761224300892346, 6.692913385826772199, -2.099874368989729234 ) ) ;
#4871 = VECTOR ( 'NONE', #15786, 39.37007874015748143 ) ;
#4872 = DIRECTION ( 'NONE',  ( 1.000000000000000000, 0.000000000000000000, 0.000000000000000000 ) ) ;
#4873 = DIRECTION ( 'NONE',  ( 1.000000000000000000, -0.000000000000000000, 0.000000000000000000 ) ) ;
#4874 = ADVANCED_FACE ( 'NONE', ( #16337 ), #43174, .F. ) ;
#4875 = CARTESIAN_POINT ( 'NONE',  ( 2.099568260077707027, 6.692913385826772199, -0.5296909464895783737 ) ) ;
#4876 = ADVANCED_FACE ( 'NONE', ( #8333 ), #589, .F. ) ;
#4877 = VERTEX_POINT ( 'NONE', #39575 ) ;
#4878 = EDGE_CURVE ( 'NONE', #49034, #6476, #12456, .T. ) ;
#4879 = FACE_OUTER_BOUND ( 'NONE', #34844, .T. ) ;
#4880 = ORIENTED_EDGE ( 'NONE', *, *, #43802, .T. ) ;
#4881 = DIRECTION ( 'NONE',  ( 1.000000000000000000, 0.000000000000000000, -1.156482317317871478E-16 ) ) ;
#4882 = ORIENTED_EDGE ( 'NONE', *, *, #9929, .F. ) ;
#4883 = DIRECTION ( 'NONE',  ( 0.000000000000000000, 0.000000000000000000, 1.000000000000000000 ) ) ;
#4884 = DIRECTION ( 'NONE',  ( 1.000000000000000000, -0.000000000000000000, 0.000000000000000000 ) ) ;
#4885 = FACE_OUTER_BOUND ( 'NONE', #44431, .T. ) ;
#4886 = CARTESIAN_POINT ( 'NONE',  ( -0.5455278134075216556, 3.346456692913386100, -2.204724409448810540 ) ) ;
#4887 = ORIENTED_EDGE ( 'NONE', *, *, #29758, .T. ) ;
#4888 = CARTESIAN_POINT ( 'NONE',  ( 3.256118103108526111E-16, 3.267716535433071279, 2.443628662382284489 ) ) ;
#4889 = FACE_BOUND ( 'NONE', #16339, .T. ) ;
#4890 = VERTEX_POINT ( 'NONE', #46775 ) ;
#4891 = CARTESIAN_POINT ( 'NONE',  ( 1.276224672101352153, 0.5249316475426865081, 1.385958525304569200 ) ) ;
#4892 = EDGE_LOOP ( 'NONE', ( #8482, #11764, #26805, #8017 ) ) ;
#4893 = AXIS2_PLACEMENT_3D ( 'NONE', #7088, #11709, #42696 ) ;
#4894 = FACE_OUTER_BOUND ( 'NONE', #50074, .T. ) ;
#4895 = DIRECTION ( 'NONE',  ( -1.000000000000000000, 0.000000000000000000, 0.000000000000000000 ) ) ;
#4896 = EDGE_CURVE ( 'NONE', #24628, #1125, #31575, .T. ) ;
#4897 = CIRCLE ( 'NONE', #11497, 1.181102362204723200 ) ;
#4898 = LINE ( 'NONE', #12909, #27163 ) ;
#4899 = VERTEX_POINT ( 'NONE', #11694 ) ;
#4900 = ORIENTED_EDGE ( 'NONE', *, *, #25123, .T. ) ;
#4901 = DIRECTION ( 'NONE',  ( -1.000000000000000000, 0.000000000000000000, 0.000000000000000000 ) ) ;
#4902 = LINE ( 'NONE', #20646, #3466 ) ;
#4903 = FACE_BOUND ( 'NONE', #5937, .T. ) ;
#4904 = CIRCLE ( 'NONE', #14827, 2.165354330708661568 ) ;
#4905 = EDGE_CURVE ( 'NONE', #8911, #43312, #27945, .T. ) ;
#4906 = PLANE ( 'NONE',  #45958 ) ;
#4907 = CARTESIAN_POINT ( 'NONE',  ( 0.07982360342473591996, 1.709180471932028711, 0.000000000000000000 ) ) ;
#4908 = EDGE_CURVE ( 'NONE', #12085, #29688, #31323, .T. ) ;
#4909 = VERTEX_POINT ( 'NONE', #31836 ) ;
#4910 = CARTESIAN_POINT ( 'NONE',  ( 0.000000000000000000, 3.267716535433071279, 0.4330708661417290162 ) ) ;
#4911 = B_SPLINE_CURVE_WITH_KNOTS ( 'NONE', 3,
 ( #9794, #20178, #24063, #16835 ),
 .UNSPECIFIED., .F., .F.,
 ( 4, 4 ),
 ( 3.862052508787299689E-07, 0.04892898802743299996 ),
 .UNSPECIFIED. ) ;
#4912 = EDGE_CURVE ( 'NONE', #23868, #47925, #7574, .T. ) ;
#4913 = ORIENTED_EDGE ( 'NONE', *, *, #766, .T. ) ;
#4914 = ORIENTED_EDGE ( 'NONE', *, *, #10069, .F. ) ;
#4916 = EDGE_CURVE ( 'NONE', #15234, #8249, #1429, .T. ) ;
#4915 = VERTEX_POINT ( 'NONE', #19931 ) ;
#4917 = DIRECTION ( 'NONE',  ( -3.469446951953613696E-16, 0.000000000000000000, -1.000000000000000000 ) ) ;
#4918 = DIRECTION ( 'NONE',  ( -3.469446951953613696E-16, 0.000000000000000000, -1.000000000000000000 ) ) ;
#4919 = VECTOR ( 'NONE', #27865, 39.37007874015748143 ) ;
#4920 = DIRECTION ( 'NONE',  ( 1.000000000000000000, 0.000000000000000000, -3.469446951953613696E-16 ) ) ;
#4921 = LINE ( 'NONE', #28919, #44466 ) ;
#4922 = EDGE_LOOP ( 'NONE', ( #13627, #35055, #24672, #46414 ) ) ;
#4923 = ORIENTED_EDGE ( 'NONE', *, *, #42368, .T. ) ;
#4924 = DIRECTION ( 'NONE',  ( 0.01601477604151182663, -0.9998717552508123996, 0.000000000000000000 ) ) ;
#4925 = LINE ( 'NONE', #28668, #25465 ) ;
#4926 = CARTESIAN_POINT ( 'NONE',  ( 0.4696143004045484348, 3.346456692913386100, 1.535433070866133898 ) ) ;
#4927 = CARTESIAN_POINT ( 'NONE',  ( -1.439733046521776139, 0.000000000000000000, 0.3149606299212578953 ) ) ;
#4928 = DIRECTION ( 'NONE',  ( -0.9749279121818259508, 0.000000000000000000, 0.2225209339563041788 ) ) ;
#4929 = EDGE_CURVE ( 'NONE', #37360, #49076, #7823, .T. ) ;
#4930 = CIRCLE ( 'NONE', #8214, 2.165354330708661568 ) ;
#4931 = DIRECTION ( 'NONE',  ( 1.734723475976806848E-16, -0.000000000000000000, 1.000000000000000000 ) ) ;
#4932 = EDGE_CURVE ( 'NONE', #39028, #26808, #50844, .T. ) ;
#4933 = EDGE_CURVE ( 'NONE', #3787, #4283, #3954, .T. ) ;
#4934 = DIRECTION ( 'NONE',  ( 0.000000000000000000, 0.000000000000000000, -1.000000000000000000 ) ) ;
#4935 = DIRECTION ( 'NONE',  ( -1.000000000000000000, -0.000000000000000000, -0.000000000000000000 ) ) ;
#4936 = ORIENTED_EDGE ( 'NONE', *, *, #17932, .F. ) ;
#4937 = FACE_OUTER_BOUND ( 'NONE', #23184, .T. ) ;
#4938 = CARTESIAN_POINT ( 'NONE',  ( 0.7423782071083084855, 0.000000000000000000, -1.889763779527552812 ) ) ;
#4939 = AXIS2_PLACEMENT_3D ( 'NONE', #25913, #42661, #34427 ) ;
#4940 = EDGE_LOOP ( 'NONE', ( #17995, #32729, #45783, #12798 ) ) ;
#4941 = ORIENTED_EDGE ( 'NONE', *, *, #19656, .T. ) ;
#4942 = LINE ( 'NONE', #44171, #5125 ) ;
#4943 = DIRECTION ( 'NONE',  ( 1.734723475976806848E-16, -0.000000000000000000, 1.000000000000000000 ) ) ;
#4944 = CARTESIAN_POINT ( 'NONE',  ( 1.909347346926324462, 0.000000000000000000, -0.7874015748031473194 ) ) ;
#4945 = ORIENTED_EDGE ( 'NONE', *, *, #1555, .T. ) ;
#4946 = ORIENTED_EDGE ( 'NONE', *, *, #10906, .T. ) ;
#4947 = DIRECTION ( 'NONE',  ( 1.734723475976806848E-16, 0.000000000000000000, 1.000000000000000000 ) ) ;
#4948 = EDGE_LOOP ( 'NONE', ( #8306, #20787, #23073, #40405 ) ) ;
#4949 = ORIENTED_EDGE ( 'NONE', *, *, #18847, .F. ) ;
#4950 = LINE ( 'NONE', #1844, #7880 ) ;
#4951 = FACE_OUTER_BOUND ( 'NONE', #7570, .T. ) ;
#4952 = CARTESIAN_POINT ( 'NONE',  ( 1.882988517681383200, 1.574803149606302854, 1.069164917025817507 ) ) ;
#4953 = EDGE_CURVE ( 'NONE', #42837, #31796, #12207, .T. ) ;
#4954 = ORIENTED_EDGE ( 'NONE', *, *, #18206, .T. ) ;
#4955 = ORIENTED_EDGE ( 'NONE', *, *, #20729, .T. ) ;
#4956 = VERTEX_POINT ( 'NONE', #16079 ) ;
#4957 = CARTESIAN_POINT ( 'NONE',  ( -2.544445989810643294, 1.675520440985067916, 0.8784858062910045895 ) ) ;
#4958 = ORIENTED_EDGE ( 'NONE', *, *, #3669, .T. ) ;
#4959 = VERTEX_POINT ( 'NONE', #31072 ) ;
#4960 = DIRECTION ( 'NONE',  ( -0.000000000000000000, 1.000000000000000000, -0.000000000000000000 ) ) ;
#4961 = LINE ( 'NONE', #43932, #48308 ) ;
#4962 = PLANE ( 'NONE',  #31893 ) ;
#4963 = EDGE_CURVE ( 'NONE', #47752, #32071, #35960, .T. ) ;
#4964 = VECTOR ( 'NONE', #38649, 39.37007874015748143 ) ;
#4965 = ORIENTED_EDGE ( 'NONE', *, *, #2303, .F. ) ;
#4966 = AXIS2_PLACEMENT_3D ( 'NONE', #18451, #24982, #10451 ) ;
#4967 = EDGE_CURVE ( 'NONE', #5543, #45211, #19427, .T. ) ;
#4968 = CARTESIAN_POINT ( 'NONE',  ( -2.454875160333845674, 3.189042514953126961, -0.3543307086614173040 ) ) ;
#4969 = CARTESIAN_POINT ( 'NONE',  ( -0.5455278134075213226, 3.267716535433071279, 9.463399047163221947E-17 ) ) ;
#4970 = CARTESIAN_POINT ( 'NONE',  ( 0.4696143004045479352, 0.000000000000000000, 0.1574803149606283648 ) ) ;
#4971 = EDGE_CURVE ( 'NONE', #17488, #5041, #4461, .T. ) ;
#4972 = ORIENTED_EDGE ( 'NONE', *, *, #958, .T. ) ;
#4973 = LINE ( 'NONE', #8588, #159 ) ;
#4974 = CARTESIAN_POINT ( 'NONE',  ( -1.636583440222563635, 0.000000000000000000, 0.3149606299212578953 ) ) ;
#4975 = CARTESIAN_POINT ( 'NONE',  ( -0.8942052331142552601, 0.000000000000000000, 2.204724409448808764 ) ) ;
#4976 = ORIENTED_EDGE ( 'NONE', *, *, #47779, .F. ) ;
#4977 = ORIENTED_EDGE ( 'NONE', *, *, #22978, .F. ) ;
#4978 = AXIS2_PLACEMENT_3D ( 'NONE', #17290, #9027, #48987 ) ;
#4979 = FACE_OUTER_BOUND ( 'NONE', #4892, .T. ) ;
#4980 = FACE_OUTER_BOUND ( 'NONE', #10040, .T. ) ;
#4981 = CARTESIAN_POINT ( 'NONE',  ( -1.149923682057703456, 1.049866565877818125, -1.666459639168880402 ) ) ;
#4982 = CARTESIAN_POINT ( 'NONE',  ( 1.979793062125284608, 1.651646828087945051, 2.191257344206569257 ) ) ;
#4983 = EDGE_CURVE ( 'NONE', #17988, #4450, #11447, .T. ) ;
#4984 = LINE ( 'NONE', #24608, #41176 ) ;
#4985 = ORIENTED_EDGE ( 'NONE', *, *, #7603, .F. ) ;
#4986 = VERTEX_POINT ( 'NONE', #23309 ) ;
#4987 = CARTESIAN_POINT ( 'NONE',  ( -1.439733046521777027, 3.346456692913386100, -0.8267716535433052849 ) ) ;
#4988 = EDGE_CURVE ( 'NONE', #36614, #35430, #39064, .T. ) ;
#4989 = ORIENTED_EDGE ( 'NONE', *, *, #43374, .T. ) ;
#4990 = CARTESIAN_POINT ( 'NONE',  ( -2.103998301714549157, 3.346456692913386100, -0.5118110236220464460 ) ) ;
#4991 = DIRECTION ( 'NONE',  ( -1.000000000000000000, 0.000000000000000000, 1.734723475976806848E-16 ) ) ;
#4992 = ADVANCED_FACE ( 'NONE', ( #25606 ), #9096, .F. ) ;
#4993 = EDGE_CURVE ( 'NONE', #20171, #43099, #17107, .T. ) ;
#4994 = DIRECTION ( 'NONE',  ( 1.000000000000000000, 0.000000000000000000, 0.000000000000000000 ) ) ;
#4995 = LINE ( 'NONE', #47043, #31837 ) ;
#4996 = CARTESIAN_POINT ( 'NONE',  ( 0.4696143004045484903, 3.346456692913386100, 1.102362204724404160 ) ) ;
#4997 = ORIENTED_EDGE ( 'NONE', *, *, #18346, .F. ) ;
#4998 = LINE ( 'NONE', #20742, #39027 ) ;
#4999 = EDGE_CURVE ( 'NONE', #26233, #16054, #16856, .T. ) ;
#5000 = DIRECTION ( 'NONE',  ( -0.000000000000000000, 1.000000000000000000, -0.000000000000000000 ) ) ;
#5001 = VECTOR ( 'NONE', #8288, 39.37007874015748143 ) ;
#5002 = ORIENTED_EDGE ( 'NONE', *, *, #5384, .T. ) ;
#5003 = LINE ( 'NONE', #9129, #966 ) ;
#5004 = VECTOR ( 'NONE', #46131, 39.37007874015748143 ) ;
#5005 = DIRECTION ( 'NONE',  ( -8.021399753802077430E-17, -1.000000000000000000, -8.389726389140663754E-17 ) ) ;
#5006 = DIRECTION ( 'NONE',  ( -1.000000000000000000, -0.000000000000000000, -0.000000000000000000 ) ) ;
#5007 = ORIENTED_EDGE ( 'NONE', *, *, #26540, .F. ) ;
#5008 = CARTESIAN_POINT ( 'NONE',  ( -2.182111253630085290, 3.346456692913386100, -0.3149606299212589500 ) ) ;
#5009 = LINE ( 'NONE', #36512, #7695 ) ;
#5010 = CARTESIAN_POINT ( 'NONE',  ( -0.04921259842519689481, 0.000000000000000000, 2.952755905511811108 ) ) ;
#5011 = ORIENTED_EDGE ( 'NONE', *, *, #10243, .T. ) ;
#5012 = LINE ( 'NONE', #16383, #7371 ) ;
#5013 = VECTOR ( 'NONE', #40471, 39.37007874015748143 ) ;
#5014 = LINE ( 'NONE', #44247, #23280 ) ;
#5015 = ORIENTED_EDGE ( 'NONE', *, *, #32273, .T. ) ;
#5016 = DIRECTION ( 'NONE',  ( -1.000000000000000000, 0.000000000000000000, 1.734723475976806848E-16 ) ) ;
#5017 = CARTESIAN_POINT ( 'NONE',  ( 2.715732320886252271, 2.755905511811027164, 1.948858261851765361 ) ) ;
#5018 = CARTESIAN_POINT ( 'NONE',  ( -1.794796351285542491, 3.346456692913386100, 1.102362204724404160 ) ) ;
#5019 = LINE ( 'NONE', #13283, #28438 ) ;
#5020 = SHAPE_REPRESENTATION ( 'Top Cover', ( #26741 ), #16013 ) ;
#5021 = DIRECTION ( 'NONE',  ( 0.000000000000000000, 0.000000000000000000, -1.000000000000000000 ) ) ;
#5022 = ORIENTED_EDGE ( 'NONE', *, *, #48676, .T. ) ;
#5023 = ORIENTED_EDGE ( 'NONE', *, *, #40851, .F. ) ;
#5024 = LINE ( 'NONE', #4007, #47086 ) ;
#5025 = DIRECTION ( 'NONE',  ( 0.000000000000000000, 0.000000000000000000, -1.000000000000000000 ) ) ;
#5026 = ORIENTED_EDGE ( 'NONE', *, *, #691, .T. ) ;
#5027 = CARTESIAN_POINT ( 'NONE',  ( -0.3486774197067334380, 3.267716535433071279, 0.9448818897637749625 ) ) ;
#5028 = LINE ( 'NONE', #5281, #21937 ) ;
#5029 = CARTESIAN_POINT ( 'NONE',  ( 2.663634708613022539, 1.658847949249850462, -0.6584354324901854350 ) ) ;
#5030 = DIRECTION ( 'NONE',  ( -3.469446951953613696E-16, 0.000000000000000000, -1.000000000000000000 ) ) ;
#5031 = ORIENTED_EDGE ( 'NONE', *, *, #38373, .T. ) ;
#5032 = ORIENTED_EDGE ( 'NONE', *, *, #13516, .T. ) ;
#5033 = EDGE_CURVE ( 'NONE', #10946, #14069, #28711, .T. ) ;
#5034 = DIRECTION ( 'NONE',  ( 1.000000000000000000, 0.000000000000000000, 0.000000000000000000 ) ) ;
#5035 = DIRECTION ( 'NONE',  ( -3.469446951953613696E-16, 0.000000000000000000, -1.000000000000000000 ) ) ;
#5036 = CARTESIAN_POINT ( 'NONE',  ( -0.04921259842519688094, 0.02713143566191717967, 1.843522435433914142 ) ) ;
#5037 = ORIENTED_EDGE ( 'NONE', *, *, #17363, .F. ) ;
#5038 = DIRECTION ( 'NONE',  ( 0.000000000000000000, 0.000000000000000000, 1.000000000000000000 ) ) ;
#5039 = EDGE_CURVE ( 'NONE', #41221, #39372, #48552, .T. ) ;
#5040 = FACE_BOUND ( 'NONE', #4798, .T. ) ;
#5041 = VERTEX_POINT ( 'NONE', #5985 ) ;
#5042 = DIRECTION ( 'NONE',  ( 5.782411586589357392E-17, 0.000000000000000000, 1.000000000000000000 ) ) ;
#5043 = ORIENTED_EDGE ( 'NONE', *, *, #16110, .F. ) ;
#5044 = VERTEX_POINT ( 'NONE', #32609 ) ;
#5045 = DIRECTION ( 'NONE',  ( 0.9009688679024218105, 0.000000000000000000, -0.4338837391175526803 ) ) ;
#5046 = AXIS2_PLACEMENT_3D ( 'NONE', #21702, #6717, #17323 ) ;
#5047 = VECTOR ( 'NONE', #45197, 39.37007874015748143 ) ;
#5048 = VERTEX_POINT ( 'NONE', #24849 ) ;
#5049 = ORIENTED_EDGE ( 'NONE', *, *, #36805, .F. ) ;
#5050 = PLANE ( 'NONE',  #18695 ) ;
#5051 = UNCERTAINTY_MEASURE_WITH_UNIT (LENGTH_MEASURE( 1.000000000000000082E-05 ), #13245, 'distance_accuracy_value', 'NONE');
#5052 = VERTEX_POINT ( 'NONE', #29485 ) ;
#5053 = VECTOR ( 'NONE', #30244, 39.37007874015748143 ) ;
#5054 = EDGE_CURVE ( 'NONE', #373, #17272, #40598, .T. ) ;
#5055 = DIRECTION ( 'NONE',  ( -0.000000000000000000, 0.000000000000000000, 1.000000000000000000 ) ) ;
#5056 = CARTESIAN_POINT ( 'NONE',  ( 0.4788131938641111973, 1.504819983455083277, 2.914091152102192162 ) ) ;
#5057 = LINE ( 'NONE', #47356, #47300 ) ;
#5058 = VECTOR ( 'NONE', #38162, 39.37007874015748143 ) ;
#5059 = EDGE_CURVE ( 'NONE', #35559, #28822, #9353, .T. ) ;
#5060 = DIRECTION ( 'NONE',  ( -1.000000000000000000, 0.000000000000000000, -0.000000000000000000 ) ) ;
#5061 = CARTESIAN_POINT ( 'NONE',  ( 1.015142113812069313, 3.346456692913386100, -0.7874015748031473194 ) ) ;
#5062 = CARTESIAN_POINT ( 'NONE',  ( 0.1968503937007874405, 0.000000000000000000, 0.000000000000000000 ) ) ;
#5063 = ORIENTED_EDGE ( 'NONE', *, *, #10594, .F. ) ;
#5064 = CARTESIAN_POINT ( 'NONE',  ( -0.6214413264104939882, 3.346456692913386100, 1.417322834645662777 ) ) ;
#5065 = EDGE_CURVE ( 'NONE', #54, #45803, #12979, .T. ) ;
#5066 = CARTESIAN_POINT ( 'NONE',  ( -2.121469926805683137, 6.692913385826772199, -0.4337334748181714827 ) ) ;
#5067 = ORIENTED_EDGE ( 'NONE', *, *, #46689, .T. ) ;
#5068 = LINE ( 'NONE', #9963, #42952 ) ;
#5069 = CARTESIAN_POINT ( 'NONE',  ( -0.3486774197067339376, 3.267716535433071279, -0.9448818897637762948 ) ) ;
#5070 = ORIENTED_EDGE ( 'NONE', *, *, #32379, .F. ) ;
#5071 = CARTESIAN_POINT ( 'NONE',  ( 2.923830433158672637, 1.447338937300884254, 0.4126163062934453118 ) ) ;
#5072 = CARTESIAN_POINT ( 'NONE',  ( 2.947574761915768171, 1.765190094501404072, -0.1816379373804911379 ) ) ;
#5073 = LINE ( 'NONE', #20036, #44933 ) ;
#5074 = ORIENTED_EDGE ( 'NONE', *, *, #11349, .F. ) ;
#5075 = CARTESIAN_POINT ( 'NONE',  ( -3.001271764839907430, 5.118110236220475784, 0.08552506819282497397 ) ) ;
#5076 = ORIENTED_EDGE ( 'NONE', *, *, #50492, .F. ) ;
#5077 = FACE_BOUND ( 'NONE', #25467, .T. ) ;
#5078 = DIRECTION ( 'NONE',  ( 0.9998717552508121775, 0.01601477604151182663, 0.000000000000000000 ) ) ;
#5079 = CONICAL_SURFACE ( 'NONE', #38079, 3.483074324928249421, 1.244861948955335196 ) ;
#5080 = AXIS2_PLACEMENT_3D ( 'NONE', #5292, #16409, #4785 ) ;
#5081 = DIRECTION ( 'NONE',  ( 0.7071067811865486830, 0.000000000000000000, 0.7071067811865462405 ) ) ;
#5082 = CARTESIAN_POINT ( 'NONE',  ( 0.000000000000000000, 3.346456692913386100, 0.000000000000000000 ) ) ;
#5083 = AXIS2_PLACEMENT_3D ( 'NONE', #7374, #641, #28505 ) ;
#5084 = ORIENTED_EDGE ( 'NONE', *, *, #17746, .T. ) ;
#5085 = ORIENTED_EDGE ( 'NONE', *, *, #16592, .F. ) ;
#5086 = PLANE ( 'NONE',  #13114 ) ;
#5087 = VERTEX_POINT ( 'NONE', #5219 ) ;
#5088 = AXIS2_PLACEMENT_3D ( 'NONE', #13618, #44075, #29355 ) ;
#5089 = DIRECTION ( 'NONE',  ( -0.000000000000000000, 0.000000000000000000, 1.000000000000000000 ) ) ;
#5090 = ORIENTED_EDGE ( 'NONE', *, *, #21562, .T. ) ;
#5091 = LINE ( 'NONE', #32476, #2552 ) ;
#5092 = AXIS2_PLACEMENT_3D ( 'NONE', #37785, #30280, #45490 ) ;
#5093 = ORIENTED_EDGE ( 'NONE', *, *, #41636, .T. ) ;
#5094 = DIRECTION ( 'NONE',  ( -0.000000000000000000, 0.000000000000000000, 1.000000000000000000 ) ) ;
#5095 = CARTESIAN_POINT ( 'NONE',  ( -2.150518151785907772, 1.673457466938482296, -0.2530435858860717313 ) ) ;
#5096 = EDGE_CURVE ( 'NONE', #11186, #7899, #40853, .T. ) ;
#5097 = ORIENTED_EDGE ( 'NONE', *, *, #917, .T. ) ;
#5098 = EDGE_CURVE ( 'NONE', #29929, #41791, #33122, .T. ) ;
#5099 = PLANE ( 'NONE',  #50394 ) ;
#5100 = VERTEX_POINT ( 'NONE', #29225 ) ;
#5101 = EDGE_CURVE ( 'NONE', #25743, #36107, #9153, .T. ) ;
#5103 = EDGE_LOOP ( 'NONE', ( #630, #39990, #49805, #12724 ) ) ;
#5102 = EDGE_CURVE ( 'NONE', #31043, #19694, #36730, .T. ) ;
#5104 = ORIENTED_EDGE ( 'NONE', *, *, #6795, .T. ) ;
#5105 = LINE ( 'NONE', #16735, #24006 ) ;
#5106 = VERTEX_POINT ( 'NONE', #28963 ) ;
#5107 = CARTESIAN_POINT ( 'NONE',  ( -0.07591351300297340121, 3.267716535433071279, -0.03937007874015908959 ) ) ;
#5108 = VERTEX_POINT ( 'NONE', #16597 ) ;
#5109 = CARTESIAN_POINT ( 'NONE',  ( -0.8182917201112819283, 3.267716535433071279, 1.419509857074483292E-16 ) ) ;
#5110 = CIRCLE ( 'NONE', #21594, 2.244934639244525076 ) ;
#5111 = CARTESIAN_POINT ( 'NONE',  ( 2.755905511811024056, 2.913385826771657250, -1.023622047244094224 ) ) ;
#5112 = EDGE_CURVE ( 'NONE', #41298, #26467, #48801, .T. ) ;
#5113 = CARTESIAN_POINT ( 'NONE',  ( -0.5455278134075214336, 3.346456692913386100, 2.007874015748021268 ) ) ;
#5114 = ORIENTED_EDGE ( 'NONE', *, *, #17469, .T. ) ;
#5115 = B_SPLINE_CURVE_WITH_KNOTS ( 'NONE', 3,
 ( #47195, #32015, #47707, #12382 ),
 .UNSPECIFIED., .F., .F.,
 ( 4, 4 ),
 ( 0.001822208875684674370, 0.04534500198965564499 ),
 .UNSPECIFIED. ) ;
#5116 = AXIS2_PLACEMENT_3D ( 'NONE', #4191, #24067, #28893 ) ;
#5117 = CARTESIAN_POINT ( 'NONE',  ( 0.6233543567505464011, 1.574803149606302854, -2.073689640095370379 ) ) ;
#5118 = CARTESIAN_POINT ( 'NONE',  ( 1.838947341486932396, 0.05737377265108637575, 0.6492553997849701553 ) ) ;
#5119 = LINE ( 'NONE', #36622, #1029 ) ;
#5120 = CARTESIAN_POINT ( 'NONE',  ( -0.2727639067037608278, 0.000000000000000000, -0.9842519685039344823 ) ) ;
#5121 = EDGE_CURVE ( 'NONE', #41095, #36016, #44700, .T. ) ;
#5122 = VECTOR ( 'NONE', #17177, 39.37007874015748143 ) ;
#5123 = CARTESIAN_POINT ( 'NONE',  ( 2.052631463899901920, 3.346456692913386100, -0.4724409448818889246 ) ) ;
#5124 = CARTESIAN_POINT ( 'NONE',  ( 1.531154912952772396, 1.205361022782829114E-17, 1.532020527533857646 ) ) ;
#5125 = VECTOR ( 'NONE', #12952, 39.37007874015748143 ) ;
#5126 = DIRECTION ( 'NONE',  ( -0.01601477604151182663, 0.9998717552508123996, -0.000000000000000000 ) ) ;
#5127 = ORIENTED_EDGE ( 'NONE', *, *, #41999, .T. ) ;
#5128 = DIRECTION ( 'NONE',  ( -3.469446951953613696E-16, 0.000000000000000000, -1.000000000000000000 ) ) ;
#5129 = CARTESIAN_POINT ( 'NONE',  ( 0.000000000000000000, 6.692913385826772199, 0.000000000000000000 ) ) ;
#5130 = VERTEX_POINT ( 'NONE', #41114 ) ;
#5131 = LINE ( 'NONE', #41273, #8629 ) ;
#5132 = ORIENTED_EDGE ( 'NONE', *, *, #18754, .T. ) ;
#5133 = ADVANCED_FACE ( 'NONE', ( #5737 ), #9866, .F. ) ;
#5134 = DIRECTION ( 'NONE',  ( 0.000000000000000000, 0.000000000000000000, 1.000000000000000000 ) ) ;
#5135 = FACE_OUTER_BOUND ( 'NONE', #30795, .T. ) ;
#5136 = CARTESIAN_POINT ( 'NONE',  ( -1.636583440222563635, 0.000000000000000000, 0.6299212598425164567 ) ) ;
#5137 = CYLINDRICAL_SURFACE ( 'NONE', #40765, 2.165354330708661568 ) ;
#5138 = LINE ( 'NONE', #16511, #26885 ) ;
#5139 = ORIENTED_EDGE ( 'NONE', *, *, #23479, .T. ) ;
#5140 = DIRECTION ( 'NONE',  ( -0.01601477604151182663, 0.9998717552508123996, -0.000000000000000000 ) ) ;
#5141 = FACE_BOUND ( 'NONE', #15625, .T. ) ;
#5142 = EDGE_LOOP ( 'NONE', ( #50252, #42769, #12288, #35125 ) ) ;
#5143 = DIRECTION ( 'NONE',  ( -0.01601477604151182663, 0.9998717552508123996, -0.000000000000000000 ) ) ;
#5144 = ORIENTED_EDGE ( 'NONE', *, *, #39737, .T. ) ;
#5145 = DIRECTION ( 'NONE',  ( 7.097135778201662695E-17, 1.000000000000000000, -1.075170113095010447E-16 ) ) ;
#5146 = DIRECTION ( 'NONE',  ( -1.000000000000000000, 0.000000000000000000, -0.000000000000000000 ) ) ;
#5147 = VECTOR ( 'NONE', #14113, 39.37007874015748143 ) ;
#5148 = DIRECTION ( 'NONE',  ( 0.000000000000000000, -1.000000000000000000, -0.000000000000000000 ) ) ;
#5149 = ORIENTED_EDGE ( 'NONE', *, *, #24398, .T. ) ;
#5151 = VERTEX_POINT ( 'NONE', #44200 ) ;
#5150 = EDGE_CURVE ( 'NONE', #31480, #46130, #22877, .T. ) ;
#5152 = CARTESIAN_POINT ( 'NONE',  ( 1.312248418042879727, 1.574803149606302854, -1.722429524498089393 ) ) ;
#5154 = LINE ( 'NONE', #17296, #47090 ) ;
#5153 = CIRCLE ( 'NONE', #25795, 2.164630168518208109 ) ;
#5155 = FACE_BOUND ( 'NONE', #9383, .T. ) ;
#5156 = EDGE_CURVE ( 'NONE', #33305, #43110, #8843, .T. ) ;
#5157 = VECTOR ( 'NONE', #16491, 39.37007874015748143 ) ;
#5158 = AXIS2_PLACEMENT_3D ( 'NONE', #28147, #4924, #36684 ) ;
#5159 = DIRECTION ( 'NONE',  ( 0.000000000000000000, -1.000000000000000000, 0.000000000000000000 ) ) ;
#5160 = PLANE ( 'NONE',  #8571 ) ;
#5161 = EDGE_CURVE ( 'NONE', #36537, #13304, #6755, .T. ) ;
#5162 = EDGE_CURVE ( 'NONE', #47679, #50505, #18121, .T. ) ;
#5163 = ORIENTED_EDGE ( 'NONE', *, *, #45852, .T. ) ;
#5164 = DIRECTION ( 'NONE',  ( -3.986037398843765983E-20, -1.000000000000000000, -1.160734090543304660E-16 ) ) ;
#5165 = VERTEX_POINT ( 'NONE', #45962 ) ;
#5166 = ORIENTED_EDGE ( 'NONE', *, *, #18903, .F. ) ;
#5167 = B_SPLINE_CURVE_WITH_KNOTS ( 'NONE', 3,
 ( #3729, #19460, #31868, #31353 ),
 .UNSPECIFIED., .F., .F.,
 ( 4, 4 ),
 ( 6.518678076764506353E-07, 0.004612785042107461070 ),
 .UNSPECIFIED. ) ;
#5168 = VERTEX_POINT ( 'NONE', #37753 ) ;
#5169 = DIRECTION ( 'NONE',  ( -0.000000000000000000, -1.000000000000000000, -0.000000000000000000 ) ) ;
#5170 = PLANE ( 'NONE',  #7698 ) ;
#5171 = EDGE_CURVE ( 'NONE', #11955, #30948, #10630, .T. ) ;
#5172 = DIRECTION ( 'NONE',  ( 1.000000000000000000, 0.000000000000000000, 0.000000000000000000 ) ) ;
#5173 = DIRECTION ( 'NONE',  ( -1.000000000000000000, 0.000000000000000000, -0.000000000000000000 ) ) ;
#5174 = VERTEX_POINT ( 'NONE', #49563 ) ;
#5175 = VERTEX_POINT ( 'NONE', #26369 ) ;
#5176 = CARTESIAN_POINT ( 'NONE',  ( 1.152895553066221934, 1.205361022782829114E-17, -1.833672301139072092 ) ) ;
#5177 = DIRECTION ( 'NONE',  ( -3.469446951953613696E-16, 0.000000000000000000, -1.000000000000000000 ) ) ;
#5178 = CARTESIAN_POINT ( 'NONE',  ( -1.377952755905513360, 0.000000000000000000, 2.165354330708661568 ) ) ;
#5179 = EDGE_CURVE ( 'NONE', #23170, #34848, #14732, .T. ) ;
#5180 = DIRECTION ( 'NONE',  ( 1.000000000000000000, 0.000000000000000000, 0.000000000000000000 ) ) ;
#5181 = CARTESIAN_POINT ( 'NONE',  ( 1.015142113812069313, 3.346456692913386100, -1.102362204724405714 ) ) ;
#5182 = LINE ( 'NONE', #17073, #37526 ) ;
#5183 = EDGE_CURVE ( 'NONE', #4787, #18808, #42115, .T. ) ;
#5184 = DIRECTION ( 'NONE',  ( 1.000000000000000000, 0.000000000000000000, 0.000000000000000000 ) ) ;
#5185 = AXIS2_PLACEMENT_3D ( 'NONE', #21996, #12978, #21484 ) ;
#5186 = ORIENTED_EDGE ( 'NONE', *, *, #25169, .F. ) ;
#5187 = DIRECTION ( 'NONE',  ( -0.9998717552508121775, -0.01601477604151182663, 0.000000000000000000 ) ) ;
#5188 = LINE ( 'NONE', #6218, #2984 ) ;
#5189 = EDGE_LOOP ( 'NONE', ( #27153, #29663, #29166, #50793 ) ) ;
#5190 = ADVANCED_FACE ( 'NONE', ( #2376 ), #26617, .F. ) ;
#5191 = AXIS2_PLACEMENT_3D ( 'NONE', #29944, #13693, #44907 ) ;
#5192 = ORIENTED_EDGE ( 'NONE', *, *, #6673, .F. ) ;
#5193 = VECTOR ( 'NONE', #3851, 39.37007874015748143 ) ;
#5194 = DIRECTION ( 'NONE',  ( 1.000000000000000000, 0.000000000000000000, 0.000000000000000000 ) ) ;
#5195 = CARTESIAN_POINT ( 'NONE',  ( 1.560669927219590303, 0.000000000000000000, -1.417322834645665219 ) ) ;
#5196 = ORIENTED_EDGE ( 'NONE', *, *, #25031, .F. ) ;
#5197 = VECTOR ( 'NONE', #35033, 39.37007874015748143 ) ;
#5198 = EDGE_CURVE ( 'NONE', #47008, #18423, #22500, .T. ) ;
#5199 = ORIENTED_EDGE ( 'NONE', *, *, #36575, .T. ) ;
#5200 = PLANE ( 'NONE',  #34503 ) ;
#5201 = VERTEX_POINT ( 'NONE', #45711 ) ;
#5202 = ORIENTED_EDGE ( 'NONE', *, *, #3385, .F. ) ;
#5203 = EDGE_CURVE ( 'NONE', #25675, #40849, #45455, .T. ) ;
#5204 = FACE_OUTER_BOUND ( 'NONE', #32993, .T. ) ;
#5205 = CARTESIAN_POINT ( 'NONE',  ( -0.7582255214199161708, 0.000000000000000000, -1.687894986714875811 ) ) ;
#5206 = ORIENTED_EDGE ( 'NONE', *, *, #50818, .T. ) ;
#5207 = VERTEX_POINT ( 'NONE', #2879 ) ;
#5208 = VERTEX_POINT ( 'NONE', #18632 ) ;
#5209 = LINE ( 'NONE', #25344, #24683 ) ;
#5210 = ORIENTED_EDGE ( 'NONE', *, *, #43069, .T. ) ;
#5211 = ORIENTED_EDGE ( 'NONE', *, *, #35567, .T. ) ;
#5212 = CARTESIAN_POINT ( 'NONE',  ( 1.909347346926324684, 3.346456692913386100, 1.021348170950612033 ) ) ;
#5213 = CARTESIAN_POINT ( 'NONE',  ( 2.164823134740036625, 6.692913385826772199, -0.04796011690015051371 ) ) ;
#5214 = CARTESIAN_POINT ( 'NONE',  ( -1.613060539954027872, 1.682065834201676324, -1.474157253483306507 ) ) ;
#5215 = ADVANCED_FACE ( 'NONE', ( #41867 ), #6508, .T. ) ;
#5216 = VERTEX_POINT ( 'NONE', #33881 ) ;
#5217 = DIRECTION ( 'NONE',  ( 1.000000000000000000, 0.000000000000000000, 0.000000000000000000 ) ) ;
#5218 = CARTESIAN_POINT ( 'NONE',  ( -0.5455278134075214336, 3.346456692913386100, -1.574803149606293529 ) ) ;
#5219 = CARTESIAN_POINT ( 'NONE',  ( -1.377952755905510918, 0.000000000000000000, -4.133858267716536083 ) ) ;
#5220 = EDGE_CURVE ( 'NONE', #39958, #44569, #38005, .T. ) ;
#5221 = ORIENTED_EDGE ( 'NONE', *, *, #12536, .F. ) ;
#5222 = FACE_OUTER_BOUND ( 'NONE', #33682, .T. ) ;
#5223 = VECTOR ( 'NONE', #7754, 39.37007874015748143 ) ;
#5224 = CARTESIAN_POINT ( 'NONE',  ( -0.6214413264104939882, 0.000000000000000000, 0.9055118110236167750 ) ) ;
#5225 = DIRECTION ( 'NONE',  ( 0.000000000000000000, 1.000000000000000000, 0.000000000000000000 ) ) ;
#5226 = ORIENTED_EDGE ( 'NONE', *, *, #15675, .T. ) ;
#5227 = AXIS2_PLACEMENT_3D ( 'NONE', #6980, #10849, #26587 ) ;
#5228 = ORIENTED_EDGE ( 'NONE', *, *, #22310, .F. ) ;
#5229 = DIRECTION ( 'NONE',  ( 0.000000000000000000, -1.000000000000000000, 0.000000000000000000 ) ) ;
#5230 = DIRECTION ( 'NONE',  ( -1.000000000000000000, 0.000000000000000000, 0.000000000000000000 ) ) ;
#5231 = AXIS2_PLACEMENT_3D ( 'NONE', #3082, #35086, #26570 ) ;
#5232 = CIRCLE ( 'NONE', #282, 2.106299212598425008 ) ;
#5233 = DIRECTION ( 'NONE',  ( 0.000000000000000000, 0.000000000000000000, -1.000000000000000000 ) ) ;
#5234 = LINE ( 'NONE', #49328, #36864 ) ;
#5235 = CARTESIAN_POINT ( 'NONE',  ( 0.7423782071083087075, 0.000000000000000000, -0.9448818897637765168 ) ) ;
#5236 = ORIENTED_EDGE ( 'NONE', *, *, #26883, .T. ) ;
#5237 = ORIENTED_EDGE ( 'NONE', *, *, #49263, .F. ) ;
#5238 = VECTOR ( 'NONE', #21001, 39.37007874015748143 ) ;
#5239 = CARTESIAN_POINT ( 'NONE',  ( 1.015142113812069313, 3.346456692913386100, -0.1574803149606301411 ) ) ;
#5240 = ORIENTED_EDGE ( 'NONE', *, *, #39388, .T. ) ;
#5241 = LINE ( 'NONE', #32628, #43907 ) ;
#5242 = LINE ( 'NONE', #44977, #16014 ) ;
#5243 = EDGE_CURVE ( 'NONE', #22183, #15854, #3128, .T. ) ;
#5244 = DIRECTION ( 'NONE',  ( -1.000000000000000000, 0.000000000000000000, 1.734723475976806848E-16 ) ) ;
#5245 = CARTESIAN_POINT ( 'NONE',  ( -0.3486774197067341041, 3.267716535433071279, 1.209717811016579571E-16 ) ) ;
#5246 = CARTESIAN_POINT ( 'NONE',  ( -1.002259110181423551, 1.593423740086483020, -1.967789019142131002 ) ) ;
#5247 = EDGE_LOOP ( 'NONE', ( #565, #311, #9454, #26075, #14028, #42552 ) ) ;
#5248 = DIRECTION ( 'NONE',  ( -3.469446951953613696E-16, 0.000000000000000000, -1.000000000000000000 ) ) ;
#5249 = LINE ( 'NONE', #5510, #45476 ) ;
#5250 = EDGE_CURVE ( 'NONE', #21513, #17057, #46217, .T. ) ;
#5251 = ORIENTED_EDGE ( 'NONE', *, *, #16199, .F. ) ;
#5252 = LINE ( 'NONE', #28997, #34760 ) ;
#5253 = EDGE_CURVE ( 'NONE', #20106, #10800, #33627, .T. ) ;
#5254 = LINE ( 'NONE', #6283, #8009 ) ;
#5255 = CARTESIAN_POINT ( 'NONE',  ( 4.580371886574746102E-17, 7.874015748031496287, 0.3740157480314960647 ) ) ;
#5257 = EDGE_CURVE ( 'NONE', #6252, #10014, #36998, .T. ) ;
#5256 = ORIENTED_EDGE ( 'NONE', *, *, #43702, .T. ) ;
#5258 = CARTESIAN_POINT ( 'NONE',  ( -1.359688503674094884, 0.002096987401480311045, 1.147260674818413761 ) ) ;
#5259 = FACE_OUTER_BOUND ( 'NONE', #32846, .T. ) ;
#5260 = AXIS2_PLACEMENT_3D ( 'NONE', #16155, #24414, #48116 ) ;
#5261 = EDGE_CURVE ( 'NONE', #25678, #17533, #34414, .T. ) ;
#5262 = ORIENTED_EDGE ( 'NONE', *, *, #10542, .T. ) ;
#5263 = AXIS2_PLACEMENT_3D ( 'NONE', #21144, #13654, #5653 ) ;
#5264 = CARTESIAN_POINT ( 'NONE',  ( -1.022179187220786156, 1.536459357544157411, 2.770232080386278106 ) ) ;
#5265 = CARTESIAN_POINT ( 'NONE',  ( 2.190654571063535005, 1.742989292944022939, 0.7635320059819211691 ) ) ;
#5266 = ORIENTED_EDGE ( 'NONE', *, *, #21122, .T. ) ;
#5267 = LINE ( 'NONE', #1648, #18784 ) ;
#5268 = CIRCLE ( 'NONE', #28364, 1.743387098533651480 ) ;
#5269 = VECTOR ( 'NONE', #47746, 39.37007874015748143 ) ;
#5270 = CARTESIAN_POINT ( 'NONE',  ( -1.891439052599157122, 1.677607092856729709, 1.073712343777111222 ) ) ;
#5271 = LINE ( 'NONE', #20760, #15628 ) ;
#5272 = PLANE ( 'NONE',  #3726 ) ;
#5273 = CARTESIAN_POINT ( 'NONE',  ( -1.091055626815042201, 3.346456692913386100, 1.259842519685033357 ) ) ;
#5274 = EDGE_LOOP ( 'NONE', ( #8670, #5023, #37442, #29473 ) ) ;
#5275 = ORIENTED_EDGE ( 'NONE', *, *, #17950, .F. ) ;
#5276 = FACE_OUTER_BOUND ( 'NONE', #27759, .T. ) ;
#5277 = AXIS2_PLACEMENT_3D ( 'NONE', #16561, #24305, #8808 ) ;
#5278 = CARTESIAN_POINT ( 'NONE',  ( -2.082617625631827174, 3.346456692913386100, 0.3149606299212578953 ) ) ;
#5279 = ORIENTED_EDGE ( 'NONE', *, *, #36053, .F. ) ;
#5280 = DIRECTION ( 'NONE',  ( -3.469446951953613696E-16, 0.000000000000000000, -1.000000000000000000 ) ) ;
#5281 = CARTESIAN_POINT ( 'NONE',  ( 1.560669927219591191, 3.267716535433071279, -5.414661521997678257E-16 ) ) ;
#5282 = CARTESIAN_POINT ( 'NONE',  ( -1.252056778656947422, 1.687847970117562602, -1.807033786809818077 ) ) ;
#5283 = EDGE_CURVE ( 'NONE', #22536, #17189, #5897, .T. ) ;
#5284 = CARTESIAN_POINT ( 'NONE',  ( -1.166969139818015977, 0.000000000000000000, -1.102362204724405270 ) ) ;
#5285 = ORIENTED_EDGE ( 'NONE', *, *, #6185, .F. ) ;
#5286 = ORIENTED_EDGE ( 'NONE', *, *, #5558, .F. ) ;
#5287 = DIRECTION ( 'NONE',  ( -1.000000000000000000, 0.000000000000000000, 0.000000000000000000 ) ) ;
#5288 = CARTESIAN_POINT ( 'NONE',  ( 0.4788131938641112528, 1.726726173772622941, 2.914091152102192162 ) ) ;
#5289 = LINE ( 'NONE', #49380, #41236 ) ;
#5290 = EDGE_CURVE ( 'NONE', #24015, #11634, #33859, .T. ) ;
#5291 = ORIENTED_EDGE ( 'NONE', *, *, #5283, .T. ) ;
#5292 = CARTESIAN_POINT ( 'NONE',  ( 0.07982360342473591996, 1.709180471932028711, 0.000000000000000000 ) ) ;
#5293 = FACE_BOUND ( 'NONE', #48183, .T. ) ;
#5294 = ORIENTED_EDGE ( 'NONE', *, *, #35057, .F. ) ;
#5295 = EDGE_CURVE ( 'NONE', #1759, #12892, #29653, .T. ) ;
#5296 = CARTESIAN_POINT ( 'NONE',  ( -1.946505901478385203, 6.692913385826772199, 0.9915739042680188353 ) ) ;
#5297 = ORIENTED_EDGE ( 'NONE', *, *, #22713, .T. ) ;
#5298 = ORIENTED_EDGE ( 'NONE', *, *, #13965, .F. ) ;
#5299 = DIRECTION ( 'NONE',  ( -0.000000000000000000, 1.000000000000000000, -0.000000000000000000 ) ) ;
#5300 = EDGE_LOOP ( 'NONE', ( #2251, #17374, #13821, #1024 ) ) ;
#5301 = PLANE ( 'NONE',  #35156 ) ;
#5302 = ORIENTED_EDGE ( 'NONE', *, *, #21065, .T. ) ;
#5303 = AXIS2_PLACEMENT_3D ( 'NONE', #29437, #47988, #20922 ) ;
#5304 = VECTOR ( 'NONE', #44224, 39.37007874015748143 ) ;
#5305 = LINE ( 'NONE', #42377, #8148 ) ;
#5306 = FACE_OUTER_BOUND ( 'NONE', #50047, .T. ) ;
#5307 = DIRECTION ( 'NONE',  ( 1.000000000000000000, 0.000000000000000000, 0.000000000000000000 ) ) ;
#5308 = VECTOR ( 'NONE', #12060, 39.37007874015748143 ) ;
#5309 = VECTOR ( 'NONE', #40757, 39.37007874015748143 ) ;
#5310 = B_SPLINE_CURVE_WITH_KNOTS ( 'NONE', 3,
 ( #4060, #36322, #47887, #15918 ),
 .UNSPECIFIED., .F., .F.,
 ( 4, 4 ),
 ( 2.472324174565337688E-07, 0.002500445842694518778 ),
 .UNSPECIFIED. ) ;
#5311 = B_SPLINE_CURVE_WITH_KNOTS ( 'NONE', 3,
 ( #37586, #17953, #41202, #40945 ),
 .UNSPECIFIED., .F., .F.,
 ( 4, 4 ),
 ( 0.03860485074691297896, 0.04008437576871594354 ),
 .UNSPECIFIED. ) ;
#5312 = PLANE ( 'NONE',  #31393 ) ;
#5313 = CARTESIAN_POINT ( 'NONE',  ( -0.04921259842519701277, 1.019748554299324761, 2.583324191532910596 ) ) ;
#5314 = DIRECTION ( 'NONE',  ( 1.000000000000000000, 0.000000000000000000, 0.000000000000000000 ) ) ;
#5315 = AXIS2_PLACEMENT_3D ( 'NONE', #31108, #35234, #13903 ) ;
#5316 = ORIENTED_EDGE ( 'NONE', *, *, #46102, .F. ) ;
#5317 = LINE ( 'NONE', #25700, #44774 ) ;
#5318 = CARTESIAN_POINT ( 'NONE',  ( 1.909347346926324684, 3.267716535433071279, -0.4724409448818889246 ) ) ;
#5319 = ORIENTED_EDGE ( 'NONE', *, *, #37509, .T. ) ;
#5320 = CARTESIAN_POINT ( 'NONE',  ( -1.181102362204724088, 0.000000000000000000, 1.062992125984251413 ) ) ;
#5321 = EDGE_CURVE ( 'NONE', #3351, #1706, #41800, .T. ) ;
#5322 = LINE ( 'NONE', #12307, #46679 ) ;
#5323 = VERTEX_POINT ( 'NONE', #41522 ) ;
#5324 = DIRECTION ( 'NONE',  ( 1.000000000000000000, 0.000000000000000000, 0.000000000000000000 ) ) ;
#5325 = EDGE_CURVE ( 'NONE', #10605, #13662, #13145, .T. ) ;
#5326 = LINE ( 'NONE', #21077, #7803 ) ;
#5327 = EDGE_CURVE ( 'NONE', #39217, #47188, #5652, .T. ) ;
#5328 = CARTESIAN_POINT ( 'NONE',  ( 2.113646359261424745, 1.643330668647667858, -0.9569352356128659753 ) ) ;
#5329 = EDGE_LOOP ( 'NONE', ( #47541, #13338, #10578, #9171 ) ) ;
#5330 = CARTESIAN_POINT ( 'NONE',  ( 0.1968503937007873017, 3.346456692913386100, 0.6299212598425161236 ) ) ;
#5331 = VERTEX_POINT ( 'NONE', #9780 ) ;
#5332 = FACE_BOUND ( 'NONE', #33690, .T. ) ;
#5333 = CARTESIAN_POINT ( 'NONE',  ( 0.1968503937007872462, 3.267716535433071279, 0.1181102362204701633 ) ) ;
#5334 = EDGE_CURVE ( 'NONE', #2753, #32787, #43452, .T. ) ;
#5335 = CARTESIAN_POINT ( 'NONE',  ( 1.636583440222563857, 3.346456692913386100, 0.9448818897637746295 ) ) ;
#5336 = DIRECTION ( 'NONE',  ( 1.000000000000000000, -0.000000000000000000, 0.000000000000000000 ) ) ;
#5337 = ORIENTED_EDGE ( 'NONE', *, *, #34389, .F. ) ;
#5338 = ORIENTED_EDGE ( 'NONE', *, *, #39768, .T. ) ;
#5339 = AXIS2_PLACEMENT_3D ( 'NONE', #4481, #35469, #31598 ) ;
#5340 = CARTESIAN_POINT ( 'NONE',  ( -0.07591351300297277671, 0.000000000000000000, 0.7874015748031456541 ) ) ;
#5341 = EDGE_LOOP ( 'NONE', ( #30961, #25210, #24135, #3080 ) ) ;
#5342 = VECTOR ( 'NONE', #22513, 39.37007874015747433 ) ;
#5343 = EDGE_CURVE ( 'NONE', #7654, #22523, #25266, .T. ) ;
#5344 = CARTESIAN_POINT ( 'NONE',  ( 1.909347346926324684, 3.267716535433071279, -3.312189666507128175E-16 ) ) ;
#5345 = ORIENTED_EDGE ( 'NONE', *, *, #7538, .T. ) ;
#5346 = VECTOR ( 'NONE', #19733, 39.37007874015748143 ) ;
#5347 = DIRECTION ( 'NONE',  ( 1.734723475976806848E-16, 0.000000000000000000, 1.000000000000000000 ) ) ;
#5348 = EDGE_CURVE ( 'NONE', #30262, #18933, #17021, .T. ) ;
#5349 = VERTEX_POINT ( 'NONE', #6156 ) ;
#5350 = PLANE ( 'NONE',  #21669 ) ;
#5351 = ADVANCED_FACE ( 'NONE', ( #49226 ), #29392, .F. ) ;
#5352 = CARTESIAN_POINT ( 'NONE',  ( -0.6383587639822442261, 1.599252270110662399, -2.128056888689588089 ) ) ;
#5353 = AXIS2_PLACEMENT_3D ( 'NONE', #42784, #15927, #43028 ) ;
#5354 = ORIENTED_EDGE ( 'NONE', *, *, #11069, .F. ) ;
#5355 = EDGE_CURVE ( 'NONE', #3576, #41125, #40510, .T. ) ;
#5356 = CARTESIAN_POINT ( 'NONE',  ( 2.734482843737263025, 1.663397001319319113, -1.115254632218672493 ) ) ;
#5357 = ORIENTED_EDGE ( 'NONE', *, *, #47014, .T. ) ;
#5358 = ORIENTED_EDGE ( 'NONE', *, *, #14860, .F. ) ;
#5359 = EDGE_CURVE ( 'NONE', #2219, #44295, #45374, .T. ) ;
#5360 = ORIENTED_EDGE ( 'NONE', *, *, #3125, .F. ) ;
#5361 = ORIENTED_EDGE ( 'NONE', *, *, #22534, .F. ) ;
#5362 = CARTESIAN_POINT ( 'NONE',  ( -0.5455278134075208785, 3.267716535433071279, 1.692913385826762873 ) ) ;
#5363 = DIRECTION ( 'NONE',  ( 1.000000000000000000, -0.000000000000000000, 0.000000000000000000 ) ) ;
#5364 = ORIENTED_EDGE ( 'NONE', *, *, #30856, .T. ) ;
#5365 = DIRECTION ( 'NONE',  ( -0.000000000000000000, -1.000000000000000000, -0.000000000000000000 ) ) ;
#5366 = EDGE_LOOP ( 'NONE', ( #35640, #9215, #9161, #29939 ) ) ;
#5367 = DIRECTION ( 'NONE',  ( 0.000000000000000000, -0.000000000000000000, 1.000000000000000000 ) ) ;
#5368 = CARTESIAN_POINT ( 'NONE',  ( 0.5455278134075208785, 3.346456692913386100, -1.889763779527552812 ) ) ;
#5369 = B_SPLINE_CURVE_WITH_KNOTS ( 'NONE', 3,
 ( #38557, #42164, #6802, #3181 ),
 .UNSPECIFIED., .F., .F.,
 ( 4, 4 ),
 ( 0.03795604549884937229, 0.03924238266445750911 ),
 .UNSPECIFIED. ) ;
#5370 = ORIENTED_EDGE ( 'NONE', *, *, #42658, .T. ) ;
#5371 = DIRECTION ( 'NONE',  ( 1.734723475976806848E-16, -0.000000000000000000, 1.000000000000000000 ) ) ;
#5372 = DIRECTION ( 'NONE',  ( 1.734723475976806848E-16, 0.000000000000000000, 1.000000000000000000 ) ) ;
#5373 = AXIS2_PLACEMENT_3D ( 'NONE', #6716, #34839, #34592 ) ;
#5374 = ORIENTED_EDGE ( 'NONE', *, *, #14610, .F. ) ;
#5375 = DIRECTION ( 'NONE',  ( -1.000000000000000000, 0.000000000000000000, -0.000000000000000000 ) ) ;
#5376 = DIRECTION ( 'NONE',  ( -1.000000000000000000, 0.000000000000000000, 1.734723475976806848E-16 ) ) ;
#5377 = AXIS2_PLACEMENT_3D ( 'NONE', #9544, #17044, #17542 ) ;
#5378 = CARTESIAN_POINT ( 'NONE',  ( 1.766507679922142415, 0.000000000000000000, -1.146458082145294544 ) ) ;
#5379 = CARTESIAN_POINT ( 'NONE',  ( -1.636583440222563635, 3.346456692913386100, -0.1968503937007879123 ) ) ;
#5380 = CARTESIAN_POINT ( 'NONE',  ( 0.9225641151090032688, 1.049866565877818347, -1.802300656674452384 ) ) ;
#5381 = ORIENTED_EDGE ( 'NONE', *, *, #32867, .F. ) ;
#5382 = DIRECTION ( 'NONE',  ( -1.156482317317871478E-16, 0.000000000000000000, -1.000000000000000000 ) ) ;
#5383 = CARTESIAN_POINT ( 'NONE',  ( -1.295932337655932853, 1.699056454769137137, -2.653223682158572405 ) ) ;
#5384 = EDGE_CURVE ( 'NONE', #44282, #2677, #33031, .T. ) ;
#5385 = VECTOR ( 'NONE', #33990, 39.37007874015748143 ) ;
#5386 = ORIENTED_EDGE ( 'NONE', *, *, #49263, .T. ) ;
#5387 = CARTESIAN_POINT ( 'NONE',  ( 0.000000000000000000, 0.000000000000000000, 0.000000000000000000 ) ) ;
#5388 = EDGE_CURVE ( 'NONE', #48506, #47496, #17520, .T. ) ;
#5389 = ORIENTED_EDGE ( 'NONE', *, *, #50451, .T. ) ;
#5390 = DIRECTION ( 'NONE',  ( -0.000000000000000000, 1.000000000000000000, -0.000000000000000000 ) ) ;
#5391 = ADVANCED_FACE ( 'NONE', ( #48212 ), #12887, .F. ) ;
#5392 = CARTESIAN_POINT ( 'NONE',  ( -0.8942052331142547050, 3.346456692913386100, 0.4330708661417290162 ) ) ;
#5393 = DIRECTION ( 'NONE',  ( 1.734723475976806848E-16, -0.000000000000000000, 1.000000000000000000 ) ) ;
#5394 = LINE ( 'NONE', #17278, #24282 ) ;
#5395 = CARTESIAN_POINT ( 'NONE',  ( -2.160844847985643025, 1.574872742815768500, 0.1614166013721432535 ) ) ;
#5396 = EDGE_LOOP ( 'NONE', ( #3777, #3072, #27859 ) ) ;
#5397 = CARTESIAN_POINT ( 'NONE',  ( 0.000000000000000000, 3.267716535433071279, 0.4330708661417290162 ) ) ;
#5398 = FACE_OUTER_BOUND ( 'NONE', #5721, .T. ) ;
#5399 = VERTEX_POINT ( 'NONE', #20880 ) ;
#5400 = CARTESIAN_POINT ( 'NONE',  ( 1.183645401082124904, 0.000000000000000000, 1.279993023352361980 ) ) ;
#5401 = ORIENTED_EDGE ( 'NONE', *, *, #39602, .T. ) ;
#5402 = CARTESIAN_POINT ( 'NONE',  ( -0.07591351300297337346, 3.267716535433071279, 2.633779063002570064E-17 ) ) ;
#5403 = FACE_OUTER_BOUND ( 'NONE', #18199, .T. ) ;
#5404 = EDGE_CURVE ( 'NONE', #25030, #21072, #46214, .T. ) ;
#5405 = CARTESIAN_POINT ( 'NONE',  ( -1.091055626815042867, 3.267716535433071279, 1.892679809432645129E-16 ) ) ;
#5406 = CARTESIAN_POINT ( 'NONE',  ( -1.450036433410862635, 0.001605425820709399697, -1.016128049641541020 ) ) ;
#5407 = AXIS2_PLACEMENT_3D ( 'NONE', #31730, #16494, #7974 ) ;
#5408 = EDGE_CURVE ( 'NONE', #22325, #18373, #19032, .T. ) ;
#5409 = ORIENTED_EDGE ( 'NONE', *, *, #6278, .T. ) ;
#5410 = ORIENTED_EDGE ( 'NONE', *, *, #14891, .F. ) ;
#5411 = VECTOR ( 'NONE', #38708, 39.37007874015748143 ) ;
#5412 = ADVANCED_FACE ( 'NONE', ( #42030 ), #42274, .F. ) ;
#5413 = CARTESIAN_POINT ( 'NONE',  ( -0.2727639067037602172, 0.000000000000000000, 0.7874015748031456541 ) ) ;
#5414 = CARTESIAN_POINT ( 'NONE',  ( -0.8942052331142552601, 3.267716535433071279, -1.456692913385822186 ) ) ;
#5415 = FACE_BOUND ( 'NONE', #16739, .T. ) ;
#5416 = VERTEX_POINT ( 'NONE', #46629 ) ;
#5417 = VECTOR ( 'NONE', #19101, 39.37007874015748143 ) ;
#5418 = DIRECTION ( 'NONE',  ( -1.000000000000000000, 0.000000000000000000, 0.000000000000000000 ) ) ;
#5419 = CARTESIAN_POINT ( 'NONE',  ( -1.461782879395278512, 5.905511811023623991, -1.598346982901828639 ) ) ;
#5420 = VECTOR ( 'NONE', #40593, 39.37007874015748143 ) ;
#5421 = ORIENTED_EDGE ( 'NONE', *, *, #26158, .F. ) ;
#5422 = DIRECTION ( 'NONE',  ( 0.000000000000000000, -1.000000000000000000, -0.000000000000000000 ) ) ;
#5423 = VECTOR ( 'NONE', #12187, 39.37007874015748143 ) ;
#5424 = DIRECTION ( 'NONE',  ( 1.000000000000000000, 0.000000000000000000, 0.000000000000000000 ) ) ;
#5425 = ORIENTED_EDGE ( 'NONE', *, *, #4126, .F. ) ;
#5426 = ORIENTED_EDGE ( 'NONE', *, *, #11216, .F. ) ;
#5427 = ORIENTED_EDGE ( 'NONE', *, *, #20800, .F. ) ;
#5428 = DIRECTION ( 'NONE',  ( 1.000000000000000000, 0.000000000000000000, 0.000000000000000000 ) ) ;
#5429 = DIRECTION ( 'NONE',  ( 0.000000000000000000, 1.000000000000000000, 0.000000000000000000 ) ) ;
#5430 = DIRECTION ( 'NONE',  ( -0.01601477604151182663, 0.9998717552508123996, -0.000000000000000000 ) ) ;
#5431 = DIRECTION ( 'NONE',  ( 0.000000000000000000, -1.000000000000000000, 0.000000000000000000 ) ) ;
#5432 = EDGE_LOOP ( 'NONE', ( #12568, #43738, #18292, #7640, #49921 ) ) ;
#5433 = VERTEX_POINT ( 'NONE', #14917 ) ;
#5434 = DIRECTION ( 'NONE',  ( -0.000000000000000000, 1.000000000000000000, -0.000000000000000000 ) ) ;
#5435 = CARTESIAN_POINT ( 'NONE',  ( 1.287906020515829919, 3.346456692913386100, -1.456692913385822630 ) ) ;
#5436 = DIRECTION ( 'NONE',  ( 2.891205793294678326E-16, 0.000000000000000000, -1.000000000000000000 ) ) ;
#5437 = DIRECTION ( 'NONE',  ( -0.000000000000000000, 1.000000000000000000, -0.000000000000000000 ) ) ;
#5438 = DIRECTION ( 'NONE',  ( -3.469446951953613696E-16, 0.000000000000000000, -1.000000000000000000 ) ) ;
#5439 = DIRECTION ( 'NONE',  ( -0.000000000000000000, 1.000000000000000000, -0.000000000000000000 ) ) ;
#5440 = VECTOR ( 'NONE', #31863, 39.37007874015748143 ) ;
#5441 = CARTESIAN_POINT ( 'NONE',  ( 0.000000000000000000, 3.346456692913386100, 0.000000000000000000 ) ) ;
#5442 = EDGE_CURVE ( 'NONE', #42803, #9319, #22913, .T. ) ;
#5443 = ORIENTED_EDGE ( 'NONE', *, *, #8590, .T. ) ;
#5444 = AXIS2_PLACEMENT_3D ( 'NONE', #38534, #6779, #34158 ) ;
#5445 = CARTESIAN_POINT ( 'NONE',  ( -0.3500732549360408563, 1.603869690133923331, 2.204675616574417685 ) ) ;
#5446 = CARTESIAN_POINT ( 'NONE',  ( 0.1067246931122726866, 0.02962905676920215767, 0.000000000000000000 ) ) ;
#5447 = EDGE_CURVE ( 'NONE', #8302, #39762, #6914, .T. ) ;
#5448 = AXIS2_PLACEMENT_3D ( 'NONE', #17441, #17951, #13317 ) ;
#5449 = ORIENTED_EDGE ( 'NONE', *, *, #30336, .F. ) ;
#5450 = AXIS2_PLACEMENT_3D ( 'NONE', #31632, #43486, #47332 ) ;
#5451 = EDGE_CURVE ( 'NONE', #46412, #45936, #14154, .T. ) ;
#5452 = ORIENTED_EDGE ( 'NONE', *, *, #44665, .T. ) ;
#5453 = FACE_OUTER_BOUND ( 'NONE', #44923, .T. ) ;
#5454 = CARTESIAN_POINT ( 'NONE',  ( 2.867773316779195447, 5.118110236220475784, -0.7050287376752000235 ) ) ;
#5455 = EDGE_CURVE ( 'NONE', #3016, #39431, #30921, .T. ) ;
#5456 = VECTOR ( 'NONE', #25933, 39.37007874015748143 ) ;
#5457 = ORIENTED_EDGE ( 'NONE', *, *, #12375, .F. ) ;
#5458 = EDGE_CURVE ( 'NONE', #1865, #39550, #12261, .T. ) ;
#5459 = AXIS2_PLACEMENT_3D ( 'NONE', #50993, #20321, #43552 ) ;
#5460 = ORIENTED_EDGE ( 'NONE', *, *, #22631, .T. ) ;
#5461 = FACE_OUTER_BOUND ( 'NONE', #13168, .T. ) ;
#5462 = ORIENTED_EDGE ( 'NONE', *, *, #50380, .T. ) ;
#5463 = CARTESIAN_POINT ( 'NONE',  ( -0.9602959360900468200, 0.01253876862113688373, 1.511314840084332145 ) ) ;
#5464 = CARTESIAN_POINT ( 'NONE',  ( -2.142325647309101022, 3.346456692913386100, 0.3149606299212578953 ) ) ;
#5465 = EDGE_CURVE ( 'NONE', #2174, #9322, #29904, .T. ) ;
#5466 = ORIENTED_EDGE ( 'NONE', *, *, #45239, .F. ) ;
#5467 = VERTEX_POINT ( 'NONE', #18032 ) ;
#5468 = ORIENTED_EDGE ( 'NONE', *, *, #6520, .T. ) ;
#5469 = CARTESIAN_POINT ( 'NONE',  ( 0.000000000000000000, 3.267716535433071279, 0.000000000000000000 ) ) ;
#5470 = EDGE_LOOP ( 'NONE', ( #3066, #26099, #48653 ) ) ;
#5471 = ORIENTED_EDGE ( 'NONE', *, *, #7047, .T. ) ;
#5472 = EDGE_CURVE ( 'NONE', #162, #21208, #42433, .T. ) ;
#5473 = CARTESIAN_POINT ( 'NONE',  ( -1.985260859929297794, 3.267716535433071279, 6.887757239314512246E-16 ) ) ;
#5474 = LINE ( 'NONE', #5213, #2178 ) ;
#5475 = DIRECTION ( 'NONE',  ( 7.815966141386463688E-14, 0.000000000000000000, 1.000000000000000000 ) ) ;
#5476 = ORIENTED_EDGE ( 'NONE', *, *, #24195, .F. ) ;
#5477 = LINE ( 'NONE', #36984, #14738 ) ;
#5478 = CARTESIAN_POINT ( 'NONE',  ( -0.5455278134075208785, 3.346456692913386100, 0.9448818897637749625 ) ) ;
#5479 = ADVANCED_FACE ( 'NONE', ( #2791 ), #30157, .F. ) ;
#5480 = CARTESIAN_POINT ( 'NONE',  ( -2.061297163897529483, 3.346456692913386100, 0.4330708661417290162 ) ) ;
#5481 = AXIS2_PLACEMENT_3D ( 'NONE', #48391, #39926, #27785 ) ;
#5482 = ORIENTED_EDGE ( 'NONE', *, *, #4347, .F. ) ;
#5483 = CARTESIAN_POINT ( 'NONE',  ( 1.909347346926324684, 0.000000000000000000, 0.1574803149606280872 ) ) ;
#5484 = DIRECTION ( 'NONE',  ( 0.000000000000000000, 0.000000000000000000, -1.000000000000000000 ) ) ;
#5485 = VECTOR ( 'NONE', #23379, 39.37007874015748143 ) ;
#5486 = VECTOR ( 'NONE', #13826, 39.37007874015748143 ) ;
#5487 = CARTESIAN_POINT ( 'NONE',  ( 0.4696143004045484903, 0.000000000000000000, 1.732283464566921172 ) ) ;
#5488 = ORIENTED_EDGE ( 'NONE', *, *, #39318, .T. ) ;
#5489 = ORIENTED_EDGE ( 'NONE', *, *, #36807, .T. ) ;
#5490 =( CONVERSION_BASED_UNIT ( 'INCH', #41369 ) LENGTH_UNIT ( ) NAMED_UNIT ( #28098 ) );
#5491 = ADVANCED_FACE ( 'NONE', ( #45616 ), #31394, .T. ) ;
#5492 = VECTOR ( 'NONE', #30050, 39.37007874015748143 ) ;
#5493 = LINE ( 'NONE', #21240, #44537 ) ;
#5494 = VECTOR ( 'NONE', #10790, 39.37007874015748143 ) ;
#5495 = DIRECTION ( 'NONE',  ( -0.000000000000000000, 1.000000000000000000, -0.000000000000000000 ) ) ;
#5496 = CARTESIAN_POINT ( 'NONE',  ( 1.780101451746607610, 5.905511811023623991, 1.234002060668518919 ) ) ;
#5497 = ORIENTED_EDGE ( 'NONE', *, *, #27556, .F. ) ;
#5498 = ORIENTED_EDGE ( 'NONE', *, *, #37642, .T. ) ;
#5499 = CONICAL_SURFACE ( 'NONE', #21165, 3.033577403570480779, 1.554780866114618743 ) ;
#5500 = DIRECTION ( 'NONE',  ( -0.000000000000000000, 1.000000000000000000, -0.000000000000000000 ) ) ;
#5501 = ORIENTED_EDGE ( 'NONE', *, *, #5701, .T. ) ;
#5502 = DIRECTION ( 'NONE',  ( 1.000000000000000000, 0.000000000000000000, -3.469446951953613696E-16 ) ) ;
#5503 = CARTESIAN_POINT ( 'NONE',  ( -0.07591351300297333182, 3.346456692913386100, 2.362204724409437961 ) ) ;
#5504 = LINE ( 'NONE', #1113, #29147 ) ;
#5506 = LINE ( 'NONE', #21765, #13707 ) ;
#5505 = APPLICATION_CONTEXT ( 'automotive_design' ) ;
#5507 = CARTESIAN_POINT ( 'NONE',  ( 1.363819533518803029, 0.000000000000000000, -1.102362204724405714 ) ) ;
#5508 = ORIENTED_EDGE ( 'NONE', *, *, #826, .F. ) ;
#5509 = CARTESIAN_POINT ( 'NONE',  ( -1.712496953225538077, 3.267716535433071279, 5.941417334598193996E-16 ) ) ;
#5510 = CARTESIAN_POINT ( 'NONE',  ( 1.287906020515830585, 3.346456692913386100, 1.574803149606291974 ) ) ;
#5511 = EDGE_CURVE ( 'NONE', #3209, #45101, #10280, .T. ) ;
#5512 = EDGE_LOOP ( 'NONE', ( #5226, #25154, #10758, #5497 ) ) ;
#5513 = FACE_OUTER_BOUND ( 'NONE', #12305, .T. ) ;
#5514 = CARTESIAN_POINT ( 'NONE',  ( -2.139229417893220297, 6.692913385826772199, -0.3394403656973701833 ) ) ;
#5515 = DIRECTION ( 'NONE',  ( 1.000000000000000000, -0.000000000000000000, 0.000000000000000000 ) ) ;
#5516 = EDGE_CURVE ( 'NONE', #28782, #4720, #26028, .T. ) ;
#5517 = ORIENTED_EDGE ( 'NONE', *, *, #39704, .T. ) ;
#5518 = VECTOR ( 'NONE', #20562, 39.37007874015748143 ) ;
#5519 = CARTESIAN_POINT ( 'NONE',  ( -0.2727639067037602172, 3.267716535433071279, 1.102362204724404160 ) ) ;
#5520 = ADVANCED_FACE ( 'NONE', ( #26528 ), #46377, .F. ) ;
#5521 = DIRECTION ( 'NONE',  ( 0.9998717552508121775, 0.01601477604151182663, 0.000000000000000000 ) ) ;
#5522 = VECTOR ( 'NONE', #36620, 39.37007874015748854 ) ;
#5523 = VERTEX_POINT ( 'NONE', #26779 ) ;
#5524 = CARTESIAN_POINT ( 'NONE',  ( 0.7423782071083084855, 3.267716535433071279, -2.034117492951036166 ) ) ;
#5525 = CARTESIAN_POINT ( 'NONE',  ( 2.168245791271197209, 1.466194936398640181, -2.004968704497248400 ) ) ;
#5526 = ORIENTED_EDGE ( 'NONE', *, *, #22982, .T. ) ;
#5527 = LINE ( 'NONE', #21278, #32807 ) ;
#5528 = DIRECTION ( 'NONE',  ( 0.000000000000000000, 0.000000000000000000, 1.000000000000000000 ) ) ;
#5529 = DIRECTION ( 'NONE',  ( -3.469446951953613696E-16, 0.000000000000000000, -1.000000000000000000 ) ) ;
#5530 = LINE ( 'NONE', #33679, #21094 ) ;
#5531 = VECTOR ( 'NONE', #18890, 39.37007874015748143 ) ;
#5532 = LINE ( 'NONE', #37549, #27912 ) ;
#5533 = ORIENTED_EDGE ( 'NONE', *, *, #8314, .T. ) ;
#5534 = ORIENTED_EDGE ( 'NONE', *, *, #6836, .T. ) ;
#5535 = CARTESIAN_POINT ( 'NONE',  ( -1.695772546416001836, 1.692832103184166437, -2.417756147381374010 ) ) ;
#5536 = FACE_OUTER_BOUND ( 'NONE', #42874, .T. ) ;
#5537 = ORIENTED_EDGE ( 'NONE', *, *, #24850, .T. ) ;
#5538 = CARTESIAN_POINT ( 'NONE',  ( -2.494543283151989144, 1.577876278647536434, -1.012699542302954114 ) ) ;
#5539 = PLANE ( 'NONE',  #45853 ) ;
#5540 = DIRECTION ( 'NONE',  ( -0.000000000000000000, 0.000000000000000000, 1.000000000000000000 ) ) ;
#5541 = LINE ( 'NONE', #10371, #11636 ) ;
#5542 = ORIENTED_EDGE ( 'NONE', *, *, #22942, .F. ) ;
#5543 = VERTEX_POINT ( 'NONE', #3289 ) ;
#5544 = LINE ( 'NONE', #36791, #36968 ) ;
#5545 = CARTESIAN_POINT ( 'NONE',  ( 0.5433756366782908076, 1.727723484189010561, 2.902374796132115353 ) ) ;
#5546 = ADVANCED_FACE ( 'NONE', ( #34042 ), #34793, .F. ) ;
#5547 = LINE ( 'NONE', #40665, #50233 ) ;
#5548 = ORIENTED_EDGE ( 'NONE', *, *, #28138, .F. ) ;
#5549 = LINE ( 'NONE', #28264, #23198 ) ;
#5550 = FACE_BOUND ( 'NONE', #45091, .T. ) ;
#5551 = ORIENTED_EDGE ( 'NONE', *, *, #45589, .T. ) ;
#5552 = CARTESIAN_POINT ( 'NONE',  ( 1.636583440222563857, 0.000000000000000000, -0.1968503937007886062 ) ) ;
#5553 = ORIENTED_EDGE ( 'NONE', *, *, #15762, .F. ) ;
#5554 = ORIENTED_EDGE ( 'NONE', *, *, #23913, .F. ) ;
#5555 = CARTESIAN_POINT ( 'NONE',  ( 0.2727639067037604947, 3.346456692913386100, 0.1574803149606283648 ) ) ;
#5556 = EDGE_CURVE ( 'NONE', #5087, #40355, #45873, .T. ) ;
#5557 = AXIS2_PLACEMENT_3D ( 'NONE', #14501, #26117, #14239 ) ;
#5558 = EDGE_CURVE ( 'NONE', #18488, #26431, #19789, .T. ) ;
#5559 = VECTOR ( 'NONE', #19967, 39.37007874015748143 ) ;
#5560 = VERTEX_POINT ( 'NONE', #19534 ) ;
#5561 = FACE_OUTER_BOUND ( 'NONE', #41020, .T. ) ;
#5562 = DIRECTION ( 'NONE',  ( -1.000000000000000000, 0.000000000000000000, 0.000000000000000000 ) ) ;
#5563 = ORIENTED_EDGE ( 'NONE', *, *, #25909, .F. ) ;
#5564 = VECTOR ( 'NONE', #931, 39.37007874015748143 ) ;
#5565 = EDGE_CURVE ( 'NONE', #15453, #33477, #15923, .T. ) ;
#5566 = DIRECTION ( 'NONE',  ( 1.734723475976806848E-16, 0.000000000000000000, 1.000000000000000000 ) ) ;
#5567 = DIRECTION ( 'NONE',  ( 0.000000000000000000, -1.000000000000000000, 0.000000000000000000 ) ) ;
#5568 = LINE ( 'NONE', #1946, #4487 ) ;
#5569 = ADVANCED_FACE ( 'NONE', ( #32201 ), #43536, .F. ) ;
#5570 = DIRECTION ( 'NONE',  ( -1.000000000000000000, 0.000000000000000000, -0.000000000000000000 ) ) ;
#5571 = CARTESIAN_POINT ( 'NONE',  ( -0.04921259842519688094, 0.02713143566191717967, 1.843522435433914142 ) ) ;
#5572 = DIRECTION ( 'NONE',  ( -1.000000000000000000, 0.000000000000000000, 1.734723475976806848E-16 ) ) ;
#5573 = ORIENTED_EDGE ( 'NONE', *, *, #29977, .T. ) ;
#5574 = DIRECTION ( 'NONE',  ( -1.000000000000000000, 0.000000000000000000, 0.000000000000000000 ) ) ;
#5575 = VECTOR ( 'NONE', #17446, 39.37007874015748143 ) ;
#5576 = DIRECTION ( 'NONE',  ( -0.000000000000000000, 1.000000000000000000, -0.000000000000000000 ) ) ;
#5577 = ADVANCED_FACE ( 'NONE', ( #50982 ), #23979, .T. ) ;
#5578 = ORIENTED_EDGE ( 'NONE', *, *, #44701, .T. ) ;
#5579 = CARTESIAN_POINT ( 'NONE',  ( 2.378961647330872786, 3.346456692913386100, -1.161035397307311917E-15 ) ) ;
#5580 = CARTESIAN_POINT ( 'NONE',  ( 0.5455278134075217666, 3.346456692913386100, 2.204724409448808764 ) ) ;
#5581 = EDGE_LOOP ( 'NONE', ( #49168, #3951, #14563, #20212 ) ) ;
#5582 = CARTESIAN_POINT ( 'NONE',  ( -0.2727639067037602172, 3.346456692913386100, 2.047244094488179567 ) ) ;
#5583 = DIRECTION ( 'NONE',  ( -0.000000000000000000, 1.000000000000000000, -0.000000000000000000 ) ) ;
#5584 = EDGE_CURVE ( 'NONE', #5934, #3813, #21499, .T. ) ;
#5585 = CARTESIAN_POINT ( 'NONE',  ( -1.985260859929297794, 3.267716535433071279, 0.1181102362204704270 ) ) ;
#5586 = ORIENTED_EDGE ( 'NONE', *, *, #39418, .T. ) ;
#5587 = LINE ( 'NONE', #29594, #12534 ) ;
#5588 = ORIENTED_EDGE ( 'NONE', *, *, #11493, .F. ) ;
#5589 = FACE_BOUND ( 'NONE', #5621, .T. ) ;
#5590 = DIRECTION ( 'NONE',  ( 0.000000000000000000, 0.000000000000000000, -1.000000000000000000 ) ) ;
#5591 = FACE_OUTER_BOUND ( 'NONE', #2418, .T. ) ;
#5592 = CARTESIAN_POINT ( 'NONE',  ( -0.2480359799030329715, -0.6299212598425202314, 0.2799391584775194342 ) ) ;
#5593 = CONICAL_SURFACE ( 'NONE', #26193, 2.246510896728926010, 0.01601546068027819014 ) ;
#5594 = VECTOR ( 'NONE', #45178, 39.37007874015748854 ) ;
#5595 = EDGE_CURVE ( 'NONE', #41400, #1980, #11594, .T. ) ;
#5596 = VERTEX_POINT ( 'NONE', #23669 ) ;
#5597 = ORIENTED_EDGE ( 'NONE', *, *, #18684, .F. ) ;
#5598 = PLANE ( 'NONE',  #47664 ) ;
#5599 = ORIENTED_EDGE ( 'NONE', *, *, #35021, .T. ) ;
#5600 = VECTOR ( 'NONE', #41551, 39.37007874015748143 ) ;
#5601 = CARTESIAN_POINT ( 'NONE',  ( 0.000000000000000000, 3.267716535433071279, -7.512581982576723358E-16 ) ) ;
#5602 = VERTEX_POINT ( 'NONE', #39423 ) ;
#5603 = CARTESIAN_POINT ( 'NONE',  ( -1.091055626815042645, 0.000000000000000000, 1.889763779527550147 ) ) ;
#5604 = VECTOR ( 'NONE', #9021, 39.37007874015748143 ) ;
#5605 = VERTEX_POINT ( 'NONE', #43023 ) ;
#5606 = DIRECTION ( 'NONE',  ( -1.000000000000000000, 0.000000000000000000, 1.734723475976806848E-16 ) ) ;
#5607 = EDGE_CURVE ( 'NONE', #15116, #19912, #39679, .T. ) ;
#5608 = VECTOR ( 'NONE', #10818, 39.37007874015748143 ) ;
#5609 = FACE_OUTER_BOUND ( 'NONE', #18671, .T. ) ;
#5610 = ORIENTED_EDGE ( 'NONE', *, *, #50282, .T. ) ;
#5611 = CARTESIAN_POINT ( 'NONE',  ( 0.5272349255864849926, 0.000000000000000000, 2.905303903342417726 ) ) ;
#5612 = ORIENTED_EDGE ( 'NONE', *, *, #44908, .T. ) ;
#5613 = ORIENTED_EDGE ( 'NONE', *, *, #48081, .F. ) ;
#5614 = AXIS2_PLACEMENT_3D ( 'NONE', #14017, #45481, #37777 ) ;
#5615 = EDGE_CURVE ( 'NONE', #1023, #48695, #35552, .T. ) ;
#5616 = EDGE_CURVE ( 'NONE', #18320, #7706, #50726, .T. ) ;
#5617 = ORIENTED_EDGE ( 'NONE', *, *, #4353, .F. ) ;
#5618 = ORIENTED_EDGE ( 'NONE', *, *, #26359, .T. ) ;
#5619 = DIRECTION ( 'NONE',  ( -3.469446951953613696E-16, 0.000000000000000000, -1.000000000000000000 ) ) ;
#5620 = EDGE_CURVE ( 'NONE', #22725, #35907, #47640, .T. ) ;
#5621 = EDGE_LOOP ( 'NONE', ( #11871, #35566, #49419, #4006 ) ) ;
#5622 = CARTESIAN_POINT ( 'NONE',  ( 0.2727639067037607168, 3.267716535433071279, -4.731699523581612823E-17 ) ) ;
#5623 = ORIENTED_EDGE ( 'NONE', *, *, #32381, .F. ) ;
#5624 = CARTESIAN_POINT ( 'NONE',  ( -0.2727639067037607723, 3.346456692913386100, 2.362204724409437961 ) ) ;
#5625 = VECTOR ( 'NONE', #19664, 39.37007874015748143 ) ;
#5626 = CARTESIAN_POINT ( 'NONE',  ( 0.07982360342473591996, 1.709180471932028711, 0.000000000000000000 ) ) ;
#5627 = ORIENTED_EDGE ( 'NONE', *, *, #3867, .T. ) ;
#5628 = CARTESIAN_POINT ( 'NONE',  ( 0.000000000000000000, 3.267716535433071279, 0.7874015748031456541 ) ) ;
#5629 = CARTESIAN_POINT ( 'NONE',  ( 2.724759210110882179, 1.758266479573719510, 0.3194316615506513357 ) ) ;
#5630 = ORIENTED_EDGE ( 'NONE', *, *, #556, .T. ) ;
#5631 = CARTESIAN_POINT ( 'NONE',  ( -0.5455278134075214336, 3.346456692913386100, 2.007874015748021268 ) ) ;
#5632 = DIRECTION ( 'NONE',  ( -3.469446951953613696E-16, 0.000000000000000000, -1.000000000000000000 ) ) ;
#5633 = AXIS2_PLACEMENT_3D ( 'NONE', #31452, #47148, #7953 ) ;
#5634 = EDGE_CURVE ( 'NONE', #26534, #660, #43281, .T. ) ;
#5635 = LINE ( 'NONE', #41265, #1279 ) ;
#5636 = CARTESIAN_POINT ( 'NONE',  ( 0.7423782071083087075, 3.346456692913386100, -6.146657985744592735E-16 ) ) ;
#5637 = AXIS2_PLACEMENT_3D ( 'NONE', #9163, #16664, #650 ) ;
#5638 = VECTOR ( 'NONE', #20379, 39.37007874015748143 ) ;
#5639 = EDGE_CURVE ( 'NONE', #19400, #26179, #35047, .T. ) ;
#5640 = CARTESIAN_POINT ( 'NONE',  ( 0.000000000000000000, 3.346456692913386100, 0.000000000000000000 ) ) ;
#5641 = ORIENTED_EDGE ( 'NONE', *, *, #39675, .T. ) ;
#5642 = DIRECTION ( 'NONE',  ( -3.469446951953613696E-16, 0.000000000000000000, -1.000000000000000000 ) ) ;
#5643 = CARTESIAN_POINT ( 'NONE',  ( 1.015142113812069979, 3.346456692913386100, 1.732283464566921172 ) ) ;
#5644 = EDGE_CURVE ( 'NONE', #26643, #48342, #32473, .T. ) ;
#5645 = VECTOR ( 'NONE', #20343, 39.37007874015748143 ) ;
#5646 = ORIENTED_EDGE ( 'NONE', *, *, #23323, .T. ) ;
#5647 = CARTESIAN_POINT ( 'NONE',  ( 1.687984952120843207, 3.346456692913386100, -1.259842519685035800 ) ) ;
#5648 = EDGE_CURVE ( 'NONE', #30555, #2803, #8444, .T. ) ;
#5649 = EDGE_CURVE ( 'NONE', #43058, #23763, #11545, .T. ) ;
#5650 = CIRCLE ( 'NONE', #25434, 1.181102362204723200 ) ;
#5651 = ORIENTED_EDGE ( 'NONE', *, *, #914, .F. ) ;
#5652 = LINE ( 'NONE', #9521, #10499 ) ;
#5653 = DIRECTION ( 'NONE',  ( 5.779879058772725700E-18, 1.000000000000000000, -1.286990067732317241E-16 ) ) ;
#5654 = LINE ( 'NONE', #48214, #29508 ) ;
#5655 = PLANE ( 'NONE',  #41610 ) ;
#5656 = DIRECTION ( 'NONE',  ( 0.000000000000000000, 0.000000000000000000, 1.000000000000000000 ) ) ;
#5657 = ORIENTED_EDGE ( 'NONE', *, *, #15972, .F. ) ;
#5658 = CARTESIAN_POINT ( 'NONE',  ( -2.491402175429631605, 1.680428061220146096, -1.585592796919542025 ) ) ;
#5659 = FACE_BOUND ( 'NONE', #821, .T. ) ;
#5660 = CARTESIAN_POINT ( 'NONE',  ( 2.078641700530069691, 0.5219575377975975705, -0.9419735264436572830 ) ) ;
#5661 = VERTEX_POINT ( 'NONE', #31421 ) ;
#5662 = DIRECTION ( 'NONE',  ( -3.986037398843765983E-20, -1.000000000000000000, -1.160734090543304660E-16 ) ) ;
#5663 = VERTEX_POINT ( 'NONE', #47123 ) ;
#5664 = CARTESIAN_POINT ( 'NONE',  ( 1.363819533518803029, 0.000000000000000000, -1.929133858267710666 ) ) ;
#5665 = DIRECTION ( 'NONE',  ( 0.000000000000000000, -1.000000000000000000, 0.000000000000000000 ) ) ;
#5666 = AXIS2_PLACEMENT_3D ( 'NONE', #16907, #44756, #1151 ) ;
#5667 = CARTESIAN_POINT ( 'NONE',  ( -2.106299212598425008, 3.267716535433071279, -6.146657985744592735E-16 ) ) ;
#5668 = LINE ( 'NONE', #35880, #40388 ) ;
#5669 = VERTEX_POINT ( 'NONE', #7926 ) ;
#5670 = VERTEX_POINT ( 'NONE', #12316 ) ;
#5671 = DIRECTION ( 'NONE',  ( -0.000000000000000000, 1.000000000000000000, -0.000000000000000000 ) ) ;
#5672 = CARTESIAN_POINT ( 'NONE',  ( -2.996855935080999345, 2.755905511811027164, 0.1838511574193319453 ) ) ;
#5673 = FACE_BOUND ( 'NONE', #43440, .T. ) ;
#5674 = ORIENTED_EDGE ( 'NONE', *, *, #27184, .F. ) ;
#5675 = CONICAL_SURFACE ( 'NONE', #6530, 3.483074324928249421, 1.244861948955335196 ) ;
#5676 = AXIS2_PLACEMENT_3D ( 'NONE', #23478, #39746, #46696 ) ;
#5677 = DIRECTION ( 'NONE',  ( 0.01601477604151182663, -0.9998717552508123996, 0.000000000000000000 ) ) ;
#5678 = DIRECTION ( 'NONE',  ( -3.469446951953613696E-16, 0.000000000000000000, -1.000000000000000000 ) ) ;
#5679 = EDGE_CURVE ( 'NONE', #12398, #21285, #24191, .T. ) ;
#5680 = ORIENTED_EDGE ( 'NONE', *, *, #50176, .F. ) ;
#5681 = EDGE_LOOP ( 'NONE', ( #278, #27334, #44209, #46752 ) ) ;
#5682 = AXIS2_PLACEMENT_3D ( 'NONE', #5699, #48762, #20929 ) ;
#5683 = DIRECTION ( 'NONE',  ( -0.000000000000000000, -1.000000000000000000, -0.000000000000000000 ) ) ;
#5684 = EDGE_CURVE ( 'NONE', #23466, #8911, #36069, .T. ) ;
#5685 = EDGE_CURVE ( 'NONE', #122, #48282, #3439, .T. ) ;
#5686 = DIRECTION ( 'NONE',  ( 0.8660254037844432595, 0.000000000000000000, 0.4999999999999920064 ) ) ;
#5687 = ORIENTED_EDGE ( 'NONE', *, *, #26874, .F. ) ;
#5688 = ORIENTED_EDGE ( 'NONE', *, *, #26874, .T. ) ;
#5689 = VECTOR ( 'NONE', #5515, 39.37007874015748143 ) ;
#5690 = EDGE_CURVE ( 'NONE', #21621, #8302, #20086, .T. ) ;
#5691 = ORIENTED_EDGE ( 'NONE', *, *, #39666, .F. ) ;
#5692 = DIRECTION ( 'NONE',  ( 0.000000000000000000, 0.000000000000000000, 1.000000000000000000 ) ) ;
#5693 = CARTESIAN_POINT ( 'NONE',  ( 1.566245445154855531, 1.172985819482486924, -0.9842519685039369248 ) ) ;
#5694 = CARTESIAN_POINT ( 'NONE',  ( 0.000000000000000000, 3.267716535433071279, -1.299212598425193210 ) ) ;
#5695 = DIRECTION ( 'NONE',  ( -0.01601477604151182663, 0.9998717552508123996, -0.000000000000000000 ) ) ;
#5696 = ORIENTED_EDGE ( 'NONE', *, *, #4983, .T. ) ;
#5697 = VERTEX_POINT ( 'NONE', #34935 ) ;
#5698 = CARTESIAN_POINT ( 'NONE',  ( -2.182111253630085290, 0.000000000000000000, 0.6299212598425164567 ) ) ;
#5699 = CARTESIAN_POINT ( 'NONE',  ( 0.000000000000000000, 0.000000000000000000, 0.000000000000000000 ) ) ;
#5700 = DIRECTION ( 'NONE',  ( -0.000000000000000000, 0.000000000000000000, 1.000000000000000000 ) ) ;
#5701 = EDGE_CURVE ( 'NONE', #51000, #29752, #50616, .T. ) ;
#5702 = LINE ( 'NONE', #21448, #9504 ) ;
#5703 = EDGE_CURVE ( 'NONE', #35551, #13057, #29735, .T. ) ;
#5704 = DIRECTION ( 'NONE',  ( 1.000000000000000000, -0.000000000000000000, 0.000000000000000000 ) ) ;
#5705 = VECTOR ( 'NONE', #45193, 39.37007874015748143 ) ;
#5706 = DIRECTION ( 'NONE',  ( -1.000000000000000000, 0.000000000000000000, 1.734723475976806848E-16 ) ) ;
#5707 = ORIENTED_EDGE ( 'NONE', *, *, #46799, .T. ) ;
#5708 = CARTESIAN_POINT ( 'NONE',  ( -2.182111253630085290, 0.000000000000000000, -0.3149606299212589500 ) ) ;
#5709 = CARTESIAN_POINT ( 'NONE',  ( -2.734482843737247038, 1.572033689214636709, -1.115254632218712016 ) ) ;
#5710 = EDGE_CURVE ( 'NONE', #15688, #17158, #2934, .T. ) ;
#5711 = ORIENTED_EDGE ( 'NONE', *, *, #14378, .F. ) ;
#5712 = EDGE_LOOP ( 'NONE', ( #6613, #41284, #13089, #11024 ) ) ;
#5714 = FACE_OUTER_BOUND ( 'NONE', #3774, .T. ) ;
#5713 = AXIS2_PLACEMENT_3D ( 'NONE', #33458, #10707, #9693 ) ;
#5715 = FACE_OUTER_BOUND ( 'NONE', #1698, .T. ) ;
#5716 = ORIENTED_EDGE ( 'NONE', *, *, #19757, .F. ) ;
#5717 = AXIS2_PLACEMENT_3D ( 'NONE', #28753, #29265, #14032 ) ;
#5718 = ORIENTED_EDGE ( 'NONE', *, *, #40325, .F. ) ;
#5719 = DIRECTION ( 'NONE',  ( 1.000000000000000000, 0.000000000000000000, 0.000000000000000000 ) ) ;
#5720 = AXIS2_PLACEMENT_3D ( 'NONE', #10160, #25151, #40899 ) ;
#5721 = EDGE_LOOP ( 'NONE', ( #30256, #9334, #27245, #19437 ) ) ;
#5722 = CARTESIAN_POINT ( 'NONE',  ( 0.8182917201112819283, 0.000000000000000000, 0.4724409448818868706 ) ) ;
#5723 = CARTESIAN_POINT ( 'NONE',  ( -1.439733046521776583, 0.000000000000000000, -0.3149606299212592275 ) ) ;
#5724 = ORIENTED_EDGE ( 'NONE', *, *, #12990, .T. ) ;
#5725 = EDGE_LOOP ( 'NONE', ( #47606, #9789, #8859, #23830 ) ) ;
#5726 = VERTEX_POINT ( 'NONE', #18934 ) ;
#5727 = CARTESIAN_POINT ( 'NONE',  ( -0.07591351300297340121, 3.346456692913386100, -1.929133858267710000 ) ) ;
#5728 = ORIENTED_EDGE ( 'NONE', *, *, #36362, .T. ) ;
#5729 = ORIENTED_EDGE ( 'NONE', *, *, #21994, .F. ) ;
#5730 = DIRECTION ( 'NONE',  ( 1.000000000000000000, -0.000000000000000000, 0.000000000000000000 ) ) ;
#5731 = CARTESIAN_POINT ( 'NONE',  ( -1.166969139818015977, 3.346456692913386100, 2.047244094488179567 ) ) ;
#5732 = CARTESIAN_POINT ( 'NONE',  ( 0.8182917201112821504, 3.267716535433071279, -1.419509857074483539E-16 ) ) ;
#5733 = ORIENTED_EDGE ( 'NONE', *, *, #43765, .F. ) ;
#5734 = DIRECTION ( 'NONE',  ( 0.000000000000000000, 0.000000000000000000, 1.000000000000000000 ) ) ;
#5735 = CARTESIAN_POINT ( 'NONE',  ( 0.1155636338427008941, -0.5222242541845523167, 0.000000000000000000 ) ) ;
#5736 = AXIS2_PLACEMENT_3D ( 'NONE', #45136, #21418, #5916 ) ;
#5737 = FACE_OUTER_BOUND ( 'NONE', #38102, .T. ) ;
#5738 = ORIENTED_EDGE ( 'NONE', *, *, #17303, .T. ) ;
#5739 = DIRECTION ( 'NONE',  ( 0.000000000000000000, 0.000000000000000000, -1.000000000000000000 ) ) ;
#5740 = LINE ( 'NONE', #45715, #17804 ) ;
#5741 = EDGE_CURVE ( 'NONE', #3513, #50909, #35188, .T. ) ;
#5742 = EDGE_CURVE ( 'NONE', #29455, #13127, #29747, .T. ) ;
#5743 = DIRECTION ( 'NONE',  ( -3.469446951953613696E-16, 0.000000000000000000, -1.000000000000000000 ) ) ;
#5744 = EDGE_LOOP ( 'NONE', ( #9518, #12886, #4336, #50309 ) ) ;
#5745 = ORIENTED_EDGE ( 'NONE', *, *, #18280, .F. ) ;
#5746 = EDGE_CURVE ( 'NONE', #26109, #23437, #50866, .T. ) ;
#5747 = AXIS2_PLACEMENT_3D ( 'NONE', #44407, #24799, #1300 ) ;
#5748 = CARTESIAN_POINT ( 'NONE',  ( 1.181102362204724310, 0.000000000000000000, -1.062992125984252079 ) ) ;
#5749 = CARTESIAN_POINT ( 'NONE',  ( -1.648387110752326468, 1.040182331015016670, 1.961529008066261071 ) ) ;
#5750 = FACE_OUTER_BOUND ( 'NONE', #8062, .T. ) ;
#5751 = ORIENTED_EDGE ( 'NONE', *, *, #21446, .T. ) ;
#5752 = ORIENTED_EDGE ( 'NONE', *, *, #49279, .T. ) ;
#5753 = CARTESIAN_POINT ( 'NONE',  ( 1.662320194739497436, 6.692913385826772199, -1.388601395075552469 ) ) ;
#5754 = VECTOR ( 'NONE', #24384, 39.37007874015748143 ) ;
#5755 = VERTEX_POINT ( 'NONE', #30556 ) ;
#5756 = CARTESIAN_POINT ( 'NONE',  ( -0.2727639067037610499, 3.267716535433071279, -2.047244094488181343 ) ) ;
#5757 = CARTESIAN_POINT ( 'NONE',  ( -2.100190309385016274, 0.000000000000000000, 0.5298329251847215815 ) ) ;
#5758 = ADVANCED_FACE ( 'NONE', ( #26923 ), #4187, .T. ) ;
#5759 = FACE_OUTER_BOUND ( 'NONE', #15559, .T. ) ;
#5760 = B_SPLINE_CURVE_WITH_KNOTS ( 'NONE', 3,
 ( #33157, #9651, #3101, #46437 ),
 .UNSPECIFIED., .F., .F.,
 ( 4, 4 ),
 ( 3.500189189202590508E-07, 0.04605799665413929517 ),
 .UNSPECIFIED. ) ;
#5761 = CARTESIAN_POINT ( 'NONE',  ( -2.454875160333845674, 3.346456692913386100, -0.1574803149606298636 ) ) ;
#5762 = DIRECTION ( 'NONE',  ( -3.469446951953613696E-16, 0.000000000000000000, -1.000000000000000000 ) ) ;
#5763 = ORIENTED_EDGE ( 'NONE', *, *, #22322, .F. ) ;
#5764 = LINE ( 'NONE', #2403, #1107 ) ;
#5765 = FACE_OUTER_BOUND ( 'NONE', #15794, .T. ) ;
#5766 = ADVANCED_FACE ( 'NONE', ( #7318 ), #7566, .F. ) ;
#5767 = FACE_OUTER_BOUND ( 'NONE', #50441, .T. ) ;
#5768 = ORIENTED_EDGE ( 'NONE', *, *, #18494, .T. ) ;
#5769 = CARTESIAN_POINT ( 'NONE',  ( -0.5325339963216841888, 1.608673276636491511, 2.658891206781928584 ) ) ;
#5770 = DIRECTION ( 'NONE',  ( -1.000000000000000000, 0.000000000000000000, 1.734723475976806848E-16 ) ) ;
#5771 = DIRECTION ( 'NONE',  ( -0.000000000000000000, 1.000000000000000000, -0.000000000000000000 ) ) ;
#5772 = AXIS2_PLACEMENT_3D ( 'NONE', #19180, #30565, #3193 ) ;
#5773 = VERTEX_POINT ( 'NONE', #19419 ) ;
#5774 = LINE ( 'NONE', #49096, #26710 ) ;
#5775 = DIRECTION ( 'NONE',  ( 0.000000000000000000, 0.000000000000000000, -1.000000000000000000 ) ) ;
#5776 = ORIENTED_EDGE ( 'NONE', *, *, #46908, .F. ) ;
#5777 = CARTESIAN_POINT ( 'NONE',  ( 1.877225812761377011, 0.01875739138253415192, -0.8558842445003409516 ) ) ;
#5778 = CARTESIAN_POINT ( 'NONE',  ( 0.04921259842519670746, 1.514263714023589502, 2.952755905511811108 ) ) ;
#5779 = VERTEX_POINT ( 'NONE', #31315 ) ;
#5780 = DIRECTION ( 'NONE',  ( 1.000000000000000000, 0.000000000000000000, 0.000000000000000000 ) ) ;
#5781 = ADVANCED_FACE ( 'NONE', ( #47010 ), #15566, .F. ) ;
#5782 = VECTOR ( 'NONE', #26819, 39.37007874015748143 ) ;
#5783 = CARTESIAN_POINT ( 'NONE',  ( 0.5455278134075211005, 3.346456692913386100, -0.5118110236220467790 ) ) ;
#5784 = DIRECTION ( 'NONE',  ( -1.000000000000000000, 0.000000000000000000, -0.000000000000000000 ) ) ;
#5785 = DIRECTION ( 'NONE',  ( -0.000000000000000000, -1.000000000000000000, -0.000000000000000000 ) ) ;
#5786 = VECTOR ( 'NONE', #29746, 39.37007874015748143 ) ;
#5787 = CARTESIAN_POINT ( 'NONE',  ( -0.6235241006192316915, 5.905511811023623991, 2.074304693190350157 ) ) ;
#5788 = ORIENTED_EDGE ( 'NONE', *, *, #23109, .F. ) ;
#5789 = EDGE_LOOP ( 'NONE', ( #6881, #12510, #39083, #29734 ) ) ;
#5790 = CARTESIAN_POINT ( 'NONE',  ( 0.5455278134075211005, 3.267716535433071279, -0.5118110236220467790 ) ) ;
#5791 = DIRECTION ( 'NONE',  ( -1.000000000000000000, 0.000000000000000000, -0.000000000000000000 ) ) ;
#5792 = ORIENTED_EDGE ( 'NONE', *, *, #48412, .T. ) ;
#5793 = CARTESIAN_POINT ( 'NONE',  ( 0.000000000000000000, 3.346456692913386100, 0.000000000000000000 ) ) ;
#5794 = CARTESIAN_POINT ( 'NONE',  ( -1.712496953225537633, 3.346456692913386100, 1.226315847645293999 ) ) ;
#5795 = LINE ( 'NONE', #49375, #50791 ) ;
#5796 = ORIENTED_EDGE ( 'NONE', *, *, #11004, .F. ) ;
#5797 = ORIENTED_EDGE ( 'NONE', *, *, #4678, .F. ) ;
#5798 = DIRECTION ( 'NONE',  ( -0.04486483035050446017, 1.288287287306305283E-16, -0.9989930665413151445 ) ) ;
#5799 = CARTESIAN_POINT ( 'NONE',  ( 0.4696143004045484348, 3.267716535433071279, 1.535433070866133898 ) ) ;
#5800 = LINE ( 'NONE', #21548, #14841 ) ;
#5801 = ORIENTED_EDGE ( 'NONE', *, *, #45713, .T. ) ;
#5802 = LENGTH_MEASURE_WITH_UNIT ( LENGTH_MEASURE( 0.02539999999999999897 ), #14821 );
#5803 = FACE_BOUND ( 'NONE', #26604, .T. ) ;
#5804 = EDGE_LOOP ( 'NONE', ( #24791, #15698, #48121 ) ) ;
#5805 = ADVANCED_FACE ( 'NONE', ( #23554 ), #39309, .F. ) ;
#5806 = CARTESIAN_POINT ( 'NONE',  ( 0.8182917201112824834, 3.267716535433071279, 1.732283464566921172 ) ) ;
#5807 = ORIENTED_EDGE ( 'NONE', *, *, #21141, .T. ) ;
#5808 = ORIENTED_EDGE ( 'NONE', *, *, #37373, .F. ) ;
#5809 = CARTESIAN_POINT ( 'NONE',  ( 2.013783482383322720, 1.740156378764222245, 1.139548688847630942 ) ) ;
#5810 = DIRECTION ( 'NONE',  ( -3.986037398843765983E-20, -1.000000000000000000, -1.160734090543304660E-16 ) ) ;
#5811 = EDGE_CURVE ( 'NONE', #44964, #12754, #35442, .T. ) ;
#5812 = EDGE_CURVE ( 'NONE', #28481, #42469, #42249, .T. ) ;
#5813 = VERTEX_POINT ( 'NONE', #10931 ) ;
#5814 = DIRECTION ( 'NONE',  ( 1.734723475976806848E-16, 0.000000000000000000, 1.000000000000000000 ) ) ;
#5815 = EDGE_CURVE ( 'NONE', #22677, #17201, #38811, .T. ) ;
#5816 = LINE ( 'NONE', #41196, #22191 ) ;
#5817 = VERTEX_POINT ( 'NONE', #32602 ) ;
#5818 = LINE ( 'NONE', #9697, #31059 ) ;
#5819 = LINE ( 'NONE', #21572, #50595 ) ;
#5820 = VECTOR ( 'NONE', #49902, 39.37007874015748143 ) ;
#5821 = VECTOR ( 'NONE', #25519, 39.37007874015748143 ) ;
#5822 = EDGE_CURVE ( 'NONE', #47516, #15540, #35564, .T. ) ;
#5823 = DIRECTION ( 'NONE',  ( 0.000000000000000000, 0.000000000000000000, -1.000000000000000000 ) ) ;
#5824 = CARTESIAN_POINT ( 'NONE',  ( -1.651646936617113148, 1.205361022782829114E-17, 0.5883978091303396774 ) ) ;
#5825 = CARTESIAN_POINT ( 'NONE',  ( 0.000000000000000000, 3.346456692913386100, 0.000000000000000000 ) ) ;
#5826 = ORIENTED_EDGE ( 'NONE', *, *, #45810, .T. ) ;
#5827 = DIRECTION ( 'NONE',  ( -0.000000000000000000, 1.000000000000000000, -0.000000000000000000 ) ) ;
#5828 = EDGE_CURVE ( 'NONE', #13249, #13554, #16588, .T. ) ;
#5829 = VECTOR ( 'NONE', #43039, 39.37007874015748143 ) ;
#5830 = CARTESIAN_POINT ( 'NONE',  ( 0.4696143004045479352, 3.346456692913386100, -1.102362204724405714 ) ) ;
#5831 = VERTEX_POINT ( 'NONE', #12972 ) ;
#5832 = CARTESIAN_POINT ( 'NONE',  ( 1.560669927219590525, 0.000000000000000000, -0.6692913385826764205 ) ) ;
#5833 = LINE ( 'NONE', #45552, #19540 ) ;
#5834 = ORIENTED_EDGE ( 'NONE', *, *, #21122, .F. ) ;
#5835 = CARTESIAN_POINT ( 'NONE',  ( -0.6982598466389058345, 0.000000000000000000, 1.720449438420079691 ) ) ;
#5836 = EDGE_CURVE ( 'NONE', #41060, #29553, #31815, .T. ) ;
#5837 = LINE ( 'NONE', #37088, #1955 ) ;
#5838 = CARTESIAN_POINT ( 'NONE',  ( 0.04921259842519689481, 1.205361022782829114E-17, -2.165433070866142007 ) ) ;
#5839 = ORIENTED_EDGE ( 'NONE', *, *, #4031, .T. ) ;
#5840 = FACE_OUTER_BOUND ( 'NONE', #34649, .T. ) ;
#5841 = ORIENTED_EDGE ( 'NONE', *, *, #49708, .T. ) ;
#5842 = FACE_BOUND ( 'NONE', #11615, .T. ) ;
#5843 = EDGE_CURVE ( 'NONE', #18933, #11499, #35693, .T. ) ;
#5844 = CARTESIAN_POINT ( 'NONE',  ( 2.878724150143186833, 0.000000000000000000, -0.6570500018394808128 ) ) ;
#5845 = LINE ( 'NONE', #41726, #404 ) ;
#5846 = DIRECTION ( 'NONE',  ( 1.442222014787672788E-15, -0.7071067811865483499, -0.7071067811865465735 ) ) ;
#5847 = ORIENTED_EDGE ( 'NONE', *, *, #38387, .F. ) ;
#5848 = ORIENTED_EDGE ( 'NONE', *, *, #3869, .T. ) ;
#5849 = DIRECTION ( 'NONE',  ( -0.000000000000000000, 0.000000000000000000, 1.000000000000000000 ) ) ;
#5850 = VERTEX_POINT ( 'NONE', #5212 ) ;
#5851 = EDGE_CURVE ( 'NONE', #29348, #8682, #32342, .T. ) ;
#5852 = DIRECTION ( 'NONE',  ( -3.469446951953613696E-16, 0.000000000000000000, -1.000000000000000000 ) ) ;
#5853 = ORIENTED_EDGE ( 'NONE', *, *, #45204, .T. ) ;
#5854 = EDGE_CURVE ( 'NONE', #33436, #28782, #27936, .T. ) ;
#5855 = VECTOR ( 'NONE', #11843, 39.37007874015748143 ) ;
#5856 = CARTESIAN_POINT ( 'NONE',  ( 0.07982360342473591996, 1.709180471932028711, 0.000000000000000000 ) ) ;
#5857 = VECTOR ( 'NONE', #23691, 39.37007874015748143 ) ;
#5858 = ORIENTED_EDGE ( 'NONE', *, *, #30748, .F. ) ;
#5859 = DIRECTION ( 'NONE',  ( 1.000000000000000000, 0.000000000000000000, 0.000000000000000000 ) ) ;
#5860 = CARTESIAN_POINT ( 'NONE',  ( -1.363819533518803029, 3.346456692913386100, 0.4724409448818871482 ) ) ;
#5861 = ORIENTED_EDGE ( 'NONE', *, *, #3603, .T. ) ;
#5862 = PLANE ( 'NONE',  #13352 ) ;
#5863 = ORIENTED_EDGE ( 'NONE', *, *, #4225, .T. ) ;
#5864 = AXIS2_PLACEMENT_3D ( 'NONE', #45833, #6626, #37367 ) ;
#5865 = ORIENTED_EDGE ( 'NONE', *, *, #28004, .F. ) ;
#5866 = ADVANCED_FACE ( 'NONE', ( #48543 ), #28442, .F. ) ;
#5867 = AXIS2_PLACEMENT_3D ( 'NONE', #26215, #19215, #37853 ) ;
#5868 = ORIENTED_EDGE ( 'NONE', *, *, #33209, .F. ) ;
#5869 = ORIENTED_EDGE ( 'NONE', *, *, #19464, .F. ) ;
#5870 = DIRECTION ( 'NONE',  ( -1.000000000000000000, 0.000000000000000000, -0.000000000000000000 ) ) ;
#5871 = EDGE_CURVE ( 'NONE', #26807, #44408, #43676, .T. ) ;
#5872 = ORIENTED_EDGE ( 'NONE', *, *, #321, .T. ) ;
#5873 = CARTESIAN_POINT ( 'NONE',  ( 1.560669927219590303, 3.346456692913386100, -1.501022570047217508 ) ) ;
#5874 = LINE ( 'NONE', #25245, #2985 ) ;
#5875 = CARTESIAN_POINT ( 'NONE',  ( 0.000000000000000000, 6.692913385826772199, 0.000000000000000000 ) ) ;
#5876 = ORIENTED_EDGE ( 'NONE', *, *, #11732, .T. ) ;
#5877 = CARTESIAN_POINT ( 'NONE',  ( -1.295932337743544771, 1.600617638626312678, -2.653223682116380377 ) ) ;
#5878 = FACE_OUTER_BOUND ( 'NONE', #22395, .T. ) ;
#5879 = ORIENTED_EDGE ( 'NONE', *, *, #25978, .T. ) ;
#5880 = CARTESIAN_POINT ( 'NONE',  ( -0.6214413264104939882, 3.267716535433071279, 2.156057715732899300E-16 ) ) ;
#5881 = CARTESIAN_POINT ( 'NONE',  ( 0.000000000000000000, 1.574803149606302854, 0.000000000000000000 ) ) ;
#5882 = CARTESIAN_POINT ( 'NONE',  ( -1.051609096396380449, 0.4349011127721510994, -1.025452293874513643 ) ) ;
#5883 = DIRECTION ( 'NONE',  ( 0.000000000000000000, 0.000000000000000000, -1.000000000000000000 ) ) ;
#5884 = AXIS2_PLACEMENT_3D ( 'NONE', #34531, #27271, #10523 ) ;
#5885 = VECTOR ( 'NONE', #29805, 39.37007874015748143 ) ;
#5886 = PLANE ( 'NONE',  #22385 ) ;
#5887 = DIRECTION ( 'NONE',  ( -0.000000000000000000, 1.000000000000000000, -0.000000000000000000 ) ) ;
#5888 = ORIENTED_EDGE ( 'NONE', *, *, #21921, .F. ) ;
#5889 = FACE_OUTER_BOUND ( 'NONE', #25561, .T. ) ;
#5890 = EDGE_CURVE ( 'NONE', #21800, #640, #2281, .T. ) ;
#5891 = DIRECTION ( 'NONE',  ( 0.000000000000000000, -1.000000000000000000, 0.000000000000000000 ) ) ;
#5892 = VECTOR ( 'NONE', #25661, 39.37007874015748143 ) ;
#5893 = VERTEX_POINT ( 'NONE', #1083 ) ;
#5894 = LINE ( 'NONE', #45116, #1190 ) ;
#5895 = AXIS2_PLACEMENT_3D ( 'NONE', #6748, #21293, #46457 ) ;
#5896 = ORIENTED_EDGE ( 'NONE', *, *, #14795, .F. ) ;
#5897 = LINE ( 'NONE', #1262, #3889 ) ;
#5898 = EDGE_CURVE ( 'NONE', #49043, #48480, #47523, .T. ) ;
#5899 = CARTESIAN_POINT ( 'NONE',  ( -0.2727639067037602172, 0.000000000000000000, 0.7874015748031456541 ) ) ;
#5900 = PLANE ( 'NONE',  #4783 ) ;
#5901 = EDGE_CURVE ( 'NONE', #14542, #34665, #28702, .T. ) ;
#5902 = CARTESIAN_POINT ( 'NONE',  ( -1.091055626815042201, 3.267716535433071279, 0.7480314960629874665 ) ) ;
#5903 = CARTESIAN_POINT ( 'NONE',  ( 0.1968503937007873850, 3.346456692913386100, -0.1968503937007874405 ) ) ;
#5904 = VERTEX_POINT ( 'NONE', #39816 ) ;
#5905 = ADVANCED_FACE ( 'NONE', ( #44450 ), #318, .F. ) ;
#5906 = PLANE ( 'NONE',  #13346 ) ;
#5907 = VERTEX_POINT ( 'NONE', #40076 ) ;
#5908 = FACE_OUTER_BOUND ( 'NONE', #13539, .T. ) ;
#5909 = ORIENTED_EDGE ( 'NONE', *, *, #1016, .F. ) ;
#5910 = FACE_OUTER_BOUND ( 'NONE', #16784, .T. ) ;
#5911 = LINE ( 'NONE', #23806, #8735 ) ;
#5912 = ORIENTED_EDGE ( 'NONE', *, *, #8437, .T. ) ;
#5913 = DIRECTION ( 'NONE',  ( -0.9362348706397417564, -4.074795501490096117E-17, 0.3513748240813304724 ) ) ;
#5914 = CARTESIAN_POINT ( 'NONE',  ( 1.915720322920900331, 0.05860343245220329955, -0.3867724703730804348 ) ) ;
#5915 = EDGE_CURVE ( 'NONE', #37376, #45969, #20451, .T. ) ;
#5916 = DIRECTION ( 'NONE',  ( 1.734723475976806848E-16, 0.000000000000000000, 1.000000000000000000 ) ) ;
#5917 = ORIENTED_EDGE ( 'NONE', *, *, #4031, .F. ) ;
#5918 = VERTEX_POINT ( 'NONE', #39565 ) ;
#5919 = CARTESIAN_POINT ( 'NONE',  ( 1.909347346926324462, 3.346456692913386100, -0.7874015748031473194 ) ) ;
#5920 = FACE_BOUND ( 'NONE', #20077, .T. ) ;
#5921 = EDGE_LOOP ( 'NONE', ( #21543, #37183, #2903, #51009 ) ) ;
#5922 = EDGE_CURVE ( 'NONE', #13777, #29680, #9088, .T. ) ;
#5923 = CIRCLE ( 'NONE', #43862, 2.165354330708661568 ) ;
#5924 = CARTESIAN_POINT ( 'NONE',  ( 1.038530695135447157, 0.4349011127721510994, 1.038530695135446491 ) ) ;
#5925 = CARTESIAN_POINT ( 'NONE',  ( -1.195183497228115035E-16, 0.000000000000000000, 0.6299212598425161236 ) ) ;
#5926 = ORIENTED_EDGE ( 'NONE', *, *, #47886, .T. ) ;
#5927 = ORIENTED_EDGE ( 'NONE', *, *, #29010, .F. ) ;
#5928 = EDGE_CURVE ( 'NONE', #9867, #380, #34292, .T. ) ;
#5929 = ADVANCED_FACE ( 'NONE', ( #4195 ), #43931, .F. ) ;
#5930 = CARTESIAN_POINT ( 'NONE',  ( -0.7381027496704857249, 1.531192278308824539, -2.859439394060923068 ) ) ;
#5931 = AXIS2_PLACEMENT_3D ( 'NONE', #50611, #15057, #49865 ) ;
#5932 = DIRECTION ( 'NONE',  ( -0.000000000000000000, 1.000000000000000000, -0.000000000000000000 ) ) ;
#5933 = ORIENTED_EDGE ( 'NONE', *, *, #724, .T. ) ;
#5934 = VERTEX_POINT ( 'NONE', #49050 ) ;
#5935 = AXIS2_PLACEMENT_3D ( 'NONE', #5611, #21365, #48174 ) ;
#5936 = B_SPLINE_CURVE_WITH_KNOTS ( 'NONE', 3,
 ( #39698, #38500, #8459, #455 ),
 .UNSPECIFIED., .F., .F.,
 ( 4, 4 ),
 ( 2.767188889283819338E-07, 0.002500421436352599953 ),
 .UNSPECIFIED. ) ;
#5937 = EDGE_LOOP ( 'NONE', ( #37341, #37558, #43902, #25835 ) ) ;
#5938 = CARTESIAN_POINT ( 'NONE',  ( 0.6584127755596609344, 0.000000000000000000, 1.614277297217986851 ) ) ;
#5939 = VECTOR ( 'NONE', #39349, 39.37007874015748143 ) ;
#5940 = CARTESIAN_POINT ( 'NONE',  ( 0.002207914879453961969, 6.692913385826772199, 0.04916304461325451958 ) ) ;
#5941 = DIRECTION ( 'NONE',  ( -3.469446951953613696E-16, 0.000000000000000000, -1.000000000000000000 ) ) ;
#5942 = PLANE ( 'NONE',  #42045 ) ;
#5943 = EDGE_LOOP ( 'NONE', ( #27980, #17491, #3263, #43050 ) ) ;
#5944 = ORIENTED_EDGE ( 'NONE', *, *, #17774, .T. ) ;
#5945 = CARTESIAN_POINT ( 'NONE',  ( -1.091055626815042645, 0.000000000000000000, -1.259842519685034690 ) ) ;
#5946 = CARTESIAN_POINT ( 'NONE',  ( 1.738775347548010775, 0.01809092828461609376, -1.088788177563327242 ) ) ;
#5947 = FACE_OUTER_BOUND ( 'NONE', #26998, .T. ) ;
#5948 = CARTESIAN_POINT ( 'NONE',  ( -0.6214413264104939882, 3.267716535433071279, 2.156057715732899300E-16 ) ) ;
#5949 = CARTESIAN_POINT ( 'NONE',  ( 0.8182917201112819283, 0.000000000000000000, 0.9055118110236164419 ) ) ;
#5950 = DIRECTION ( 'NONE',  ( -1.000000000000000000, -0.000000000000000000, -0.000000000000000000 ) ) ;
#5951 = FACE_OUTER_BOUND ( 'NONE', #7357, .T. ) ;
#5952 = VERTEX_POINT ( 'NONE', #17857 ) ;
#5953 = FACE_OUTER_BOUND ( 'NONE', #42865, .T. ) ;
#5954 = CARTESIAN_POINT ( 'NONE',  ( -0.5455278134075208785, 3.346456692913386100, 1.259842519685033357 ) ) ;
#5955 = ORIENTED_EDGE ( 'NONE', *, *, #6740, .T. ) ;
#5956 = VERTEX_POINT ( 'NONE', #25597 ) ;
#5957 = VECTOR ( 'NONE', #11076, 39.37007874015748143 ) ;
#5958 = DIRECTION ( 'NONE',  ( -3.469446951953613696E-16, 0.000000000000000000, -1.000000000000000000 ) ) ;
#5959 = EDGE_CURVE ( 'NONE', #39288, #19595, #9345, .T. ) ;
#5960 = ORIENTED_EDGE ( 'NONE', *, *, #8419, .F. ) ;
#5961 = EDGE_CURVE ( 'NONE', #48339, #18734, #41353, .T. ) ;
#5962 = AXIS2_PLACEMENT_3D ( 'NONE', #15128, #14878, #23630 ) ;
#5963 = ORIENTED_EDGE ( 'NONE', *, *, #5741, .F. ) ;
#5964 = LINE ( 'NONE', #24824, #22119 ) ;
#5965 = AXIS2_PLACEMENT_3D ( 'NONE', #32946, #8406, #9428 ) ;
#5966 = EDGE_LOOP ( 'NONE', ( #35133, #49690, #35452, #22345 ) ) ;
#5967 = EDGE_CURVE ( 'NONE', #26524, #8104, #5977, .T. ) ;
#5968 = VECTOR ( 'NONE', #47121, 39.37007874015748143 ) ;
#5969 = CARTESIAN_POINT ( 'NONE',  ( 1.536664496436137830E-16, 3.267716535433071279, -2.665687976667846366E-32 ) ) ;
#5970 = CARTESIAN_POINT ( 'NONE',  ( 0.1071992566810385378, 0.000000000000000000, -1.740088185897661788 ) ) ;
#5971 = B_SPLINE_CURVE_WITH_KNOTS ( 'NONE', 3,
 ( #14393, #1751, #17506, #41011 ),
 .UNSPECIFIED., .F., .F.,
 ( 4, 4 ),
 ( 0.001391672322771502933, 0.04655779653607895058 ),
 .UNSPECIFIED. ) ;
#5972 = VERTEX_POINT ( 'NONE', #2367 ) ;
#5973 = ORIENTED_EDGE ( 'NONE', *, *, #34789, .F. ) ;
#5974 = CARTESIAN_POINT ( 'NONE',  ( -1.812426027168695164, 1.687013308263498601, 1.999690358701252224 ) ) ;
#5975 = ORIENTED_EDGE ( 'NONE', *, *, #17589, .F. ) ;
#5976 = EDGE_LOOP ( 'NONE', ( #28466, #48268, #15483, #21224 ) ) ;
#5977 = LINE ( 'NONE', #26110, #35554 ) ;
#5978 = FACE_OUTER_BOUND ( 'NONE', #45627, .T. ) ;
#5979 = DIRECTION ( 'NONE',  ( -0.000000000000000000, 0.000000000000000000, 1.000000000000000000 ) ) ;
#5980 = EDGE_CURVE ( 'NONE', #26348, #26976, #44950, .T. ) ;
#5981 = ORIENTED_EDGE ( 'NONE', *, *, #38170, .F. ) ;
#5982 = EDGE_CURVE ( 'NONE', #39976, #17373, #2109, .T. ) ;
#5983 = CARTESIAN_POINT ( 'NONE',  ( -0.3486774197067339376, 3.267716535433071279, -0.3149606299212593941 ) ) ;
#5984 = FACE_OUTER_BOUND ( 'NONE', #45319, .T. ) ;
#5985 = CARTESIAN_POINT ( 'NONE',  ( 0.3136974817028399531, 5.905511811023623991, -2.936457595020219635 ) ) ;
#5986 = ORIENTED_EDGE ( 'NONE', *, *, #28757, .F. ) ;
#5987 = EDGE_CURVE ( 'NONE', #36398, #38696, #33620, .T. ) ;
#5988 = DIRECTION ( 'NONE',  ( -0.9510565162951500895, 0.000000000000000000, -0.3090169943749582204 ) ) ;
#5989 = PLANE ( 'NONE',  #1325 ) ;
#5990 = EDGE_CURVE ( 'NONE', #22920, #47415, #18279, .T. ) ;
#5991 = CARTESIAN_POINT ( 'NONE',  ( -0.8069532150559463046, 5.905511811023623991, -2.010061882867142380 ) ) ;
#5992 = ORIENTED_EDGE ( 'NONE', *, *, #17751, .F. ) ;
#5993 = ORIENTED_EDGE ( 'NONE', *, *, #9951, .F. ) ;
#5994 = EDGE_CURVE ( 'NONE', #30196, #31565, #21989, .T. ) ;
#5996 = VECTOR ( 'NONE', #723, 39.37007874015748143 ) ;
#5995 = LINE ( 'NONE', #33387, #28880 ) ;
#5997 = LINE ( 'NONE', #12991, #22009 ) ;
#5998 = CARTESIAN_POINT ( 'NONE',  ( -2.715141060683412100, 5.905511811023623991, -1.160506983230101596 ) ) ;
#5999 = EDGE_LOOP ( 'NONE', ( #41647, #41341, #49136, #46808 ) ) ;
#6000 = ORIENTED_EDGE ( 'NONE', *, *, #30748, .T. ) ;
#6001 = VECTOR ( 'NONE', #40083, 39.37007874015748143 ) ;
#6002 = CARTESIAN_POINT ( 'NONE',  ( -0.7681069143398193688, 1.604975391610140578, -2.598188753026931419 ) ) ;
#6003 = VECTOR ( 'NONE', #31844, 39.37007874015748143 ) ;
#6004 = ORIENTED_EDGE ( 'NONE', *, *, #28121, .F. ) ;
#6005 = CARTESIAN_POINT ( 'NONE',  ( 2.277873973731426194, 5.905511811023623991, 1.879489153247668742 ) ) ;
#6006 = DIRECTION ( 'NONE',  ( 0.6579387259397027066, 0.000000000000000000, 0.7530714660036195163 ) ) ;
#6007 = AXIS2_PLACEMENT_3D ( 'NONE', #29638, #29379, #33778 ) ;
#6008 = VECTOR ( 'NONE', #40894, 39.37007874015748143 ) ;
#6009 = CARTESIAN_POINT ( 'NONE',  ( 0.000000000000000000, 3.267716535433071279, -1.929133858267710000 ) ) ;
#6010 = DIRECTION ( 'NONE',  ( -0.000000000000000000, 1.000000000000000000, -0.000000000000000000 ) ) ;
#6011 = CARTESIAN_POINT ( 'NONE',  ( 1.909347346926324684, 3.346456692913386100, 1.021348170950612033 ) ) ;
#6012 = VECTOR ( 'NONE', #5827, 39.37007874015748143 ) ;
#6013 = EDGE_LOOP ( 'NONE', ( #41931, #34504, #31022, #6925 ) ) ;
#6014 = DIRECTION ( 'NONE',  ( 0.000000000000000000, 1.000000000000000000, 0.000000000000000000 ) ) ;
#6015 = LINE ( 'NONE', #21770, #12002 ) ;
#6016 = CARTESIAN_POINT ( 'NONE',  ( 0.8227799331039057362, -2.325738524975369762E-16, 2.052232022298799752 ) ) ;
#6017 = VERTEX_POINT ( 'NONE', #1854 ) ;
#6018 = CARTESIAN_POINT ( 'NONE',  ( -0.4462886659516242527, 1.602328624241157851, 2.183640264916793861 ) ) ;
#6019 = LINE ( 'NONE', #44737, #34384 ) ;
#6020 = CARTESIAN_POINT ( 'NONE',  ( 0.000000000000000000, 0.000000000000000000, 0.000000000000000000 ) ) ;
#6021 = VERTEX_POINT ( 'NONE', #49807 ) ;
#6022 = DIRECTION ( 'NONE',  ( 1.000000000000000000, -0.000000000000000000, 0.000000000000000000 ) ) ;
#6023 = ADVANCED_FACE ( 'NONE', ( #17351 ), #6498, .F. ) ;
#6024 = EDGE_CURVE ( 'NONE', #50505, #19595, #24831, .T. ) ;
#6025 = ORIENTED_EDGE ( 'NONE', *, *, #49042, .T. ) ;
#6026 = CARTESIAN_POINT ( 'NONE',  ( 3.937007874015748143, 2.755905511811027164, -1.181102362204724088 ) ) ;
#6027 = DIRECTION ( 'NONE',  ( -0.000000000000000000, 1.000000000000000000, -0.000000000000000000 ) ) ;
#6028 = EDGE_LOOP ( 'NONE', ( #14691, #38744, #24735, #6724 ) ) ;
#6029 = FACE_OUTER_BOUND ( 'NONE', #38587, .T. ) ;
#6030 = EDGE_CURVE ( 'NONE', #24792, #13472, #2921, .T. ) ;
#6031 = DIRECTION ( 'NONE',  ( 1.000000000000000000, 0.000000000000000000, -3.469446951953613696E-16 ) ) ;
#6032 = DIRECTION ( 'NONE',  ( 1.000000000000000000, 0.000000000000000000, -3.469446951953613696E-16 ) ) ;
#6033 = CARTESIAN_POINT ( 'NONE',  ( -1.171400696859933532, 1.590714628027123823, 1.864644694871980590 ) ) ;
#6034 = LINE ( 'NONE', #25401, #50144 ) ;
#6035 = AXIS2_PLACEMENT_3D ( 'NONE', #20530, #16145, #36029 ) ;
#6036 = ORIENTED_EDGE ( 'NONE', *, *, #10565, .F. ) ;
#6037 = ORIENTED_EDGE ( 'NONE', *, *, #24860, .F. ) ;
#6038 = LINE ( 'NONE', #41666, #20739 ) ;
#6039 = FACE_OUTER_BOUND ( 'NONE', #26490, .T. ) ;
#6040 = EDGE_LOOP ( 'NONE', ( #21498, #11570, #39933, #5298 ) ) ;
#6041 = VECTOR ( 'NONE', #34480, 39.37007874015748143 ) ;
#6042 = CARTESIAN_POINT ( 'NONE',  ( 2.139229417893225182, 5.905511811023623991, -0.3394403656973405403 ) ) ;
#6043 = FACE_OUTER_BOUND ( 'NONE', #36783, .T. ) ;
#6044 = CARTESIAN_POINT ( 'NONE',  ( 2.298329729270955024, 1.656597557696453116, 1.853838447124175337 ) ) ;
#6045 = VECTOR ( 'NONE', #33890, 39.37007874015748143 ) ;
#6046 = VECTOR ( 'NONE', #2334, 39.37007874015748143 ) ;
#6047 = EDGE_LOOP ( 'NONE', ( #45707, #36004, #37839, #38313 ) ) ;
#6048 = ORIENTED_EDGE ( 'NONE', *, *, #17080, .F. ) ;
#6049 = ADVANCED_FACE ( 'NONE', ( #49554 ), #29983, .F. ) ;
#6050 = FACE_OUTER_BOUND ( 'NONE', #9018, .T. ) ;
#6051 = CARTESIAN_POINT ( 'NONE',  ( 0.5455278134075211005, 0.000000000000000000, -0.1968503937007880511 ) ) ;
#6052 = CARTESIAN_POINT ( 'NONE',  ( -0.04921259842519708216, 1.620047916482694861, 2.952755905511811108 ) ) ;
#6053 = EDGE_LOOP ( 'NONE', ( #15231, #37592, #23070, #1158 ) ) ;
#6054 = LINE ( 'NONE', #41428, #46293 ) ;
#6055 = DIRECTION ( 'NONE',  ( -0.000000000000000000, 1.000000000000000000, -0.000000000000000000 ) ) ;
#6056 = VECTOR ( 'NONE', #31100, 39.37007874015748143 ) ;
#6057 = ORIENTED_EDGE ( 'NONE', *, *, #10565, .T. ) ;
#6058 = EDGE_CURVE ( 'NONE', #12607, #46834, #1600, .T. ) ;
#6059 = LINE ( 'NONE', #45275, #31502 ) ;
#6060 = ORIENTED_EDGE ( 'NONE', *, *, #18524, .F. ) ;
#6061 = ORIENTED_EDGE ( 'NONE', *, *, #36534, .F. ) ;
#6062 = PLANE ( 'NONE',  #45184 ) ;
#6063 = LINE ( 'NONE', #40932, #16802 ) ;
#6064 = VERTEX_POINT ( 'NONE', #33114 ) ;
#6065 = DIRECTION ( 'NONE',  ( 0.000000000000000000, 0.000000000000000000, -1.000000000000000000 ) ) ;
#6066 = CARTESIAN_POINT ( 'NONE',  ( 1.909347346926324462, 3.267716535433071279, -3.312189666507127188E-16 ) ) ;
#6067 = ORIENTED_EDGE ( 'NONE', *, *, #9777, .T. ) ;
#6068 = EDGE_CURVE ( 'NONE', #24438, #37496, #48795, .T. ) ;
#6069 = DIRECTION ( 'NONE',  ( -3.469446951953613696E-16, 0.000000000000000000, -1.000000000000000000 ) ) ;
#6070 = DIRECTION ( 'NONE',  ( 0.01601477604151182663, -0.9998717552508123996, 0.000000000000000000 ) ) ;
#6071 = DIRECTION ( 'NONE',  ( 0.3090169943749582204, 0.000000000000000000, -0.9510565162951500895 ) ) ;
#6072 = VECTOR ( 'NONE', #1606, 39.37007874015748143 ) ;
#6073 = LINE ( 'NONE', #49653, #43456 ) ;
#6074 = CARTESIAN_POINT ( 'NONE',  ( -2.082617625631827174, 3.346456692913386100, -0.3149606299212589500 ) ) ;
#6075 = VERTEX_POINT ( 'NONE', #25095 ) ;
#6076 = FACE_OUTER_BOUND ( 'NONE', #42864, .T. ) ;
#6077 = AXIS2_PLACEMENT_3D ( 'NONE', #23471, #11603, #4369 ) ;
#6078 = B_SPLINE_CURVE_WITH_KNOTS ( 'NONE', 3,
 ( #38563, #43167, #3186, #50618 ),
 .UNSPECIFIED., .F., .F.,
 ( 4, 4 ),
 ( 5.483124400437757281E-06, 0.05042175502089817074 ),
 .UNSPECIFIED. ) ;
#6079 = LINE ( 'NONE', #33473, #37222 ) ;
#6080 = VECTOR ( 'NONE', #32152, 39.37007874015748143 ) ;
#6081 = VECTOR ( 'NONE', #16296, 39.37007874015748143 ) ;
#6082 = ORIENTED_EDGE ( 'NONE', *, *, #1111, .F. ) ;
#6083 = DIRECTION ( 'NONE',  ( -3.469446951953613696E-16, 0.000000000000000000, -1.000000000000000000 ) ) ;
#6084 = LINE ( 'NONE', #13331, #25304 ) ;
#6085 = ORIENTED_EDGE ( 'NONE', *, *, #26950, .F. ) ;
#6086 = DIRECTION ( 'NONE',  ( 1.000000000000000000, 0.000000000000000000, 0.000000000000000000 ) ) ;
#6087 = CARTESIAN_POINT ( 'NONE',  ( -0.2727639067037602727, 0.000000000000000000, 1.220472440944875281 ) ) ;
#6088 = LINE ( 'NONE', #44554, #29329 ) ;
#6089 = AXIS2_PLACEMENT_3D ( 'NONE', #35665, #35415, #32 ) ;
#6090 = B_SPLINE_CURVE_WITH_KNOTS ( 'NONE', 3,
 ( #31933, #38899, #23398, #43775 ),
 .UNSPECIFIED., .F., .F.,
 ( 4, 4 ),
 ( 2.472340781885933090E-07, 0.002500445822774367312 ),
 .UNSPECIFIED. ) ;
#6091 = EDGE_CURVE ( 'NONE', #37886, #50549, #40846, .T. ) ;
#6092 = ORIENTED_EDGE ( 'NONE', *, *, #34640, .T. ) ;
#6093 = PLANE ( 'NONE',  #46904 ) ;
#6094 = ORIENTED_EDGE ( 'NONE', *, *, #21292, .F. ) ;
#6095 = FACE_BOUND ( 'NONE', #14236, .T. ) ;
#6096 = EDGE_CURVE ( 'NONE', #2778, #1395, #36979, .T. ) ;
#6097 = PLANE ( 'NONE',  #44024 ) ;
#6098 = PLANE ( 'NONE',  #1251 ) ;
#6100 = EDGE_CURVE ( 'NONE', #39431, #16156, #12334, .T. ) ;
#6099 = CARTESIAN_POINT ( 'NONE',  ( -0.5455278134075214336, 3.267716535433071279, -1.771653543307081025 ) ) ;
#6101 = EDGE_CURVE ( 'NONE', #8816, #34870, #10825, .T. ) ;
#6102 = EDGE_LOOP ( 'NONE', ( #42682, #48907, #11238, #44775 ) ) ;
#6103 = VERTEX_POINT ( 'NONE', #6997 ) ;
#6104 = CARTESIAN_POINT ( 'NONE',  ( -0.3486774197067340486, 0.000000000000000000, -0.5118110236220467790 ) ) ;
#6105 = ORIENTED_EDGE ( 'NONE', *, *, #24701, .T. ) ;
#6106 = PLANE ( 'NONE',  #27705 ) ;
#6107 = ORIENTED_EDGE ( 'NONE', *, *, #521, .F. ) ;
#6108 = PLANE ( 'NONE',  #12450 ) ;
#6109 = EDGE_CURVE ( 'NONE', #4531, #7644, #35574, .T. ) ;
#6110 = VERTEX_POINT ( 'NONE', #20327 ) ;
#6111 = CARTESIAN_POINT ( 'NONE',  ( -2.919426793319806368, 1.673754417692067564, 0.4451252810446391095 ) ) ;
#6112 = B_SPLINE_CURVE_WITH_KNOTS ( 'NONE', 3,
 ( #44208, #12725, #32101, #44462 ),
 .UNSPECIFIED., .F., .F.,
 ( 4, 4 ),
 ( 2.051433888766743662E-07, 0.01998722169972024648 ),
 .UNSPECIFIED. ) ;
#6113 = VECTOR ( 'NONE', #41053, 39.37007874015748143 ) ;
#6114 = DIRECTION ( 'NONE',  ( -0.000000000000000000, 1.000000000000000000, -0.000000000000000000 ) ) ;
#6115 = AXIS2_PLACEMENT_3D ( 'NONE', #44654, #5430, #28401 ) ;
#6116 = EDGE_LOOP ( 'NONE', ( #34655, #4965, #40977, #24570 ) ) ;
#6118 = EDGE_CURVE ( 'NONE', #43312, #1319, #11813, .T. ) ;
#6117 = PRODUCT_DEFINITION_CONTEXT ( 'detailed design', #26605, 'design' ) ;
#6119 = DIRECTION ( 'NONE',  ( -1.000000000000000000, -1.160734090543304660E-16, 0.000000000000000000 ) ) ;
#6120 = CONICAL_SURFACE ( 'NONE', #12709, 3.033577403570480779, 1.554780866114618743 ) ;
#6121 = ORIENTED_EDGE ( 'NONE', *, *, #32920, .F. ) ;
#6122 = ORIENTED_EDGE ( 'NONE', *, *, #50686, .F. ) ;
#6123 = CIRCLE ( 'NONE', #36640, 1.743387098533651480 ) ;
#6124 = VECTOR ( 'NONE', #41331, 39.37007874015748143 ) ;
#6125 = EDGE_CURVE ( 'NONE', #29367, #18870, #30588, .T. ) ;
#6126 = ORIENTED_EDGE ( 'NONE', *, *, #29788, .T. ) ;
#6127 = ORIENTED_EDGE ( 'NONE', *, *, #45646, .T. ) ;
#6128 = CARTESIAN_POINT ( 'NONE',  ( 0.5550072188453405442, 1.618366210323673338, -2.196007637835879045 ) ) ;
#6129 = VECTOR ( 'NONE', #11599, 39.37007874015748143 ) ;
#6130 = ORIENTED_EDGE ( 'NONE', *, *, #32991, .F. ) ;
#6131 = CARTESIAN_POINT ( 'NONE',  ( 0.000000000000000000, 3.267716535433071279, 1.889763779527550369 ) ) ;
#6132 = EDGE_CURVE ( 'NONE', #46532, #33705, #26332, .T. ) ;
#6133 = DIRECTION ( 'NONE',  ( 1.734723475976806848E-16, -0.000000000000000000, 1.000000000000000000 ) ) ;
#6134 = CARTESIAN_POINT ( 'NONE',  ( -0.8942052331142547050, 3.346456692913386100, 0.9448818897637749625 ) ) ;
#6135 = ORIENTED_EDGE ( 'NONE', *, *, #44796, .F. ) ;
#6136 = CARTESIAN_POINT ( 'NONE',  ( 0.000000000000000000, 3.267716535433071279, 0.000000000000000000 ) ) ;
#6137 = CARTESIAN_POINT ( 'NONE',  ( 0.3381173457103291979, 1.574803149606302854, 2.138793126519850762 ) ) ;
#6138 = EDGE_LOOP ( 'NONE', ( #17800, #34391, #42656, #77 ) ) ;
#6139 = LINE ( 'NONE', #45102, #8478 ) ;
#6140 = CARTESIAN_POINT ( 'NONE',  ( -2.926032761125793247, 5.905511811023623991, 0.3963580683592101139 ) ) ;
#6141 = ADVANCED_FACE ( 'NONE', ( #35322 ), #47656, .F. ) ;
#6142 = DIRECTION ( 'NONE',  ( 0.000000000000000000, -1.000000000000000000, 0.000000000000000000 ) ) ;
#6143 = DIRECTION ( 'NONE',  ( -3.469446951953613696E-16, 0.000000000000000000, -1.000000000000000000 ) ) ;
#6144 = ORIENTED_EDGE ( 'NONE', *, *, #38281, .T. ) ;
#6145 = CARTESIAN_POINT ( 'NONE',  ( 0.8615171519027529090, 0.5249316497054297148, -1.675535331380912263 ) ) ;
#6146 = LINE ( 'NONE', #41770, #1387 ) ;
#6147 = VERTEX_POINT ( 'NONE', #18624 ) ;
#6148 = PLANE ( 'NONE',  #43551 ) ;
#6149 = PLANE ( 'NONE',  #31697 ) ;
#6150 = VECTOR ( 'NONE', #5230, 39.37007874015748143 ) ;
#6151 = ORIENTED_EDGE ( 'NONE', *, *, #5039, .T. ) ;
#6152 = CARTESIAN_POINT ( 'NONE',  ( -1.731485473375985240, 1.585829450765412707, -1.723556154981469524 ) ) ;
#6153 = VECTOR ( 'NONE', #39848, 39.37007874015748143 ) ;
#6154 = VECTOR ( 'NONE', #34647, 39.37007874015748143 ) ;
#6155 = ORIENTED_EDGE ( 'NONE', *, *, #22723, .F. ) ;
#6156 = CARTESIAN_POINT ( 'NONE',  ( 1.287906020515829919, 3.346456692913386100, -1.771653543307081691 ) ) ;
#6157 = VECTOR ( 'NONE', #176, 39.37007874015748143 ) ;
#6158 = EDGE_CURVE ( 'NONE', #9586, #39809, #3118, .T. ) ;
#6160 = AXIS2_PLACEMENT_3D ( 'NONE', #22159, #38412, #29901 ) ;
#6159 = CARTESIAN_POINT ( 'NONE',  ( -0.5284761224300580373, 1.574803149606302854, -2.099874368989736784 ) ) ;
#6161 = CARTESIAN_POINT ( 'NONE',  ( -1.344308260564831103, 1.595933994539297185, 2.345942870151215498 ) ) ;
#6162 = CARTESIAN_POINT ( 'NONE',  ( -1.472219874544909768, 1.696317054561777171, 2.560030851058948898 ) ) ;
#6163 = CARTESIAN_POINT ( 'NONE',  ( 2.106197740627111514, 3.201134874551266218, -1.299212598425194320 ) ) ;
#6164 = ORIENTED_EDGE ( 'NONE', *, *, #28622, .T. ) ;
#6165 = EDGE_CURVE ( 'NONE', #40104, #29343, #3355, .T. ) ;
#6166 = DIRECTION ( 'NONE',  ( -3.986037398843765983E-20, -1.000000000000000000, -1.160734090543304660E-16 ) ) ;
#6167 = VECTOR ( 'NONE', #20655, 39.37007874015748143 ) ;
#6168 = EDGE_LOOP ( 'NONE', ( #49039, #12519, #19039, #29374 ) ) ;
#6169 = ORIENTED_EDGE ( 'NONE', *, *, #36702, .F. ) ;
#6170 = CARTESIAN_POINT ( 'NONE',  ( -1.712496953225537633, 3.346456692913386100, -0.4724409448818884805 ) ) ;
#6171 = ORIENTED_EDGE ( 'NONE', *, *, #30468, .F. ) ;
#6172 = DIRECTION ( 'NONE',  ( -0.000000000000000000, 1.000000000000000000, -0.000000000000000000 ) ) ;
#6173 = FACE_OUTER_BOUND ( 'NONE', #43064, .T. ) ;
#6174 = EDGE_LOOP ( 'NONE', ( #38247, #10916, #9031, #28698 ) ) ;
#6175 = DIRECTION ( 'NONE',  ( -1.000000000000000000, 0.000000000000000000, 0.000000000000000000 ) ) ;
#6176 = PLANE ( 'NONE',  #19952 ) ;
#6177 = CARTESIAN_POINT ( 'NONE',  ( -2.258024766633058622, 3.346456692913386100, 0.1574803149606286423 ) ) ;
#6178 = ORIENTED_EDGE ( 'NONE', *, *, #48714, .T. ) ;
#6179 = ORIENTED_EDGE ( 'NONE', *, *, #42519, .T. ) ;
#6180 = DIRECTION ( 'NONE',  ( 0.9909497617679352555, 0.000000000000000000, -0.1342332658176522420 ) ) ;
#6181 = FACE_BOUND ( 'NONE', #21381, .T. ) ;
#6182 = ORIENTED_EDGE ( 'NONE', *, *, #28798, .F. ) ;
#6183 = CARTESIAN_POINT ( 'NONE',  ( 0.000000000000000000, 3.267716535433071279, 0.7480314960629874665 ) ) ;
#6184 = DIRECTION ( 'NONE',  ( 0.000000000000000000, 0.000000000000000000, -1.000000000000000000 ) ) ;
#6185 = EDGE_CURVE ( 'NONE', #42163, #9179, #5936, .T. ) ;
#6186 = ORIENTED_EDGE ( 'NONE', *, *, #6497, .T. ) ;
#6187 = EDGE_LOOP ( 'NONE', ( #18313, #4578, #5933, #16681 ) ) ;
#6188 = CARTESIAN_POINT ( 'NONE',  ( -2.454875160333845674, 3.346456692913386100, 0.1574803149606286423 ) ) ;
#6189 = ORIENTED_EDGE ( 'NONE', *, *, #36575, .F. ) ;
#6190 = VECTOR ( 'NONE', #6529, 39.37007874015748143 ) ;
#6191 = DIRECTION ( 'NONE',  ( 0.000000000000000000, -1.000000000000000000, 0.000000000000000000 ) ) ;
#6192 = EDGE_LOOP ( 'NONE', ( #32167, #40299, #13222, #4182 ) ) ;
#6193 = VECTOR ( 'NONE', #24750, 39.37007874015748143 ) ;
#6194 = ORIENTED_EDGE ( 'NONE', *, *, #16760, .F. ) ;
#6195 = EDGE_CURVE ( 'NONE', #31499, #36192, #10235, .T. ) ;
#6196 = CONICAL_SURFACE ( 'NONE', #49005, 1.850107469027523210, 0.6386652850508578450 ) ;
#6197 = EDGE_LOOP ( 'NONE', ( #25392, #40367, #38788, #18172 ) ) ;
#6198 = DIRECTION ( 'NONE',  ( 0.000000000000000000, 0.000000000000000000, -1.000000000000000000 ) ) ;
#6199 = LINE ( 'NONE', #45409, #7660 ) ;
#6200 = ADVANCED_FACE ( 'NONE', ( #16207 ), #20059, .F. ) ;
#6201 = EDGE_CURVE ( 'NONE', #50682, #20750, #31963, .T. ) ;
#6202 = CARTESIAN_POINT ( 'NONE',  ( 0.2727639067037602172, 0.000000000000000000, -2.244094488188969727 ) ) ;
#6203 = LINE ( 'NONE', #26073, #37897 ) ;
#6204 = ORIENTED_EDGE ( 'NONE', *, *, #18202, .F. ) ;
#6205 = ORIENTED_EDGE ( 'NONE', *, *, #23127, .T. ) ;
#6206 = VECTOR ( 'NONE', #6555, 39.37007874015748143 ) ;
#6207 = DIRECTION ( 'NONE',  ( -0.000000000000000000, 1.000000000000000000, -0.000000000000000000 ) ) ;
#6208 = CARTESIAN_POINT ( 'NONE',  ( -1.556712866041156440, 0.000000000000000000, 2.509548638715847435 ) ) ;
#6209 = CARTESIAN_POINT ( 'NONE',  ( 2.009930929872536520, 5.905511811023623991, -0.8055662819783819817 ) ) ;
#6210 = EDGE_CURVE ( 'NONE', #45968, #50288, #2829, .T. ) ;
#6211 = LINE ( 'NONE', #42824, #16049 ) ;
#6212 = EDGE_CURVE ( 'NONE', #23878, #38339, #50065, .T. ) ;
#6213 = CARTESIAN_POINT ( 'NONE',  ( -0.1158910538491989134, 0.02606345816900213982, -1.836661962001401305 ) ) ;
#6214 = DIRECTION ( 'NONE',  ( -0.6910626489868580968, 1.288287287306305530E-16, -0.7227948638273978821 ) ) ;
#6215 = CARTESIAN_POINT ( 'NONE',  ( 0.1968503937007873017, 3.346456692913386100, -1.259842519685035134 ) ) ;
#6216 = ORIENTED_EDGE ( 'NONE', *, *, #49010, .T. ) ;
#6217 = DIRECTION ( 'NONE',  ( -3.469446951953613696E-16, 0.000000000000000000, -1.000000000000000000 ) ) ;
#6218 = CARTESIAN_POINT ( 'NONE',  ( 1.091055626815043311, 3.346456692913386100, 1.870389530743258755 ) ) ;
#6219 = ORIENTED_EDGE ( 'NONE', *, *, #5828, .F. ) ;
#6221 = EDGE_CURVE ( 'NONE', #33190, #13314, #39444, .T. ) ;
#6220 = ORIENTED_EDGE ( 'NONE', *, *, #7603, .T. ) ;
#6222 = DIRECTION ( 'NONE',  ( 1.000000000000000000, -0.000000000000000000, 0.000000000000000000 ) ) ;
#6223 = ORIENTED_EDGE ( 'NONE', *, *, #17480, .T. ) ;
#6224 = EDGE_CURVE ( 'NONE', #4877, #29154, #50999, .T. ) ;
#6225 = VECTOR ( 'NONE', #41144, 39.37007874015748143 ) ;
#6226 = AXIS2_PLACEMENT_3D ( 'NONE', #1283, #1025, #41048 ) ;
#6227 = VERTEX_POINT ( 'NONE', #48924 ) ;
#6228 = LINE ( 'NONE', #41593, #8921 ) ;
#6229 = VECTOR ( 'NONE', #26102, 39.37007874015748143 ) ;
#6230 = ORIENTED_EDGE ( 'NONE', *, *, #43146, .T. ) ;
#6231 = CARTESIAN_POINT ( 'NONE',  ( 0.2727639067037604947, 3.346456692913386100, -0.7874015748031473194 ) ) ;
#6232 = CARTESIAN_POINT ( 'NONE',  ( 1.091055626815042423, 3.267716535433071279, -1.456692913385822630 ) ) ;
#6233 = AXIS2_PLACEMENT_3D ( 'NONE', #27870, #23752, #47462 ) ;
#6234 = EDGE_CURVE ( 'NONE', #21432, #23486, #19451, .T. ) ;
#6235 = EDGE_LOOP ( 'NONE', ( #38994, #17685, #26554, #42471 ) ) ;
#6236 = ORIENTED_EDGE ( 'NONE', *, *, #33273, .F. ) ;
#6237 = VECTOR ( 'NONE', #3237, 39.37007874015748143 ) ;
#6238 = CARTESIAN_POINT ( 'NONE',  ( -1.377952755905513360, 0.000000000000000000, 2.165354330708661568 ) ) ;
#6239 = EDGE_LOOP ( 'NONE', ( #24602, #3170, #6731, #40250 ) ) ;
#6240 = ORIENTED_EDGE ( 'NONE', *, *, #26128, .F. ) ;
#6241 = DIRECTION ( 'NONE',  ( 1.734723475976806848E-16, 0.000000000000000000, 1.000000000000000000 ) ) ;
#6242 = DIRECTION ( 'NONE',  ( -0.000000000000000000, 1.000000000000000000, -0.000000000000000000 ) ) ;
#6243 = LINE ( 'NONE', #14235, #45895 ) ;
#6244 = ORIENTED_EDGE ( 'NONE', *, *, #24518, .T. ) ;
#6245 = LINE ( 'NONE', #6506, #46077 ) ;
#6246 = CYLINDRICAL_SURFACE ( 'NONE', #29138, 2.164630168518208109 ) ;
#6247 = CARTESIAN_POINT ( 'NONE',  ( 1.909347346926324684, 3.346456692913386100, 0.7874015748031456541 ) ) ;
#6248 = ORIENTED_EDGE ( 'NONE', *, *, #35882, .F. ) ;
#6249 = FACE_OUTER_BOUND ( 'NONE', #38560, .T. ) ;
#6250 = DIRECTION ( 'NONE',  ( -1.000000000000000000, 0.000000000000000000, 0.000000000000000000 ) ) ;
#6251 = PLANE ( 'NONE',  #1763 ) ;
#6252 = VERTEX_POINT ( 'NONE', #44575 ) ;
#6253 = EDGE_LOOP ( 'NONE', ( #7730, #26426, #44255, #12733 ) ) ;
#6254 = CARTESIAN_POINT ( 'NONE',  ( -0.2727639067037611054, 3.346456692913386100, -2.148105963102950877 ) ) ;
#6255 = EDGE_CURVE ( 'NONE', #11567, #34201, #40725, .T. ) ;
#6256 = EDGE_CURVE ( 'NONE', #44591, #8682, #13925, .T. ) ;
#6257 = LINE ( 'NONE', #3140, #5531 ) ;
#6258 = CARTESIAN_POINT ( 'NONE',  ( 0.7518624479397288951, 1.654327608218965073, 2.143387597788184440 ) ) ;
#6259 = ORIENTED_EDGE ( 'NONE', *, *, #48985, .F. ) ;
#6261 = EDGE_CURVE ( 'NONE', #45433, #41060, #8714, .T. ) ;
#6260 = ORIENTED_EDGE ( 'NONE', *, *, #22999, .F. ) ;
#6262 = VECTOR ( 'NONE', #1058, 39.37007874015748143 ) ;
#6263 = VECTOR ( 'NONE', #18733, 39.37007874015748143 ) ;
#6264 = CARTESIAN_POINT ( 'NONE',  ( -1.712496953225537633, 0.000000000000000000, 1.417322834645662333 ) ) ;
#6265 = B_SPLINE_CURVE_WITH_KNOTS ( 'NONE', 3,
 ( #50957, #42755, #23138, #43253 ),
 .UNSPECIFIED., .F., .F.,
 ( 4, 4 ),
 ( 3.515646365857402650E-07, 0.04348590293487804986 ),
 .UNSPECIFIED. ) ;
#6266 = ORIENTED_EDGE ( 'NONE', *, *, #25856, .T. ) ;
#6267 = DIRECTION ( 'NONE',  ( -0.9998717552508122886, -0.01601477604151185785, 0.000000000000000000 ) ) ;
#6268 = LINE ( 'NONE', #13000, #21823 ) ;
#6269 = AXIS2_PLACEMENT_3D ( 'NONE', #46942, #39493, #769 ) ;
#6270 = VECTOR ( 'NONE', #592, 39.37007874015748143 ) ;
#6271 = CARTESIAN_POINT ( 'NONE',  ( -2.182111253630085734, 0.000000000000000000, -0.6299212598425177889 ) ) ;
#6272 = CARTESIAN_POINT ( 'NONE',  ( 0.2727639067037604947, 3.267716535433071279, 0.7874015748031454320 ) ) ;
#6273 = CARTESIAN_POINT ( 'NONE',  ( 0.000000000000000000, 6.692913385826772199, 0.000000000000000000 ) ) ;
#6274 = VECTOR ( 'NONE', #16580, 39.37007874015748143 ) ;
#6275 = EDGE_LOOP ( 'NONE', ( #11530, #27050, #40743, #24401 ) ) ;
#6276 = FACE_OUTER_BOUND ( 'NONE', #22961, .T. ) ;
#6277 = DIRECTION ( 'NONE',  ( 0.000000000000000000, 1.160734090543304660E-16, -1.000000000000000000 ) ) ;
#6278 = EDGE_CURVE ( 'NONE', #1290, #26492, #28581, .T. ) ;
#6279 = CARTESIAN_POINT ( 'NONE',  ( 2.009025172380753066, 0.000000000000000000, 0.7045170369349440520 ) ) ;
#6280 = ORIENTED_EDGE ( 'NONE', *, *, #18103, .F. ) ;
#6281 = DIRECTION ( 'NONE',  ( 1.000000000000000000, 0.000000000000000000, 0.000000000000000000 ) ) ;
#6282 = EDGE_CURVE ( 'NONE', #37890, #38377, #3467, .T. ) ;
#6283 = CARTESIAN_POINT ( 'NONE',  ( 1.966928503432568975, 3.346456692913386100, 0.9055118110236164419 ) ) ;
#6284 = DIRECTION ( 'NONE',  ( -0.000000000000000000, -1.000000000000000000, -0.000000000000000000 ) ) ;
#6285 = ORIENTED_EDGE ( 'NONE', *, *, #46946, .F. ) ;
#6286 = EDGE_CURVE ( 'NONE', #48366, #24319, #44827, .T. ) ;
#6287 = DIRECTION ( 'NONE',  ( 1.734723475976806848E-16, 0.000000000000000000, 1.000000000000000000 ) ) ;
#6288 = EDGE_CURVE ( 'NONE', #4024, #49804, #24725, .T. ) ;
#6289 = EDGE_CURVE ( 'NONE', #20175, #25737, #24970, .T. ) ;
#6290 = ORIENTED_EDGE ( 'NONE', *, *, #29344, .F. ) ;
#6291 = DIRECTION ( 'NONE',  ( -0.000000000000000000, 0.000000000000000000, 1.000000000000000000 ) ) ;
#6292 = LINE ( 'NONE', #37543, #19195 ) ;
#6293 = VERTEX_POINT ( 'NONE', #32996 ) ;
#6294 = LINE ( 'NONE', #14800, #13046 ) ;
#6295 = CARTESIAN_POINT ( 'NONE',  ( 0.000000000000000000, 2.344748451760389596, -2.874015748031496731 ) ) ;
#6296 = DIRECTION ( 'NONE',  ( -3.469446951953613696E-16, 0.000000000000000000, -1.000000000000000000 ) ) ;
#6297 = CARTESIAN_POINT ( 'NONE',  ( 1.598949220451570508, 0.5249316497054297148, -0.9964897591775290220 ) ) ;
#6298 = VECTOR ( 'NONE', #2400, 39.37007874015748143 ) ;
#6299 = ORIENTED_EDGE ( 'NONE', *, *, #5096, .T. ) ;
#6300 = ORIENTED_EDGE ( 'NONE', *, *, #5616, .T. ) ;
#6301 = DIRECTION ( 'NONE',  ( 1.000000000000000000, 0.000000000000000000, 0.000000000000000000 ) ) ;
#6302 = AXIS2_PLACEMENT_3D ( 'NONE', #5446, #33600, #25831 ) ;
#6303 = CARTESIAN_POINT ( 'NONE',  ( 0.002207914879453961969, 5.905511811023623991, 0.04916304461325442243 ) ) ;
#6304 = VECTOR ( 'NONE', #16998, 39.37007874015748143 ) ;
#6305 = ORIENTED_EDGE ( 'NONE', *, *, #15139, .T. ) ;
#6306 = LINE ( 'NONE', #48858, #1183 ) ;
#6307 = CARTESIAN_POINT ( 'NONE',  ( 0.000000000000000000, 3.267716535433071279, -1.259842519685035134 ) ) ;
#6308 = CARTESIAN_POINT ( 'NONE',  ( 2.182111253630085290, 3.267716535433071279, -3.785359618865289765E-16 ) ) ;
#6309 = CIRCLE ( 'NONE', #38448, 2.165354330708661568 ) ;
#6310 = ORIENTED_EDGE ( 'NONE', *, *, #44784, .T. ) ;
#6311 = EDGE_LOOP ( 'NONE', ( #10821, #43405, #37434, #23378 ) ) ;
#6312 = CARTESIAN_POINT ( 'NONE',  ( -1.909347346926324906, 3.346456692913386100, 1.220472440944875059 ) ) ;
#6313 = DIRECTION ( 'NONE',  ( -0.000000000000000000, 1.000000000000000000, -0.000000000000000000 ) ) ;
#6314 = VECTOR ( 'NONE', #29305, 39.37007874015748143 ) ;
#6315 = CARTESIAN_POINT ( 'NONE',  ( 2.437180031585944207, 1.205361022782829114E-17, -1.667735833703099413 ) ) ;
#6316 = ORIENTED_EDGE ( 'NONE', *, *, #49811, .T. ) ;
#6317 = B_SPLINE_CURVE_WITH_KNOTS ( 'NONE', 3,
 ( #19994, #35759, #24657, #36788 ),
 .UNSPECIFIED., .F., .F.,
 ( 4, 4 ),
 ( 5.974790683084733931E-07, 3.893004845545902756E-05 ),
 .UNSPECIFIED. ) ;
#6318 = CARTESIAN_POINT ( 'NONE',  ( -2.139038182717881487, 1.575216142802386754, 0.3394144611327329364 ) ) ;
#6320 = AXIS2_PLACEMENT_3D ( 'NONE', #3002, #45574, #41735 ) ;
#6319 = LINE ( 'NONE', #22065, #18654 ) ;
#6321 = ORIENTED_EDGE ( 'NONE', *, *, #44854, .T. ) ;
#6322 = LINE ( 'NONE', #21554, #33995 ) ;
#6323 = ORIENTED_EDGE ( 'NONE', *, *, #42210, .F. ) ;
#6324 = ORIENTED_EDGE ( 'NONE', *, *, #27947, .F. ) ;
#6325 = DIRECTION ( 'NONE',  ( 1.000000000000000000, 0.000000000000000000, 0.000000000000000000 ) ) ;
#6326 = DIRECTION ( 'NONE',  ( -0.9998717552508122886, -0.01601477604151185785, 0.000000000000000000 ) ) ;
#6327 = DIRECTION ( 'NONE',  ( 0.000000000000000000, -1.000000000000000000, 0.000000000000000000 ) ) ;
#6328 = ORIENTED_EDGE ( 'NONE', *, *, #1012, .F. ) ;
#6329 = CARTESIAN_POINT ( 'NONE',  ( -1.909347346926324906, 0.000000000000000000, -0.7874015748031470974 ) ) ;
#6330 = CARTESIAN_POINT ( 'NONE',  ( 2.126910391174609671, 1.205361022782829114E-17, 0.2384475364948296372 ) ) ;
#6331 = ORIENTED_EDGE ( 'NONE', *, *, #46049, .T. ) ;
#6332 = ADVANCED_FACE ( 'NONE', ( #32219 ), #48674, .F. ) ;
#6333 = EDGE_CURVE ( 'NONE', #47259, #5956, #13359, .T. ) ;
#6334 = ORIENTED_EDGE ( 'NONE', *, *, #18126, .T. ) ;
#6335 = CARTESIAN_POINT ( 'NONE',  ( -1.636583440222563635, 3.346456692913386100, -0.1968503937007879123 ) ) ;
#6336 = ADVANCED_FACE ( 'NONE', ( #5609 ), #32742, .F. ) ;
#6337 = DIRECTION ( 'NONE',  ( 1.000000000000000000, 0.000000000000000000, 0.000000000000000000 ) ) ;
#6338 = CIRCLE ( 'NONE', #41785, 2.165354330708661568 ) ;
#6339 = LINE ( 'NONE', #22086, #37999 ) ;
#6340 = DIRECTION ( 'NONE',  ( 1.734723475976806848E-16, 0.000000000000000000, 1.000000000000000000 ) ) ;
#6341 = CARTESIAN_POINT ( 'NONE',  ( -1.439733046521776583, 3.267716535433071279, -1.617383112398506295 ) ) ;
#6342 = ORIENTED_EDGE ( 'NONE', *, *, #7399, .T. ) ;
#6343 = CARTESIAN_POINT ( 'NONE',  ( -0.3486774197067334935, 0.000000000000000000, 1.062992125984246083 ) ) ;
#6344 = AXIS2_PLACEMENT_3D ( 'NONE', #44786, #21571, #25692 ) ;
#6345 = DIRECTION ( 'NONE',  ( 1.734723475976806848E-16, 0.000000000000000000, 1.000000000000000000 ) ) ;
#6346 = ORIENTED_EDGE ( 'NONE', *, *, #10074, .F. ) ;
#6347 = CARTESIAN_POINT ( 'NONE',  ( -0.9838852166859199944, 1.205361022782829114E-17, 1.929635236160303302 ) ) ;
#6348 = EDGE_CURVE ( 'NONE', #48222, #45550, #16726, .T. ) ;
#6349 = CARTESIAN_POINT ( 'NONE',  ( 1.833433833923351353, 0.000000000000000000, -0.9448818897637765168 ) ) ;
#6350 = ORIENTED_EDGE ( 'NONE', *, *, #14354, .T. ) ;
#6351 = CARTESIAN_POINT ( 'NONE',  ( -0.2727639067037607723, 0.000000000000000000, -1.102362204724405714 ) ) ;
#6352 = AXIS2_PLACEMENT_3D ( 'NONE', #43377, #39009, #43882 ) ;
#6353 = LINE ( 'NONE', #49417, #22550 ) ;
#6354 = CARTESIAN_POINT ( 'NONE',  ( 0.1067246931122726866, 0.02962905676920215767, 0.000000000000000000 ) ) ;
#6355 = VECTOR ( 'NONE', #3441, 39.37007874015748143 ) ;
#6356 = EDGE_CURVE ( 'NONE', #33511, #43816, #14532, .T. ) ;
#6357 = ORIENTED_EDGE ( 'NONE', *, *, #3745, .T. ) ;
#6358 = DIRECTION ( 'NONE',  ( 1.000000000000000000, 0.000000000000000000, -3.469446951953613696E-16 ) ) ;
#6359 = ORIENTED_EDGE ( 'NONE', *, *, #3625, .T. ) ;
#6360 = FACE_BOUND ( 'NONE', #50352, .T. ) ;
#6361 = CARTESIAN_POINT ( 'NONE',  ( 2.576863348864710801, 1.456480680773285741, 1.442554885838449596 ) ) ;
#6362 = DIRECTION ( 'NONE',  ( -0.9998717552508121775, -0.01601477604151182663, 0.000000000000000000 ) ) ;
#6363 = B_SPLINE_CURVE_WITH_KNOTS ( 'NONE', 3,
 ( #10059, #13937, #45647, #37435 ),
 .UNSPECIFIED., .F., .F.,
 ( 4, 4 ),
 ( 3.949417831791902674E-07, 0.04989286874765130886 ),
 .UNSPECIFIED. ) ;
#6364 = LINE ( 'NONE', #29851, #30122 ) ;
#6365 = ORIENTED_EDGE ( 'NONE', *, *, #629, .F. ) ;
#6366 = VERTEX_POINT ( 'NONE', #17483 ) ;
#6367 = DIRECTION ( 'NONE',  ( 1.000000000000000000, 0.000000000000000000, 0.000000000000000000 ) ) ;
#6368 = CARTESIAN_POINT ( 'NONE',  ( 1.363819533518803695, 0.000000000000000000, 1.535433070866133898 ) ) ;
#6369 = VERTEX_POINT ( 'NONE', #715 ) ;
#6370 = CARTESIAN_POINT ( 'NONE',  ( -1.299599272623047641, 1.691095615222215187, 2.079212968904131209 ) ) ;
#6371 = ORIENTED_EDGE ( 'NONE', *, *, #18228, .F. ) ;
#6372 = DIRECTION ( 'NONE',  ( 1.000000000000000000, 0.000000000000000000, 0.000000000000000000 ) ) ;
#6373 = VECTOR ( 'NONE', #2117, 39.37007874015748143 ) ;
#6374 = VECTOR ( 'NONE', #10973, 39.37007874015748143 ) ;
#6375 = DIRECTION ( 'NONE',  ( 0.000000000000000000, 1.000000000000000000, 0.000000000000000000 ) ) ;
#6376 = VECTOR ( 'NONE', #24687, 39.37007874015748143 ) ;
#6377 = ORIENTED_EDGE ( 'NONE', *, *, #12871, .T. ) ;
#6378 = CARTESIAN_POINT ( 'NONE',  ( 0.8182917201112824834, 3.346456692913386100, 2.004783788421103718 ) ) ;
#6379 = ORIENTED_EDGE ( 'NONE', *, *, #13843, .F. ) ;
#6380 = ORIENTED_EDGE ( 'NONE', *, *, #3682, .T. ) ;
#6381 =( BOUNDED_CURVE ( )  B_SPLINE_CURVE ( 3, ( #27943, #36217, #27683, #28447 ),
 .UNSPECIFIED., .F., .F. ) 
 B_SPLINE_CURVE_WITH_KNOTS ( ( 4, 4 ),
 ( 2.171587567367763594, 2.222479831755601598 ),
 .UNSPECIFIED. ) 
 CURVE ( )  GEOMETRIC_REPRESENTATION_ITEM ( )  RATIONAL_B_SPLINE_CURVE ( ( 1.000000000000000000, 0.9997841764314150392, 0.9997841764314150392, 1.000000000000000000 ) ) 
 REPRESENTATION_ITEM ( '' )  );
#6382 = EDGE_LOOP ( 'NONE', ( #6674, #14163, #48326, #19794 ) ) ;
#6383 = ORIENTED_EDGE ( 'NONE', *, *, #45134, .F. ) ;
#6384 = DIRECTION ( 'NONE',  ( 1.000000000000000000, 0.000000000000000000, 0.000000000000000000 ) ) ;
#6385 = EDGE_CURVE ( 'NONE', #4189, #47727, #16464, .T. ) ;
#6386 = ADVANCED_FACE ( 'NONE', ( #28322 ), #44072, .F. ) ;
#6387 = B_SPLINE_CURVE_WITH_KNOTS ( 'NONE', 3,
 ( #2459, #18452, #7586, #45790 ),
 .UNSPECIFIED., .F., .F.,
 ( 4, 4 ),
 ( 2.271194390675191284E-07, 0.01981312671808579604 ),
 .UNSPECIFIED. ) ;
#6388 = ORIENTED_EDGE ( 'NONE', *, *, #7469, .F. ) ;
#6390 = DIRECTION ( 'NONE',  ( -0.000000000000000000, 1.000000000000000000, -0.000000000000000000 ) ) ;
#6389 = CIRCLE ( 'NONE', #35240, 2.164630168518208109 ) ;
#6391 = CARTESIAN_POINT ( 'NONE',  ( 1.287906020515830141, 0.000000000000000000, 1.259842519685033357 ) ) ;
#6392 = EDGE_CURVE ( 'NONE', #26276, #43980, #34003, .T. ) ;
#6393 = PRODUCT_RELATED_PRODUCT_CATEGORY ( 'part', '', ( #50723 ) ) ;
#6394 = EDGE_CURVE ( 'NONE', #16625, #33493, #9986, .T. ) ;
#6395 = CARTESIAN_POINT ( 'NONE',  ( 2.106197740627111958, 3.267716535433071279, -7.307341331430321661E-16 ) ) ;
#6396 = DIRECTION ( 'NONE',  ( 1.734723475976806848E-16, 0.000000000000000000, 1.000000000000000000 ) ) ;
#6397 = CARTESIAN_POINT ( 'NONE',  ( 0.08119777152254364916, 1.623385212329073957, 0.000000000000000000 ) ) ;
#6398 = VERTEX_POINT ( 'NONE', #37371 ) ;
#6399 = CARTESIAN_POINT ( 'NONE',  ( -1.166969139818016199, 3.267716535433071279, -1.929133858267710000 ) ) ;
#6400 = DIRECTION ( 'NONE',  ( -0.000000000000000000, 1.000000000000000000, -0.000000000000000000 ) ) ;
#6401 = CARTESIAN_POINT ( 'NONE',  ( 2.533192966889194597, 1.751833986009839306, -0.06450362513773535977 ) ) ;
#6402 = DIRECTION ( 'NONE',  ( 0.8805955318567321166, 0.000000000000000000, 0.4738686624730094055 ) ) ;
#6403 = ORIENTED_EDGE ( 'NONE', *, *, #42440, .T. ) ;
#6404 = CARTESIAN_POINT ( 'NONE',  ( -1.030376884852511887, 0.4561333243160197171, -1.046684505418382205 ) ) ;
#6405 = EDGE_CURVE ( 'NONE', #10848, #3242, #37622, .T. ) ;
#6406 = CARTESIAN_POINT ( 'NONE',  ( 2.004210316087306154, 1.645011016312011520, 1.535359116834265070 ) ) ;
#6407 = VERTEX_POINT ( 'NONE', #21869 ) ;
#6408 = CARTESIAN_POINT ( 'NONE',  ( -1.002259110181423551, 1.593423740086483020, -1.967789019142131002 ) ) ;
#6409 = VECTOR ( 'NONE', #42360, 39.37007874015748143 ) ;
#6410 = AXIS2_PLACEMENT_3D ( 'NONE', #27403, #39286, #40054 ) ;
#6411 = CARTESIAN_POINT ( 'NONE',  ( -2.100227814008681637, 1.686526752338742385, -2.076109931251943763 ) ) ;
#6412 = ORIENTED_EDGE ( 'NONE', *, *, #29170, .F. ) ;
#6413 = EDGE_CURVE ( 'NONE', #19556, #45614, #38380, .T. ) ;
#6414 = VECTOR ( 'NONE', #14754, 39.37007874015748143 ) ;
#6415 = ORIENTED_EDGE ( 'NONE', *, *, #25695, .F. ) ;
#6416 = DIRECTION ( 'NONE',  ( -0.2660368455666826670, 0.000000000000000000, 0.9639628606958512425 ) ) ;
#6417 = CARTESIAN_POINT ( 'NONE',  ( 1.287906020515830585, 0.000000000000000000, 1.889763779527550369 ) ) ;
#6418 = CARTESIAN_POINT ( 'NONE',  ( 1.909347346926324462, 3.267716535433071279, -1.102362204724406602 ) ) ;
#6419 = DIRECTION ( 'NONE',  ( -1.000000000000000000, 0.000000000000000000, 0.000000000000000000 ) ) ;
#6420 = FACE_OUTER_BOUND ( 'NONE', #46991, .T. ) ;
#6421 = ORIENTED_EDGE ( 'NONE', *, *, #8905, .T. ) ;
#6422 = DIRECTION ( 'NONE',  ( 0.000000000000000000, 0.000000000000000000, -1.000000000000000000 ) ) ;
#6423 = EDGE_LOOP ( 'NONE', ( #15930, #4900, #3819, #49354, #12414 ) ) ;
#6424 = ORIENTED_EDGE ( 'NONE', *, *, #13516, .F. ) ;
#6425 = FACE_OUTER_BOUND ( 'NONE', #6040, .T. ) ;
#6426 = EDGE_LOOP ( 'NONE', ( #44265, #38596, #35419, #50765 ) ) ;
#6427 = CARTESIAN_POINT ( 'NONE',  ( 0.000000000000000000, 3.267716535433071279, -0.7874015748031467643 ) ) ;
#6428 = AXIS2_PLACEMENT_3D ( 'NONE', #46803, #11719, #30338 ) ;
#6429 = PLANE ( 'NONE',  #35091 ) ;
#6430 = EDGE_CURVE ( 'NONE', #5697, #17250, #50192, .T. ) ;
#6431 = ORIENTED_EDGE ( 'NONE', *, *, #39130, .T. ) ;
#6432 = DIRECTION ( 'NONE',  ( -0.000000000000000000, -1.000000000000000000, -0.000000000000000000 ) ) ;
#6433 = DIRECTION ( 'NONE',  ( -0.9998717552508122886, -0.01601477604151180928, 0.000000000000000000 ) ) ;
#6434 = LINE ( 'NONE', #33304, #10714 ) ;
#6435 = VERTEX_POINT ( 'NONE', #2749 ) ;
#6436 = ORIENTED_EDGE ( 'NONE', *, *, #2754, .T. ) ;
#6437 = FACE_OUTER_BOUND ( 'NONE', #16229, .T. ) ;
#6438 = FACE_BOUND ( 'NONE', #13813, .T. ) ;
#6439 = EDGE_LOOP ( 'NONE', ( #23840, #50761, #42513, #42633 ) ) ;
#6440 = CARTESIAN_POINT ( 'NONE',  ( -1.439733046521776361, 3.346456692913386100, 0.7480314960629874665 ) ) ;
#6441 = DIRECTION ( 'NONE',  ( -0.000000000000000000, 1.000000000000000000, -0.000000000000000000 ) ) ;
#6442 = AXIS2_PLACEMENT_3D ( 'NONE', #30544, #10416, #30292 ) ;
#6444 = VECTOR ( 'NONE', #50476, 39.37007874015748143 ) ;
#6443 = B_SPLINE_CURVE_WITH_KNOTS ( 'NONE', 3,
 ( #6656, #27273, #43014, #3794 ),
 .UNSPECIFIED., .F., .F.,
 ( 4, 4 ),
 ( 0.001673364190201165683, 0.04575664440331616428 ),
 .UNSPECIFIED. ) ;
#6445 = ORIENTED_EDGE ( 'NONE', *, *, #23852, .T. ) ;
#6446 = ORIENTED_EDGE ( 'NONE', *, *, #36929, .T. ) ;
#6447 = CARTESIAN_POINT ( 'NONE',  ( 0.000000000000000000, 5.118110236220475784, 0.000000000000000000 ) ) ;
#6448 = CARTESIAN_POINT ( 'NONE',  ( 1.556712866041120469, 1.205361022782829114E-17, 2.509548638715870084 ) ) ;
#6449 = VERTEX_POINT ( 'NONE', #41992 ) ;
#6450 = EDGE_LOOP ( 'NONE', ( #14283, #2781, #17082, #7057 ) ) ;
#6451 = AXIS2_PLACEMENT_3D ( 'NONE', #28205, #44708, #9104 ) ;
#6452 = ORIENTED_EDGE ( 'NONE', *, *, #19765, .T. ) ;
#6453 = PLANE ( 'NONE',  #9543 ) ;
#6454 = EDGE_CURVE ( 'NONE', #15353, #34370, #41485, .T. ) ;
#6455 = LINE ( 'NONE', #26323, #23354 ) ;
#6456 = AXIS2_PLACEMENT_3D ( 'NONE', #47246, #8563, #11925 ) ;
#6457 = EDGE_CURVE ( 'NONE', #20260, #32968, #14370, .T. ) ;
#6458 = CARTESIAN_POINT ( 'NONE',  ( 1.953585199828834940, 3.346456692913386100, -0.7874015748031473194 ) ) ;
#6459 = EDGE_CURVE ( 'NONE', #50666, #29472, #42854, .T. ) ;
#6460 = CARTESIAN_POINT ( 'NONE',  ( -0.07591351300297333182, 0.000000000000000000, -0.7874015748031470974 ) ) ;
#6461 = AXIS2_PLACEMENT_3D ( 'NONE', #44782, #4095, #47153 ) ;
#6462 = ORIENTED_EDGE ( 'NONE', *, *, #47253, .T. ) ;
#6463 = ORIENTED_EDGE ( 'NONE', *, *, #34764, .T. ) ;
#6464 = LINE ( 'NONE', #2582, #48010 ) ;
#6465 = CARTESIAN_POINT ( 'NONE',  ( 2.160407304981128984, 6.692913385826772199, -0.1462862061266579361 ) ) ;
#6466 = DIRECTION ( 'NONE',  ( 0.5508969814520945363, -9.689372162470668980E-17, 0.8345732537213079727 ) ) ;
#6467 = VECTOR ( 'NONE', #25632, 39.37007874015748143 ) ;
#6468 = FACE_OUTER_BOUND ( 'NONE', #25943, .T. ) ;
#6469 = CARTESIAN_POINT ( 'NONE',  ( -0.1227720337126170513, 0.000000000000000000, -1.913115909999223652 ) ) ;
#6470 = CARTESIAN_POINT ( 'NONE',  ( 1.909347346926324684, 3.346456692913386100, 0.9055118110236164419 ) ) ;
#6471 = LINE ( 'NONE', #3095, #35787 ) ;
#6472 = ORIENTED_EDGE ( 'NONE', *, *, #47592, .F. ) ;
#6473 = LINE ( 'NONE', #30972, #2812 ) ;
#6474 = DIRECTION ( 'NONE',  ( 1.000000000000000000, 0.000000000000000000, 0.000000000000000000 ) ) ;
#6475 = EDGE_LOOP ( 'NONE', ( #36449, #39268, #7132, #48029 ) ) ;
#6476 = VERTEX_POINT ( 'NONE', #6629 ) ;
#6477 = CARTESIAN_POINT ( 'NONE',  ( 2.100190309385009169, 1.205361022782829114E-17, 0.5298329251847523347 ) ) ;
#6478 = CIRCLE ( 'NONE', #22140, 2.165354330708661568 ) ;
#6479 = VERTEX_POINT ( 'NONE', #18755 ) ;
#6480 = EDGE_CURVE ( 'NONE', #7243, #4778, #14879, .T. ) ;
#6481 = B_SPLINE_CURVE_WITH_KNOTS ( 'NONE', 3,
 ( #37720, #21963, #17827, #9573 ),
 .UNSPECIFIED., .F., .F.,
 ( 4, 4 ),
 ( 0.02665634820260516513, 0.02770374167893049910 ),
 .UNSPECIFIED. ) ;
#6482 = ORIENTED_EDGE ( 'NONE', *, *, #16410, .T. ) ;
#6483 = DIRECTION ( 'NONE',  ( -0.000000000000000000, 1.000000000000000000, -0.000000000000000000 ) ) ;
#6484 = VECTOR ( 'NONE', #28886, 39.37007874015748143 ) ;
#6485 = EDGE_CURVE ( 'NONE', #13805, #10560, #33501, .T. ) ;
#6486 = ORIENTED_EDGE ( 'NONE', *, *, #21549, .F. ) ;
#6487 = AXIS2_PLACEMENT_3D ( 'NONE', #25166, #17419, #24662 ) ;
#6488 = VECTOR ( 'NONE', #13404, 39.37007874015748143 ) ;
#6489 = CARTESIAN_POINT ( 'NONE',  ( -1.636583440222564301, 0.000000000000000000, -1.574803149606293307 ) ) ;
#6490 = CARTESIAN_POINT ( 'NONE',  ( 1.669153017917641924, 1.205361022782829114E-17, 1.268159837793114031 ) ) ;
#6491 = VECTOR ( 'NONE', #2003, 39.37007874015748143 ) ;
#6492 = VERTEX_POINT ( 'NONE', #22377 ) ;
#6493 = ORIENTED_EDGE ( 'NONE', *, *, #11840, .F. ) ;
#6494 = LINE ( 'NONE', #49551, #19722 ) ;
#6495 = ORIENTED_EDGE ( 'NONE', *, *, #30047, .F. ) ;
#6496 = ORIENTED_EDGE ( 'NONE', *, *, #36635, .T. ) ;
#6497 = EDGE_CURVE ( 'NONE', #23861, #16084, #46342, .T. ) ;
#6498 = PLANE ( 'NONE',  #22372 ) ;
#6499 = CARTESIAN_POINT ( 'NONE',  ( 0.8182917201112819283, 0.000000000000000000, -0.1574803149606301411 ) ) ;
#6500 = DIRECTION ( 'NONE',  ( -3.469446951953613696E-16, 0.000000000000000000, -1.000000000000000000 ) ) ;
#6501 = LINE ( 'NONE', #22246, #37575 ) ;
#6502 = VECTOR ( 'NONE', #3797, 39.37007874015748143 ) ;
#6503 = EDGE_CURVE ( 'NONE', #4956, #37208, #34257, .T. ) ;
#6504 = VERTEX_POINT ( 'NONE', #11005 ) ;
#6505 = CIRCLE ( 'NONE', #18035, 2.165354330708661568 ) ;
#6506 = CARTESIAN_POINT ( 'NONE',  ( -1.363819533518803473, 0.000000000000000000, -1.732283464566922726 ) ) ;
#6507 = CARTESIAN_POINT ( 'NONE',  ( -1.439733046521776139, 0.000000000000000000, 0.9448818897637749625 ) ) ;
#6508 = PLANE ( 'NONE',  #35259 ) ;
#6509 = ORIENTED_EDGE ( 'NONE', *, *, #33749, .T. ) ;
#6510 = CARTESIAN_POINT ( 'NONE',  ( 2.823445274216730638, 1.450545469922353892, 0.8656477926280681245 ) ) ;
#6511 = CARTESIAN_POINT ( 'NONE',  ( -2.142325647309101022, 3.346456692913386100, -0.3149606299212589500 ) ) ;
#6512 = DIRECTION ( 'NONE',  ( 1.000000000000000000, 0.000000000000000000, 0.000000000000000000 ) ) ;
#6513 = ORIENTED_EDGE ( 'NONE', *, *, #13321, .T. ) ;
#6514 = ORIENTED_EDGE ( 'NONE', *, *, #22921, .F. ) ;
#6515 =( NAMED_UNIT ( * ) SI_UNIT ( $, .STERADIAN. ) SOLID_ANGLE_UNIT ( ) );
#6516 = ADVANCED_FACE ( 'NONE', ( #7136 ), #15749, .T. ) ;
#6517 = CARTESIAN_POINT ( 'NONE',  ( -1.363819533518803029, 3.346456692913386100, 1.102362204724404160 ) ) ;
#6518 = AXIS2_PLACEMENT_3D ( 'NONE', #48606, #36528, #33431 ) ;
#6519 = DIRECTION ( 'NONE',  ( -0.000000000000000000, 1.000000000000000000, -0.000000000000000000 ) ) ;
#6520 = EDGE_CURVE ( 'NONE', #28976, #50937, #9884, .T. ) ;
#6521 = EDGE_CURVE ( 'NONE', #19510, #6110, #38040, .T. ) ;
#6522 = DIRECTION ( 'NONE',  ( 0.000000000000000000, -1.000000000000000000, 0.000000000000000000 ) ) ;
#6523 = ORIENTED_EDGE ( 'NONE', *, *, #30910, .T. ) ;
#6524 = EDGE_LOOP ( 'NONE', ( #36692, #15073, #9338, #3919, #2808, #9299, #44307, #31432, #4096, #19910, #40163 ) ) ;
#6525 = EDGE_CURVE ( 'NONE', #45880, #42094, #22124, .T. ) ;
#6526 = CARTESIAN_POINT ( 'NONE',  ( 2.530770726936613535, 1.653353769313707478, -0.1629192465856815764 ) ) ;
#6527 = ORIENTED_EDGE ( 'NONE', *, *, #37396, .T. ) ;
#6528 = CARTESIAN_POINT ( 'NONE',  ( -1.363819533518803473, 3.346456692913386100, -0.9842519685039344823 ) ) ;
#6529 = DIRECTION ( 'NONE',  ( 1.000000000000000000, -0.000000000000000000, 0.000000000000000000 ) ) ;
#6530 = AXIS2_PLACEMENT_3D ( 'NONE', #2115, #14499, #2624 ) ;
#6531 = CIRCLE ( 'NONE', #23834, 1.850107469027523432 ) ;
#6532 = VECTOR ( 'NONE', #540, 39.37007874015748143 ) ;
#6533 = CARTESIAN_POINT ( 'NONE',  ( 2.141071258218635531, 0.000000000000000000, -0.04689341889560144638 ) ) ;
#6534 = CARTESIAN_POINT ( 'NONE',  ( 0.8182917201112819283, 3.346456692913386100, -0.9842519685039348154 ) ) ;
#6535 = DIRECTION ( 'NONE',  ( 0.000000000000000000, 0.000000000000000000, -1.000000000000000000 ) ) ;
#6536 = ORIENTED_EDGE ( 'NONE', *, *, #4523, .T. ) ;
#6537 = DIRECTION ( 'NONE',  ( -0.000000000000000000, 1.000000000000000000, -0.000000000000000000 ) ) ;
#6538 = DIRECTION ( 'NONE',  ( -0.5773502691896265082, 0.5773502691896255090, 0.5773502691896251759 ) ) ;
#6539 = VECTOR ( 'NONE', #5006, 39.37007874015748143 ) ;
#6540 = CARTESIAN_POINT ( 'NONE',  ( 2.106197740627111958, 3.267716535433071279, 0.9055118110236164419 ) ) ;
#6541 = EDGE_LOOP ( 'NONE', ( #46529, #40930, #38382, #43744, #16650, #46339, #47442, #17754, #43480, #32406, #4687 ) ) ;
#6542 = CARTESIAN_POINT ( 'NONE',  ( -0.1942989824301265822, 1.712426749178000751, -2.707845400019115001 ) ) ;
#6543 = CARTESIAN_POINT ( 'NONE',  ( -2.099568260077699033, 1.574803149606302854, -0.5296909464896101261 ) ) ;
#6544 = CARTESIAN_POINT ( 'NONE',  ( 0.7423782071083087075, 3.267716535433071279, 0.9448818897637746295 ) ) ;
#6545 = EDGE_LOOP ( 'NONE', ( #39801, #14153, #16070, #25236 ) ) ;
#6546 = ADVANCED_FACE ( 'NONE', ( #14630 ), #13342, .T. ) ;
#6547 = PLANE ( 'NONE',  #44836 ) ;
#6548 = ORIENTED_EDGE ( 'NONE', *, *, #38395, .T. ) ;
#6549 = DIRECTION ( 'NONE',  ( -1.000000000000000000, -0.000000000000000000, -0.000000000000000000 ) ) ;
#6550 = ORIENTED_EDGE ( 'NONE', *, *, #38906, .F. ) ;
#6551 = DIRECTION ( 'NONE',  ( 0.7227948638273978821, 8.018518666443169432E-17, -0.6910626489868580968 ) ) ;
#6552 = ADVANCED_FACE ( 'NONE', ( #42237 ), #43236, .F. ) ;
#6553 = LINE ( 'NONE', #11177, #47383 ) ;
#6554 = CARTESIAN_POINT ( 'NONE',  ( -0.8182917201112819283, 0.000000000000000000, -1.614173228346451605 ) ) ;
#6555 = DIRECTION ( 'NONE',  ( -3.469446951953613696E-16, 0.000000000000000000, -1.000000000000000000 ) ) ;
#6556 = EDGE_CURVE ( 'NONE', #19562, #36908, #27244, .T. ) ;
#6557 = AXIS2_PLACEMENT_3D ( 'NONE', #1080, #32859, #28952 ) ;
#6558 = ADVANCED_FACE ( 'NONE', ( #42984 ), #20001, .F. ) ;
#6559 = ORIENTED_EDGE ( 'NONE', *, *, #4527, .F. ) ;
#6560 = ORIENTED_EDGE ( 'NONE', *, *, #10814, .T. ) ;
#6561 = DIRECTION ( 'NONE',  ( -1.000000000000000000, -0.000000000000000000, -0.000000000000000000 ) ) ;
#6562 = DIRECTION ( 'NONE',  ( -0.000000000000000000, 1.000000000000000000, -0.000000000000000000 ) ) ;
#6563 = EDGE_LOOP ( 'NONE', ( #35935, #11011, #2704, #50121 ) ) ;
#6564 = DIRECTION ( 'NONE',  ( -0.000000000000000000, 1.000000000000000000, -0.000000000000000000 ) ) ;
#6565 = CARTESIAN_POINT ( 'NONE',  ( 2.793030215715258446, 0.000000000000000000, 0.9592557174602679426 ) ) ;
#6566 = FACE_OUTER_BOUND ( 'NONE', #41120, .T. ) ;
#6567 = CONICAL_SURFACE ( 'NONE', #20593, 1.850107469027523210, 0.6386652850508578450 ) ;
#6568 = ORIENTED_EDGE ( 'NONE', *, *, #17395, .T. ) ;
#6569 = ORIENTED_EDGE ( 'NONE', *, *, #40933, .F. ) ;
#6570 = LINE ( 'NONE', #2939, #19698 ) ;
#6571 = CARTESIAN_POINT ( 'NONE',  ( -0.8182917201112814842, 3.346456692913386100, 0.4724409448818872592 ) ) ;
#6572 = CARTESIAN_POINT ( 'NONE',  ( 0.2727639067037604947, 3.346456692913386100, 0.1574803149606283648 ) ) ;
#6573 = ORIENTED_EDGE ( 'NONE', *, *, #334, .T. ) ;
#6574 = AXIS2_PLACEMENT_3D ( 'NONE', #6792, #45752, #2666 ) ;
#6575 = FILL_AREA_STYLE ('',( #41932 ) ) ;
#6576 = CARTESIAN_POINT ( 'NONE',  ( 1.958513403246152640, 1.640845930445798073, -1.233835998176425308 ) ) ;
#6577 = VERTEX_POINT ( 'NONE', #23631 ) ;
#6578 = DIRECTION ( 'NONE',  ( 1.000000000000000000, 0.000000000000000000, 0.000000000000000000 ) ) ;
#6579 = ORIENTED_EDGE ( 'NONE', *, *, #1593, .T. ) ;
#6580 = ORIENTED_EDGE ( 'NONE', *, *, #2189, .F. ) ;
#6581 = EDGE_CURVE ( 'NONE', #37657, #41218, #12017, .T. ) ;
#6582 = VECTOR ( 'NONE', #30538, 39.37007874015748143 ) ;
#6583 = CARTESIAN_POINT ( 'NONE',  ( 2.867773316779195447, 1.665472095473279790, -0.7050287376752005786 ) ) ;
#6584 = CARTESIAN_POINT ( 'NONE',  ( 1.560669927219591413, 3.346456692913386100, 1.732283464566921172 ) ) ;
#6585 = EDGE_CURVE ( 'NONE', #35311, #29664, #11510, .T. ) ;
#6586 = CARTESIAN_POINT ( 'NONE',  ( 1.560669927219591413, 0.000000000000000000, 1.732283464566921172 ) ) ;
#6587 = LINE ( 'NONE', #27197, #20335 ) ;
#6588 = EDGE_CURVE ( 'NONE', #27292, #49048, #4023, .T. ) ;
#6590 = EDGE_CURVE ( 'NONE', #9082, #47888, #46590, .T. ) ;
#6589 = PRODUCT_DEFINITION_CONTEXT ( 'detailed design', #17053, 'design' ) ;
#6591 = DIRECTION ( 'NONE',  ( -1.000000000000000000, 0.000000000000000000, 0.000000000000000000 ) ) ;
#6592 = ORIENTED_EDGE ( 'NONE', *, *, #24832, .F. ) ;
#6593 = EDGE_CURVE ( 'NONE', #12364, #41352, #31134, .T. ) ;
#6594 = EDGE_LOOP ( 'NONE', ( #22079, #20118, #6216, #40919 ) ) ;
#6595 = DIRECTION ( 'NONE',  ( -1.000000000000000000, 0.000000000000000000, 1.734723475976806848E-16 ) ) ;
#6596 = VECTOR ( 'NONE', #42049, 39.37007874015748143 ) ;
#6597 = CARTESIAN_POINT ( 'NONE',  ( 0.000000000000000000, 1.574803149606302854, 0.000000000000000000 ) ) ;
#6598 = DIRECTION ( 'NONE',  ( -0.9998717552508122886, -0.01601477604151181275, 0.000000000000000000 ) ) ;
#6599 = CARTESIAN_POINT ( 'NONE',  ( 0.1067246931122726866, 0.02962905676920215767, 0.000000000000000000 ) ) ;
#6600 = VERTEX_POINT ( 'NONE', #7637 ) ;
#6601 = CARTESIAN_POINT ( 'NONE',  ( 1.833433833923351353, 3.267716535433071279, -6.361001426713998480E-16 ) ) ;
#6602 = CARTESIAN_POINT ( 'NONE',  ( 2.160407304981128984, 1.574803149606302854, -0.1462862061266585745 ) ) ;
#6603 = EDGE_LOOP ( 'NONE', ( #18318, #19202, #34390, #28044 ) ) ;
#6604 = CARTESIAN_POINT ( 'NONE',  ( 1.157218145390799036, 2.755905511811024056, 0.2363238328731523952 ) ) ;
#6605 = FACE_OUTER_BOUND ( 'NONE', #36274, .T. ) ;
#6606 = ORIENTED_EDGE ( 'NONE', *, *, #6556, .F. ) ;
#6607 = CARTESIAN_POINT ( 'NONE',  ( -2.019856298843366371, 1.049866565877817237, -0.1399740531627085005 ) ) ;
#6608 = CARTESIAN_POINT ( 'NONE',  ( -1.722370577523733459, 1.205361022782829114E-17, 0.2829729990490794655 ) ) ;
#6609 = DIRECTION ( 'NONE',  ( -1.000000000000000000, 0.000000000000000000, -0.000000000000000000 ) ) ;
#6610 = VERTEX_POINT ( 'NONE', #28013 ) ;
#6611 = DIRECTION ( 'NONE',  ( -0.01601477604151182663, 0.9998717552508123996, -0.000000000000000000 ) ) ;
#6612 = VECTOR ( 'NONE', #33864, 39.37007874015748143 ) ;
#6613 = ORIENTED_EDGE ( 'NONE', *, *, #42330, .T. ) ;
#6614 = DIRECTION ( 'NONE',  ( 0.000000000000000000, 1.000000000000000000, 0.000000000000000000 ) ) ;
#6615 = CARTESIAN_POINT ( 'NONE',  ( -1.712496953225537633, 3.346456692913386100, 1.226315847645293999 ) ) ;
#6616 = CARTESIAN_POINT ( 'NONE',  ( 1.287906020515830141, 3.267716535433071279, 0.9448818897637746295 ) ) ;
#6617 = LINE ( 'NONE', #33489, #49045 ) ;
#6618 = EDGE_CURVE ( 'NONE', #1749, #41218, #39125, .T. ) ;
#6619 = EDGE_CURVE ( 'NONE', #50789, #29175, #19499, .T. ) ;
#6620 = VERTEX_POINT ( 'NONE', #35007 ) ;
#6621 = EDGE_LOOP ( 'NONE', ( #32138, #36021, #47509, #6953 ) ) ;
#6622 = CARTESIAN_POINT ( 'NONE',  ( 0.000000000000000000, 3.267716535433071279, -0.5118110236220464460 ) ) ;
#6623 = DIRECTION ( 'NONE',  ( -0.000000000000000000, 0.000000000000000000, 1.000000000000000000 ) ) ;
#6624 = CARTESIAN_POINT ( 'NONE',  ( -0.8182917201112819283, 3.267716535433071279, -1.299212598425193210 ) ) ;
#6625 = DIRECTION ( 'NONE',  ( 0.5773502691896260641, 0.5773502691896273964, 0.5773502691896240657 ) ) ;
#6626 = DIRECTION ( 'NONE',  ( -0.01601477604151182663, 0.9998717552508123996, -0.000000000000000000 ) ) ;
#6627 = VERTEX_POINT ( 'NONE', #35262 ) ;
#6628 = CARTESIAN_POINT ( 'NONE',  ( -2.928234748147720445, 1.673608555435994516, 0.3801023473834607147 ) ) ;
#6629 = CARTESIAN_POINT ( 'NONE',  ( -0.2727639067037602172, 3.346456692913386100, 1.732283464566921172 ) ) ;
#6630 = ORIENTED_EDGE ( 'NONE', *, *, #197, .T. ) ;
#6631 = FACE_OUTER_BOUND ( 'NONE', #10807, .T. ) ;
#6632 = VERTEX_POINT ( 'NONE', #35512 ) ;
#6633 = ORIENTED_EDGE ( 'NONE', *, *, #47490, .T. ) ;
#6634 = EDGE_CURVE ( 'NONE', #11355, #15591, #31641, .T. ) ;
#6635 = VECTOR ( 'NONE', #47621, 39.37007874015748143 ) ;
#6636 = ADVANCED_FACE ( 'NONE', ( #23125 ), #22879, .F. ) ;
#6637 = VECTOR ( 'NONE', #49326, 39.37007874015748143 ) ;
#6638 = ORIENTED_EDGE ( 'NONE', *, *, #43768, .F. ) ;
#6639 = ORIENTED_EDGE ( 'NONE', *, *, #29980, .T. ) ;
#6640 = DIRECTION ( 'NONE',  ( 1.734723475976806848E-16, -0.000000000000000000, 1.000000000000000000 ) ) ;
#6641 = ADVANCED_FACE ( 'NONE', ( #15635 ), #34753, .F. ) ;
#6642 = EDGE_CURVE ( 'NONE', #30226, #448, #16148, .T. ) ;
#6643 = ORIENTED_EDGE ( 'NONE', *, *, #50223, .F. ) ;
#6644 = VECTOR ( 'NONE', #45387, 39.37007874015748143 ) ;
#6645 = PLANE ( 'NONE',  #34508 ) ;
#6646 = DIRECTION ( 'NONE',  ( 1.734723475976806848E-16, 0.000000000000000000, 1.000000000000000000 ) ) ;
#6647 = FACE_OUTER_BOUND ( 'NONE', #37327, .T. ) ;
#6648 = CARTESIAN_POINT ( 'NONE',  ( 1.472219874544873131, 1.643743200001983151, 2.560030851058970214 ) ) ;
#6649 = FACE_OUTER_BOUND ( 'NONE', #25581, .T. ) ;
#6650 = ORIENTED_EDGE ( 'NONE', *, *, #25617, .F. ) ;
#6651 = CARTESIAN_POINT ( 'NONE',  ( 0.4521076751547876138, 1.616718085813380945, 2.215705648545971407 ) ) ;
#6652 = DIRECTION ( 'NONE',  ( -1.000000000000000000, -0.000000000000000000, -0.000000000000000000 ) ) ;
#6653 = CARTESIAN_POINT ( 'NONE',  ( 1.574803149606300190, 1.172985819482486924, 1.181102362204724532 ) ) ;
#6654 = CARTESIAN_POINT ( 'NONE',  ( 1.287906020515830141, 0.000000000000000000, 0.9448818897637746295 ) ) ;
#6655 = ORIENTED_EDGE ( 'NONE', *, *, #3257, .F. ) ;
#6656 = CARTESIAN_POINT ( 'NONE',  ( 1.588513588560381828, 0.05336261777518135074, -1.107536019441389019 ) ) ;
#6657 = CARTESIAN_POINT ( 'NONE',  ( -0.3486774197067334380, 3.346456692913386100, 1.574803149606291974 ) ) ;
#6658 = ORIENTED_EDGE ( 'NONE', *, *, #3867, .F. ) ;
#6659 = DIRECTION ( 'NONE',  ( 1.000000000000000000, 0.000000000000000000, -3.469446951953613696E-16 ) ) ;
#6660 = DIRECTION ( 'NONE',  ( 0.000000000000000000, -1.000000000000000000, 0.000000000000000000 ) ) ;
#6661 = VERTEX_POINT ( 'NONE', #43748 ) ;
#6662 = LINE ( 'NONE', #46129, #31506 ) ;
#6663 = ORIENTED_EDGE ( 'NONE', *, *, #41226, .F. ) ;
#6664 = DIRECTION ( 'NONE',  ( 0.01601477604151182663, -0.9998717552508123996, 0.000000000000000000 ) ) ;
#6665 = DIRECTION ( 'NONE',  ( -0.000000000000000000, 1.000000000000000000, -0.000000000000000000 ) ) ;
#6666 = VECTOR ( 'NONE', #6143, 39.37007874015748143 ) ;
#6667 = DIRECTION ( 'NONE',  ( -0.000000000000000000, 0.000000000000000000, 1.000000000000000000 ) ) ;
#6668 = AXIS2_PLACEMENT_3D ( 'NONE', #36900, #11041, #50227 ) ;
#6669 = LINE ( 'NONE', #2034, #36674 ) ;
#6670 = DIRECTION ( 'NONE',  ( 1.000000000000000000, 0.000000000000000000, -3.469446951953613696E-16 ) ) ;
#6671 = ORIENTED_EDGE ( 'NONE', *, *, #8530, .T. ) ;
#6672 = FACE_OUTER_BOUND ( 'NONE', #1321, .T. ) ;
#6673 = EDGE_CURVE ( 'NONE', #40629, #47658, #38634, .T. ) ;
#6674 = ORIENTED_EDGE ( 'NONE', *, *, #28625, .F. ) ;
#6675 = ORIENTED_EDGE ( 'NONE', *, *, #43250, .F. ) ;
#6676 = ADVANCED_FACE ( 'NONE', ( #50436 ), #30883, .F. ) ;
#6677 = DIRECTION ( 'NONE',  ( -3.469446951953613696E-16, 0.000000000000000000, -1.000000000000000000 ) ) ;
#6678 = ORIENTED_EDGE ( 'NONE', *, *, #44605, .T. ) ;
#6679 = DIRECTION ( 'NONE',  ( 0.3513748240813304724, 0.000000000000000000, 0.9362348706397417564 ) ) ;
#6680 = VECTOR ( 'NONE', #39121, 39.37007874015748143 ) ;
#6681 = CARTESIAN_POINT ( 'NONE',  ( -1.363819533518803029, 0.000000000000000000, 0.2755905511810996522 ) ) ;
#6682 = ORIENTED_EDGE ( 'NONE', *, *, #21479, .F. ) ;
#6683 = EDGE_CURVE ( 'NONE', #35776, #46240, #12525, .T. ) ;
#6684 = FACE_OUTER_BOUND ( 'NONE', #23916, .T. ) ;
#6685 = CARTESIAN_POINT ( 'NONE',  ( -0.3486774197067339376, 3.346456692913386100, 2.137096964226333107 ) ) ;
#6686 = ADVANCED_FACE ( 'NONE', ( #24916 ), #32162, .F. ) ;
#6687 = DIRECTION ( 'NONE',  ( -0.000000000000000000, 0.000000000000000000, 1.000000000000000000 ) ) ;
#6688 = ORIENTED_EDGE ( 'NONE', *, *, #34875, .T. ) ;
#6689 = EDGE_LOOP ( 'NONE', ( #4598, #3449, #43877, #45964 ) ) ;
#6690 = DIRECTION ( 'NONE',  ( 1.734723475976806848E-16, -0.000000000000000000, 1.000000000000000000 ) ) ;
#6691 = FACE_BOUND ( 'NONE', #50479, .T. ) ;
#6692 = ORIENTED_EDGE ( 'NONE', *, *, #30725, .F. ) ;
#6693 = LINE ( 'NONE', #22442, #24568 ) ;
#6694 = EDGE_CURVE ( 'NONE', #50136, #4308, #5549, .T. ) ;
#6695 = CARTESIAN_POINT ( 'NONE',  ( -1.636583440222563857, 3.267716535433071279, 2.839019714148966584E-16 ) ) ;
#6696 = ORIENTED_EDGE ( 'NONE', *, *, #46603, .T. ) ;
#6697 = ORIENTED_EDGE ( 'NONE', *, *, #22634, .F. ) ;
#6698 = CARTESIAN_POINT ( 'NONE',  ( -0.2727639067037602172, 0.000000000000000000, 0.7874015748031456541 ) ) ;
#6699 = CARTESIAN_POINT ( 'NONE',  ( 0.000000000000000000, 0.000000000000000000, 0.000000000000000000 ) ) ;
#6700 = ADVANCED_FACE ( 'NONE', ( #48364 ), #31464, .T. ) ;
#6701 = VERTEX_POINT ( 'NONE', #40925 ) ;
#6702 = ORIENTED_EDGE ( 'NONE', *, *, #13344, .T. ) ;
#6703 = VERTEX_POINT ( 'NONE', #36544 ) ;
#6704 = DIRECTION ( 'NONE',  ( -3.469446951953613696E-16, 0.000000000000000000, -1.000000000000000000 ) ) ;
#6705 = VECTOR ( 'NONE', #43010, 39.37007874015748143 ) ;
#6706 = PLANE ( 'NONE',  #24179 ) ;
#6707 = AXIS2_PLACEMENT_3D ( 'NONE', #36087, #42353, #27810 ) ;
#6708 = FACE_OUTER_BOUND ( 'NONE', #18918, .T. ) ;
#6709 = ORIENTED_EDGE ( 'NONE', *, *, #15651, .T. ) ;
#6710 = ORIENTED_EDGE ( 'NONE', *, *, #48426, .F. ) ;
#6711 = DIRECTION ( 'NONE',  ( 1.000000000000000000, 0.000000000000000000, 0.000000000000000000 ) ) ;
#6712 = CARTESIAN_POINT ( 'NONE',  ( -0.07591351300297333182, 0.000000000000000000, -1.102362204724405714 ) ) ;
#6713 = LINE ( 'NONE', #45667, #6046 ) ;
#6714 = AXIS2_PLACEMENT_3D ( 'NONE', #26362, #14234, #6500 ) ;
#6715 = ADVANCED_FACE ( 'NONE', ( #29032 ), #27318, .T. ) ;
#6716 = CARTESIAN_POINT ( 'NONE',  ( 1.662320194739497659, 0.000000000000000000, -1.388601395075552025 ) ) ;
#6717 = DIRECTION ( 'NONE',  ( -1.000000000000000000, 0.000000000000000000, 1.734723475976806848E-16 ) ) ;
#6718 = VECTOR ( 'NONE', #26273, 39.37007874015748143 ) ;
#6719 = CARTESIAN_POINT ( 'NONE',  ( 0.1067246931122726866, 0.02962905676920215767, 0.000000000000000000 ) ) ;
#6720 = DIRECTION ( 'NONE',  ( 0.000000000000000000, -1.000000000000000000, 0.000000000000000000 ) ) ;
#6721 = ORIENTED_EDGE ( 'NONE', *, *, #26758, .F. ) ;
#6722 = DIRECTION ( 'NONE',  ( -0.8345732537212999791, 6.397775707690033618E-17, -0.5508969814521065267 ) ) ;
#6723 = LINE ( 'NONE', #45678, #45848 ) ;
#6724 = ORIENTED_EDGE ( 'NONE', *, *, #7443, .F. ) ;
#6725 = ORIENTED_EDGE ( 'NONE', *, *, #24426, .T. ) ;
#6726 = CARTESIAN_POINT ( 'NONE',  ( 1.015142113812069979, 0.000000000000000000, 2.047244094488179567 ) ) ;
#6727 = CARTESIAN_POINT ( 'NONE',  ( 1.363819533518803029, 0.000000000000000000, -1.732283464566923170 ) ) ;
#6728 = VERTEX_POINT ( 'NONE', #29291 ) ;
#6729 = B_SPLINE_CURVE_WITH_KNOTS ( 'NONE', 3,
 ( #31992, #28091, #43838, #8489 ),
 .UNSPECIFIED., .F., .F.,
 ( 4, 4 ),
 ( 6.402262811813191204E-07, 0.003597790540659576587 ),
 .UNSPECIFIED. ) ;
#6730 = EDGE_CURVE ( 'NONE', #29593, #44975, #44771, .T. ) ;
#6731 = ORIENTED_EDGE ( 'NONE', *, *, #7911, .F. ) ;
#6732 = CARTESIAN_POINT ( 'NONE',  ( 0.2727639067037604947, 3.346456692913386100, -1.102362204724405714 ) ) ;
#6733 = ORIENTED_EDGE ( 'NONE', *, *, #3050, .T. ) ;
#6734 = ADVANCED_FACE ( 'NONE', ( #20532 ), #44523, .F. ) ;
#6735 = VECTOR ( 'NONE', #41391, 39.37007874015748143 ) ;
#6736 = DIRECTION ( 'NONE',  ( -0.2225209339563041788, 1.288287287306305283E-16, -0.9749279121818259508 ) ) ;
#6737 = FACE_OUTER_BOUND ( 'NONE', #17726, .T. ) ;
#6738 = VECTOR ( 'NONE', #20784, 39.37007874015748143 ) ;
#6739 = EDGE_CURVE ( 'NONE', #5130, #47474, #8402, .T. ) ;
#6740 = EDGE_CURVE ( 'NONE', #11491, #45764, #24149, .T. ) ;
#6741 = ORIENTED_EDGE ( 'NONE', *, *, #36496, .F. ) ;
#6742 = VECTOR ( 'NONE', #18549, 39.37007874015748143 ) ;
#6743 = DIRECTION ( 'NONE',  ( -0.000000000000000000, 1.000000000000000000, -0.000000000000000000 ) ) ;
#6744 = ORIENTED_EDGE ( 'NONE', *, *, #30060, .T. ) ;
#6745 = VERTEX_POINT ( 'NONE', #13302 ) ;
#6746 = DIRECTION ( 'NONE',  ( 0.9909497617679331460, 0.000000000000000000, 0.1342332658176667026 ) ) ;
#6747 = CARTESIAN_POINT ( 'NONE',  ( -2.182111253630085290, 3.346456692913386100, -0.1968503937007880511 ) ) ;
#6748 = CARTESIAN_POINT ( 'NONE',  ( -1.735586374879336535, 0.000000000000000000, -2.388829707800051327 ) ) ;
#6749 = CARTESIAN_POINT ( 'NONE',  ( 0.8114156045248139826, 0.01345147374945592292, -1.798345332367593974 ) ) ;
#6750 = AXIS2_PLACEMENT_3D ( 'NONE', #27215, #19966, #20228 ) ;
#6751 = ORIENTED_EDGE ( 'NONE', *, *, #10988, .T. ) ;
#6752 = LINE ( 'NONE', #42358, #25380 ) ;
#6753 = ADVANCED_FACE ( 'NONE', ( #39894 ), #20268, .T. ) ;
#6754 = CARTESIAN_POINT ( 'NONE',  ( 1.905671854841463952, 1.748959039950288341, 2.256015092822681645 ) ) ;
#6755 = LINE ( 'NONE', #6247, #28648 ) ;
#6756 = VERTEX_POINT ( 'NONE', #28522 ) ;
#6757 = LINE ( 'NONE', #21743, #14178 ) ;
#6758 = EDGE_CURVE ( 'NONE', #39701, #12754, #32419, .T. ) ;
#6759 = EDGE_LOOP ( 'NONE', ( #22888, #43957, #47969, #26195, #16612, #31945, #46156, #38805, #16354, #33640, #19704, #49541, #40406 ) ) ;
#6760 = VERTEX_POINT ( 'NONE', #32943 ) ;
#6761 = CARTESIAN_POINT ( 'NONE',  ( 1.152895553066221046, 5.905511811023623991, -1.833672301139072092 ) ) ;
#6762 = EDGE_CURVE ( 'NONE', #35582, #41056, #10020, .T. ) ;
#6763 = CARTESIAN_POINT ( 'NONE',  ( -1.598711713507984022, 1.574803149606302854, -1.460438370699401522 ) ) ;
#6764 = CARTESIAN_POINT ( 'NONE',  ( 1.091055626815042645, 0.000000000000000000, -1.141732283464564013 ) ) ;
#6765 = ORIENTED_EDGE ( 'NONE', *, *, #11894, .T. ) ;
#6766 = ORIENTED_EDGE ( 'NONE', *, *, #29788, .F. ) ;
#6767 = CARTESIAN_POINT ( 'NONE',  ( -1.195183497228115035E-16, 0.000000000000000000, -1.574803149606293529 ) ) ;
#6768 = LINE ( 'NONE', #10890, #5342 ) ;
#6769 = VERTEX_POINT ( 'NONE', #12790 ) ;
#6770 = DIRECTION ( 'NONE',  ( -0.01601477604151182663, 0.9998717552508123996, -0.000000000000000000 ) ) ;
#6771 = EDGE_CURVE ( 'NONE', #20825, #22703, #9425, .T. ) ;
#6772 = LINE ( 'NONE', #45985, #6190 ) ;
#6773 = AXIS2_PLACEMENT_3D ( 'NONE', #31839, #27949, #39824 ) ;
#6774 = CARTESIAN_POINT ( 'NONE',  ( 1.491164160533713590, 0.9997502734738330510, -2.136136864276135139 ) ) ;
#6775 = DIRECTION ( 'NONE',  ( 1.000000000000000000, 0.000000000000000000, -3.469446951953613696E-16 ) ) ;
#6776 = CARTESIAN_POINT ( 'NONE',  ( -1.971247363764855320, 1.574803149606302854, -0.8960709840011922278 ) ) ;
#6777 = ORIENTED_EDGE ( 'NONE', *, *, #46551, .T. ) ;
#6778 = CARTESIAN_POINT ( 'NONE',  ( 1.287906020515829919, 3.346456692913386100, -1.740706023381844547 ) ) ;
#6779 = DIRECTION ( 'NONE',  ( 1.000000000000000000, 0.000000000000000000, -3.469446951953613696E-16 ) ) ;
#6780 = EDGE_CURVE ( 'NONE', #32449, #16395, #44273, .T. ) ;
#6781 = CONICAL_SURFACE ( 'NONE', #4306, 1.850107469027523210, 0.6386652850508578450 ) ;
#6782 = LINE ( 'NONE', #22526, #7583 ) ;
#6783 = EDGE_CURVE ( 'NONE', #2471, #9083, #21301, .T. ) ;
#6784 = ORIENTED_EDGE ( 'NONE', *, *, #27773, .F. ) ;
#6785 = VECTOR ( 'NONE', #28306, 39.37007874015748143 ) ;
#6786 = CARTESIAN_POINT ( 'NONE',  ( -0.2156685157583831947, 1.715903002249486997, -2.945280361644576850 ) ) ;
#6787 = CARTESIAN_POINT ( 'NONE',  ( 2.312967662867831287, 1.751800206377446267, -1.467809206421157864 ) ) ;
#6788 = CARTESIAN_POINT ( 'NONE',  ( 3.927031490892378253E-16, 3.267716535433071279, 2.007874015748021268 ) ) ;
#6789 = ORIENTED_EDGE ( 'NONE', *, *, #3984, .T. ) ;
#6790 = FACE_OUTER_BOUND ( 'NONE', #46621, .T. ) ;
#6791 = ORIENTED_EDGE ( 'NONE', *, *, #25745, .F. ) ;
#6792 = CARTESIAN_POINT ( 'NONE',  ( 0.000000000000000000, 2.755905511811023612, 0.000000000000000000 ) ) ;
#6793 = EDGE_LOOP ( 'NONE', ( #24498, #39832, #8666, #18929 ) ) ;
#6794 = DIRECTION ( 'NONE',  ( 0.01601477604151182663, -0.9998717552508123996, 0.000000000000000000 ) ) ;
#6795 = EDGE_CURVE ( 'NONE', #34431, #35644, #16920, .T. ) ;
#6796 = CARTESIAN_POINT ( 'NONE',  ( 0.5905511811023621549, 0.000000000000000000, -1.968503937007874072 ) ) ;
#6797 = PLANE ( 'NONE',  #14863 ) ;
#6798 = FACE_OUTER_BOUND ( 'NONE', #40928, .T. ) ;
#6799 = EDGE_CURVE ( 'NONE', #28822, #37178, #1676, .T. ) ;
#6800 = ORIENTED_EDGE ( 'NONE', *, *, #9588, .F. ) ;
#6801 = ORIENTED_EDGE ( 'NONE', *, *, #41999, .F. ) ;
#6802 = CARTESIAN_POINT ( 'NONE',  ( -1.066305685425808392, 3.256158526051301738, 2.204724409448808764 ) ) ;
#6803 = LINE ( 'NONE', #33684, #29622 ) ;
#6804 = ORIENTED_EDGE ( 'NONE', *, *, #4709, .T. ) ;
#6805 = CARTESIAN_POINT ( 'NONE',  ( 1.162932091021788183, 1.205361022782829114E-17, -1.684364178081092067 ) ) ;
#6806 = DIRECTION ( 'NONE',  ( 1.734723475976806848E-16, -0.000000000000000000, 1.000000000000000000 ) ) ;
#6807 = CARTESIAN_POINT ( 'NONE',  ( 1.636583440222563857, 3.267716535433071279, -0.3149606299212596716 ) ) ;
#6808 = B_SPLINE_CURVE_WITH_KNOTS ( 'NONE', 3,
 ( #42577, #11838, #27075, #38959 ),
 .UNSPECIFIED., .F., .F.,
 ( 4, 4 ),
 ( 2.002016750735623173E-07, 0.002500200813382404130 ),
 .UNSPECIFIED. ) ;
#6809 = VERTEX_POINT ( 'NONE', #14058 ) ;
#6810 = VECTOR ( 'NONE', #33826, 39.37007874015748143 ) ;
#6811 = ORIENTED_EDGE ( 'NONE', *, *, #13364, .T. ) ;
#6812 = PLANE ( 'NONE',  #22190 ) ;
#6813 = CARTESIAN_POINT ( 'NONE',  ( -0.8952071785065484066, 0.000000000000000000, 1.972340328593134906 ) ) ;
#6814 = DIRECTION ( 'NONE',  ( 0.000000000000000000, 0.000000000000000000, -1.000000000000000000 ) ) ;
#6815 = EDGE_CURVE ( 'NONE', #7509, #18296, #26432, .T. ) ;
#6816 = ORIENTED_EDGE ( 'NONE', *, *, #18990, .F. ) ;
#6817 = CARTESIAN_POINT ( 'NONE',  ( 3.937007874015748143, 5.118110236220475784, -1.181102362204724310 ) ) ;
#6818 = VECTOR ( 'NONE', #18242, 39.37007874015748143 ) ;
#6819 = DIRECTION ( 'NONE',  ( 0.9998717552508121775, 0.01601477604151182663, 0.000000000000000000 ) ) ;
#6820 = EDGE_LOOP ( 'NONE', ( #44127, #604, #8431, #6766 ) ) ;
#6821 = CARTESIAN_POINT ( 'NONE',  ( 0.5455278134075211005, 3.346456692913386100, -0.5118110236220467790 ) ) ;
#6822 = ORIENTED_EDGE ( 'NONE', *, *, #2755, .F. ) ;
#6823 = VECTOR ( 'NONE', #46780, 39.37007874015748143 ) ;
#6824 = VERTEX_POINT ( 'NONE', #38326 ) ;
#6825 = CARTESIAN_POINT ( 'NONE',  ( 0.2510238314733705400, 1.613497360050089036, -2.240096307734528835 ) ) ;
#6826 = CARTESIAN_POINT ( 'NONE',  ( 0.1155636338427008941, -0.5222242541845523167, 0.000000000000000000 ) ) ;
#6827 = VECTOR ( 'NONE', #42634, 39.37007874015748143 ) ;
#6828 = VECTOR ( 'NONE', #13699, 39.37007874015748143 ) ;
#6829 = CARTESIAN_POINT ( 'NONE',  ( 0.9794755770252100424, 0.5070346321433213399, -1.025452293874514087 ) ) ;
#6830 = ADVANCED_FACE ( 'NONE', ( #30062 ), #14308, .F. ) ;
#6831 = CARTESIAN_POINT ( 'NONE',  ( -1.325491792074585451, 1.600165750963108646, -2.638988599164751481 ) ) ;
#6832 = CARTESIAN_POINT ( 'NONE',  ( -0.5455278134075214336, 0.000000000000000000, -0.3149606299212593941 ) ) ;
#6833 = VERTEX_POINT ( 'NONE', #41680 ) ;
#6834 = EDGE_LOOP ( 'NONE', ( #37257, #31467, #21374, #3303 ) ) ;
#6835 = CARTESIAN_POINT ( 'NONE',  ( 0.7423782071083092626, 3.346456692913386100, 1.574803149606291974 ) ) ;
#6836 = EDGE_CURVE ( 'NONE', #29967, #22951, #45520, .T. ) ;
#6837 = DIRECTION ( 'NONE',  ( -1.000000000000000000, 0.000000000000000000, 0.000000000000000000 ) ) ;
#6838 = EDGE_CURVE ( 'NONE', #35113, #33474, #45272, .T. ) ;
#6839 = EDGE_CURVE ( 'NONE', #35448, #23722, #49383, .T. ) ;
#6840 = DIRECTION ( 'NONE',  ( 0.000000000000000000, 1.000000000000000000, 0.000000000000000000 ) ) ;
#6841 = DIRECTION ( 'NONE',  ( -3.469446951953613696E-16, 0.000000000000000000, -1.000000000000000000 ) ) ;
#6842 = CARTESIAN_POINT ( 'NONE',  ( -0.8182917201112821504, 3.267716535433071279, 1.940849049717691344 ) ) ;
#6843 = VERTEX_POINT ( 'NONE', #1931 ) ;
#6844 = LINE ( 'NONE', #15096, #12644 ) ;
#6845 = EDGE_CURVE ( 'NONE', #50043, #16378, #13811, .T. ) ;
#6846 = CARTESIAN_POINT ( 'NONE',  ( 1.883714906751835061, 0.5249316497054297148, -0.03533553182421467903 ) ) ;
#6847 = ORIENTED_EDGE ( 'NONE', *, *, #4878, .F. ) ;
#6848 = CARTESIAN_POINT ( 'NONE',  ( 0.7381027496705279134, 5.905511811023624880, -2.859439394060913298 ) ) ;
#6849 = LINE ( 'NONE', #46314, #6374 ) ;
#6850 = ORIENTED_EDGE ( 'NONE', *, *, #2415, .F. ) ;
#6851 = FACE_OUTER_BOUND ( 'NONE', #47791, .T. ) ;
#6852 = CARTESIAN_POINT ( 'NONE',  ( 1.091055626815042645, 3.267716535433071279, -8.878505979408855953E-16 ) ) ;
#6853 = PLANE ( 'NONE',  #7875 ) ;
#6854 = VECTOR ( 'NONE', #13552, 39.37007874015748143 ) ;
#6855 = ORIENTED_EDGE ( 'NONE', *, *, #44442, .F. ) ;
#6856 = DIRECTION ( 'NONE',  ( 1.000000000000000000, 0.000000000000000000, -3.469446951953613696E-16 ) ) ;
#6857 = VERTEX_POINT ( 'NONE', #2943 ) ;
#6858 = FACE_BOUND ( 'NONE', #26318, .T. ) ;
#6859 = AXIS2_PLACEMENT_3D ( 'NONE', #26625, #23507, #23769 ) ;
#6860 = EDGE_CURVE ( 'NONE', #48901, #11981, #10185, .T. ) ;
#6861 = VECTOR ( 'NONE', #23717, 39.37007874015748143 ) ;
#6862 = CARTESIAN_POINT ( 'NONE',  ( 1.015142113812069313, 3.267716535433071279, -0.03937007874015881204 ) ) ;
#6863 = DIRECTION ( 'NONE',  ( 0.000000000000000000, -1.000000000000000000, 0.000000000000000000 ) ) ;
#6864 = EDGE_CURVE ( 'NONE', #7807, #15130, #15457, .T. ) ;
#6865 = VERTEX_POINT ( 'NONE', #22063 ) ;
#6866 = ORIENTED_EDGE ( 'NONE', *, *, #668, .F. ) ;
#6867 = LINE ( 'NONE', #6622, #24875 ) ;
#6868 = AXIS2_PLACEMENT_3D ( 'NONE', #16949, #28036, #24176 ) ;
#6869 = ADVANCED_FACE ( 'NONE', ( #18441 ), #26517, .F. ) ;
#6870 = FACE_OUTER_BOUND ( 'NONE', #25046, .T. ) ;
#6871 = DIRECTION ( 'NONE',  ( 0.000000000000000000, -1.000000000000000000, 0.000000000000000000 ) ) ;
#6872 = FACE_OUTER_BOUND ( 'NONE', #38956, .T. ) ;
#6873 = CARTESIAN_POINT ( 'NONE',  ( -0.7242357167440469645, 0.5244080516102115341, 2.069776435762439082 ) ) ;
#6874 = VERTEX_POINT ( 'NONE', #10442 ) ;
#6875 = EDGE_LOOP ( 'NONE', ( #2351, #25446, #5291, #25679 ) ) ;
#6876 = CARTESIAN_POINT ( 'NONE',  ( 0.7423782071083091516, 0.000000000000000000, 1.062992125984246083 ) ) ;
#6877 = CARTESIAN_POINT ( 'NONE',  ( -0.5455278134075214336, 0.000000000000000000, -1.889763779527552146 ) ) ;
#6878 = ORIENTED_EDGE ( 'NONE', *, *, #23808, .F. ) ;
#6879 = LINE ( 'NONE', #34260, #10099 ) ;
#6880 = EDGE_LOOP ( 'NONE', ( #22112, #8729, #15832, #47326 ) ) ;
#6881 = ORIENTED_EDGE ( 'NONE', *, *, #45196, .F. ) ;
#6882 = ORIENTED_EDGE ( 'NONE', *, *, #23382, .T. ) ;
#6883 = ORIENTED_EDGE ( 'NONE', *, *, #10077, .T. ) ;
#6884 = FACE_OUTER_BOUND ( 'NONE', #6450, .T. ) ;
#6885 = VECTOR ( 'NONE', #15751, 39.37007874015748143 ) ;
#6886 = AXIS2_PLACEMENT_3D ( 'NONE', #3736, #31109, #22600 ) ;
#6887 = CARTESIAN_POINT ( 'NONE',  ( -2.803168555509503168, 1.577132182987436071, 0.9280531159812355213 ) ) ;
#6888 = CARTESIAN_POINT ( 'NONE',  ( -0.8942052331142552601, 3.346456692913386100, -0.8267716535433052849 ) ) ;
#6889 = AXIS2_PLACEMENT_3D ( 'NONE', #50513, #39460, #15206 ) ;
#6890 = VECTOR ( 'NONE', #40623, 39.37007874015748143 ) ;
#6891 = ADVANCED_FACE ( 'NONE', ( #25932 ), #49130, .T. ) ;
#6892 = EDGE_CURVE ( 'NONE', #15453, #13805, #6054, .T. ) ;
#6893 = CARTESIAN_POINT ( 'NONE',  ( 2.426524993341469649, 0.9874350405758482996, -0.9836271300236743009 ) ) ;
#6894 = EDGE_CURVE ( 'NONE', #26463, #12576, #17934, .T. ) ;
#6895 = MANIFOLD_SOLID_BREP ( 'Extrude-Thin1', #2356 ) ;
#6896 = CARTESIAN_POINT ( 'NONE',  ( 0.8182917201112817063, 3.346456692913386100, -1.417322834645664331 ) ) ;
#6897 = CARTESIAN_POINT ( 'NONE',  ( 1.723188456408574432, 1.574803149606302854, 1.311251662046225785 ) ) ;
#6898 = AXIS2_PLACEMENT_3D ( 'NONE', #37779, #6014, #13515 ) ;
#6899 = ORIENTED_EDGE ( 'NONE', *, *, #21441, .F. ) ;
#6900 = DIRECTION ( 'NONE',  ( 0.000000000000000000, 0.000000000000000000, 1.000000000000000000 ) ) ;
#6901 = DIRECTION ( 'NONE',  ( 0.000000000000000000, -1.000000000000000000, 0.000000000000000000 ) ) ;
#6902 = CARTESIAN_POINT ( 'NONE',  ( 1.835231397189315938, 1.704488142544798857, 1.400602925730996651 ) ) ;
#6903 = CARTESIAN_POINT ( 'NONE',  ( -1.692470051079808302, 0.0002787164204499768426, -0.4367734368499223141 ) ) ;
#6904 = ORIENTED_EDGE ( 'NONE', *, *, #1497, .T. ) ;
#6905 = LINE ( 'NONE', #42022, #44613 ) ;
#6906 = DIRECTION ( 'NONE',  ( 1.000000000000000000, 0.000000000000000000, 0.000000000000000000 ) ) ;
#6907 = ORIENTED_EDGE ( 'NONE', *, *, #46295, .F. ) ;
#6908 = LINE ( 'NONE', #25765, #9778 ) ;
#6909 = LINE ( 'NONE', #29388, #25954 ) ;
#6910 = ORIENTED_EDGE ( 'NONE', *, *, #35600, .F. ) ;
#6911 = LINE ( 'NONE', #42531, #16677 ) ;
#6912 = EDGE_CURVE ( 'NONE', #17493, #7739, #49629, .T. ) ;
#6913 = ORIENTED_EDGE ( 'NONE', *, *, #49537, .T. ) ;
#6914 = LINE ( 'NONE', #22665, #5004 ) ;
#6915 = CARTESIAN_POINT ( 'NONE',  ( -1.547114303032252502, 1.584696887024839906, -1.547279266820049237 ) ) ;
#6916 = PLANE ( 'NONE',  #20430 ) ;
#6917 = EDGE_CURVE ( 'NONE', #31200, #5130, #26683, .T. ) ;
#6918 = LINE ( 'NONE', #39169, #11093 ) ;
#6919 = DIRECTION ( 'NONE',  ( 0.000000000000000000, 0.000000000000000000, -1.000000000000000000 ) ) ;
#6920 = ORIENTED_EDGE ( 'NONE', *, *, #24494, .T. ) ;
#6921 = B_SPLINE_CURVE_WITH_KNOTS ( 'NONE', 3,
 ( #45510, #34186, #26175, #46023 ),
 .UNSPECIFIED., .F., .F.,
 ( 4, 4 ),
 ( 2.219923521421416046E-07, 0.01892337025898207375 ),
 .UNSPECIFIED. ) ;
#6922 = EDGE_CURVE ( 'NONE', #37613, #49793, #11198, .T. ) ;
#6923 = CARTESIAN_POINT ( 'NONE',  ( 0.8182917201112819283, 3.346456692913386100, -0.7874015748031473194 ) ) ;
#6924 = VECTOR ( 'NONE', #43243, 39.37007874015748143 ) ;
#6925 = ORIENTED_EDGE ( 'NONE', *, *, #36655, .F. ) ;
#6926 = VERTEX_POINT ( 'NONE', #19183 ) ;
#6927 = AXIS2_PLACEMENT_3D ( 'NONE', #41562, #34081, #49767 ) ;
#6928 = PLANE ( 'NONE',  #45986 ) ;
#6929 = EDGE_CURVE ( 'NONE', #9666, #34518, #27186, .T. ) ;
#6930 = ORIENTED_EDGE ( 'NONE', *, *, #3561, .T. ) ;
#6931 = CARTESIAN_POINT ( 'NONE',  ( -6.488138984952753334E-17, 3.267716535433071279, 1.125512701259787342E-32 ) ) ;
#6932 = VECTOR ( 'NONE', #2539, 39.37007874015748143 ) ;
#6933 = CARTESIAN_POINT ( 'NONE',  ( -0.5455278134075214336, 3.267716535433071279, 0.1181102362204703021 ) ) ;
#6934 = ORIENTED_EDGE ( 'NONE', *, *, #48301, .T. ) ;
#6935 = VECTOR ( 'NONE', #18914, 39.37007874015748143 ) ;
#6936 = CIRCLE ( 'NONE', #25065, 2.106299212598425008 ) ;
#6937 = PLANE ( 'NONE',  #14892 ) ;
#6938 = CARTESIAN_POINT ( 'NONE',  ( -1.008242766279392466, 0.5249316497054292707, 1.591564316631172815 ) ) ;
#6939 = AXIS2_PLACEMENT_3D ( 'NONE', #20941, #12948, #25071 ) ;
#6940 = DIRECTION ( 'NONE',  ( -0.000000000000000000, 1.000000000000000000, -0.000000000000000000 ) ) ;
#6941 = VERTEX_POINT ( 'NONE', #50379 ) ;
#6942 = ORIENTED_EDGE ( 'NONE', *, *, #42151, .T. ) ;
#6943 = DIRECTION ( 'NONE',  ( 1.734723475976806848E-16, 0.000000000000000000, 1.000000000000000000 ) ) ;
#6944 = FACE_BOUND ( 'NONE', #10930, .T. ) ;
#6945 = ORIENTED_EDGE ( 'NONE', *, *, #19650, .F. ) ;
#6946 = CARTESIAN_POINT ( 'NONE',  ( 1.149923681930125285, 1.049866565067837820, -1.666459638993234682 ) ) ;
#6947 = EDGE_LOOP ( 'NONE', ( #15864, #12976, #859, #33392 ) ) ;
#6948 = VERTEX_POINT ( 'NONE', #11696 ) ;
#6949 = LINE ( 'NONE', #38944, #29881 ) ;
#6950 = CARTESIAN_POINT ( 'NONE',  ( -1.572333874580302826, 1.588350329550590745, 1.874479074994480410 ) ) ;
#6951 = ORIENTED_EDGE ( 'NONE', *, *, #28234, .F. ) ;
#6952 = CARTESIAN_POINT ( 'NONE',  ( 1.062992125984251413, 0.5905511811023621549, -1.181102362204724754 ) ) ;
#6953 = ORIENTED_EDGE ( 'NONE', *, *, #14103, .F. ) ;
#6954 = CARTESIAN_POINT ( 'NONE',  ( 2.168245791271197209, 1.466194936398640181, -2.004968704497248400 ) ) ;
#6955 = DIRECTION ( 'NONE',  ( -0.000000000000000000, 1.000000000000000000, -0.000000000000000000 ) ) ;
#6956 = LINE ( 'NONE', #27069, #24762 ) ;
#6957 = EDGE_LOOP ( 'NONE', ( #2868, #29903, #20791, #36682 ) ) ;
#6958 = ORIENTED_EDGE ( 'NONE', *, *, #16939, .F. ) ;
#6959 = PRODUCT_DEFINITION_FORMATION_WITH_SPECIFIED_SOURCE ( 'ANY', '', #40108, .NOT_KNOWN. ) ;
#6960 = EDGE_CURVE ( 'NONE', #27704, #6577, #26512, .T. ) ;
#6961 = CARTESIAN_POINT ( 'NONE',  ( 0.2727639067037610499, 0.000000000000000000, 1.732283464566921172 ) ) ;
#6962 = DIRECTION ( 'NONE',  ( 9.964307797194585150E-17, -1.000000000000000000, 5.953396763000637613E-17 ) ) ;
#6963 = VECTOR ( 'NONE', #46548, 39.37007874015748854 ) ;
#6964 = ADVANCED_FACE ( 'NONE', ( #27688 ), #15577, .F. ) ;
#6965 = CARTESIAN_POINT ( 'NONE',  ( 2.464291103507799896, 5.905511811023623991, -1.626664315311302067 ) ) ;
#6966 = CONICAL_SURFACE ( 'NONE', #30888, 2.246510896728926010, 0.01601546068027819014 ) ;
#6967 = DIRECTION ( 'NONE',  ( 1.734723475976806848E-16, -0.000000000000000000, 1.000000000000000000 ) ) ;
#6968 = EDGE_CURVE ( 'NONE', #20663, #10224, #17498, .T. ) ;
#6969 = AXIS2_PLACEMENT_3D ( 'NONE', #12119, #32259, #48464 ) ;
#6970 = CARTESIAN_POINT ( 'NONE',  ( 0.1968503937007873017, 0.000000000000000000, 0.6299212598425161236 ) ) ;
#6971 = AXIS2_PLACEMENT_3D ( 'NONE', #48648, #36833, #13334 ) ;
#6972 = CARTESIAN_POINT ( 'NONE',  ( 1.909347346926324684, 0.000000000000000000, -0.4724409448818889246 ) ) ;
#6973 = DIRECTION ( 'NONE',  ( -0.000000000000000000, 1.000000000000000000, -0.000000000000000000 ) ) ;
#6974 = AXIS2_PLACEMENT_3D ( 'NONE', #12622, #4881, #13650 ) ;
#6975 = ORIENTED_EDGE ( 'NONE', *, *, #38343, .F. ) ;
#6976 = LINE ( 'NONE', #3347, #18479 ) ;
#6977 = FACE_OUTER_BOUND ( 'NONE', #23746, .T. ) ;
#6978 = ORIENTED_EDGE ( 'NONE', *, *, #22695, .T. ) ;
#6979 = ORIENTED_EDGE ( 'NONE', *, *, #23803, .T. ) ;
#6980 = CARTESIAN_POINT ( 'NONE',  ( -1.909347346926324462, 0.000000000000000000, 0.7874015748031456541 ) ) ;
#6981 = CARTESIAN_POINT ( 'NONE',  ( 1.909347346926324462, 3.346456692913386100, -0.7874015748031473194 ) ) ;
#6982 = EDGE_CURVE ( 'NONE', #29807, #3259, #15818, .T. ) ;
#6983 = EDGE_LOOP ( 'NONE', ( #44641, #14949, #36735, #17001 ) ) ;
#6984 = B_SPLINE_CURVE_WITH_KNOTS ( 'NONE', 3,
 ( #35730, #31870, #47565, #43713 ),
 .UNSPECIFIED., .F., .F.,
 ( 4, 4 ),
 ( 2.894122142360316399E-07, 0.01944866240183671519 ),
 .UNSPECIFIED. ) ;
#6985 = ADVANCED_FACE ( 'NONE', ( #42680 ), #15025, .T. ) ;
#6986 = EDGE_LOOP ( 'NONE', ( #5452, #45151, #28019, #35832 ) ) ;
#6987 = CARTESIAN_POINT ( 'NONE',  ( -1.862188077367287642, 3.267716535433071279, -0.9842519685039344823 ) ) ;
#6988 = ORIENTED_EDGE ( 'NONE', *, *, #26375, .F. ) ;
#6989 = CARTESIAN_POINT ( 'NONE',  ( -0.3382312733057317167, 5.905511811023623991, -2.139420919314969805 ) ) ;
#6990 = PLANE ( 'NONE',  #25542 ) ;
#6991 = VERTEX_POINT ( 'NONE', #35453 ) ;
#6992 = FACE_OUTER_BOUND ( 'NONE', #35517, .T. ) ;
#6993 = VECTOR ( 'NONE', #16033, 39.37007874015748143 ) ;
#6994 = ORIENTED_EDGE ( 'NONE', *, *, #28941, .F. ) ;
#6995 = ORIENTED_EDGE ( 'NONE', *, *, #8696, .T. ) ;
#6996 = AXIS2_PLACEMENT_3D ( 'NONE', #1572, #17326, #37206 ) ;
#6997 = CARTESIAN_POINT ( 'NONE',  ( -1.794796351285541602, 3.346456692913386100, -1.102362204724405492 ) ) ;
#6998 = CARTESIAN_POINT ( 'NONE',  ( -0.4788131938641533303, 1.613355999311305133, 2.914091152102185944 ) ) ;
#6999 = CARTESIAN_POINT ( 'NONE',  ( 1.091055626815043311, 3.346456692913386100, 1.574803149606291974 ) ) ;
#7000 = CARTESIAN_POINT ( 'NONE',  ( -1.909347346926324462, 0.000000000000000000, -0.1574803149606297248 ) ) ;
#7001 = AXIS2_PLACEMENT_3D ( 'NONE', #25214, #29601, #6362 ) ;
#7002 = ORIENTED_EDGE ( 'NONE', *, *, #28973, .T. ) ;
#7003 = LINE ( 'NONE', #19364, #9735 ) ;
#7004 = CARTESIAN_POINT ( 'NONE',  ( -1.712496953225537633, 3.267716535433071279, -0.6692913385826758654 ) ) ;
#7005 = CARTESIAN_POINT ( 'NONE',  ( 1.971834065208952769, 1.205361022782829114E-17, 0.8963217522330182430 ) ) ;
#7006 = EDGE_LOOP ( 'NONE', ( #44844, #29079, #46691, #47581 ) ) ;
#7007 = CARTESIAN_POINT ( 'NONE',  ( 0.04921259842519667277, 1.720031199985617265, 2.952755905511811108 ) ) ;
#7008 = VECTOR ( 'NONE', #36936, 39.37007874015748143 ) ;
#7009 = EDGE_LOOP ( 'NONE', ( #42719, #34929, #15640, #49501 ) ) ;
#7010 = EDGE_LOOP ( 'NONE', ( #25602, #38121, #49873, #20075 ) ) ;
#7011 = DIRECTION ( 'NONE',  ( -1.000000000000000000, -0.000000000000000000, -0.000000000000000000 ) ) ;
#7012 = DIRECTION ( 'NONE',  ( 0.000000000000000000, 0.000000000000000000, -1.000000000000000000 ) ) ;
#7013 = CARTESIAN_POINT ( 'NONE',  ( -1.363819533518803029, 0.000000000000000000, 1.417322834645662777 ) ) ;
#7014 = CARTESIAN_POINT ( 'NONE',  ( 1.833433833923351353, 3.267716535433071279, 0.4330708661417290162 ) ) ;
#7015 = EDGE_LOOP ( 'NONE', ( #26654, #6155, #42628, #37805, #28586, #48930, #21818, #46234, #39240, #4140, #20643, #36964, #43074 ) ) ;
#7016 = ORIENTED_EDGE ( 'NONE', *, *, #14202, .F. ) ;
#7017 = EDGE_CURVE ( 'NONE', #47774, #29685, #3702, .T. ) ;
#7018 =( NAMED_UNIT ( * ) SI_UNIT ( $, .STERADIAN. ) SOLID_ANGLE_UNIT ( ) );
#7019 = ADVANCED_FACE ( 'NONE', ( #39577 ), #3956, .T. ) ;
#7020 = CARTESIAN_POINT ( 'NONE',  ( -0.4478186997240815592, 0.006973536065449309831, -1.807618761453886558 ) ) ;
#7021 = ORIENTED_EDGE ( 'NONE', *, *, #24627, .T. ) ;
#7022 = CARTESIAN_POINT ( 'NONE',  ( -1.439733046521776361, 3.267716535433071279, 4.995077429881866871E-16 ) ) ;
#7023 = CARTESIAN_POINT ( 'NONE',  ( 2.009025172380753066, 0.000000000000000000, 0.7045170369349440520 ) ) ;
#7024 = ADVANCED_FACE ( 'NONE', ( #43435 ), #4206, .F. ) ;
#7025 = EDGE_CURVE ( 'NONE', #37496, #13662, #30568, .T. ) ;
#7026 = EDGE_CURVE ( 'NONE', #24792, #40146, #30829, .T. ) ;
#7027 = DIRECTION ( 'NONE',  ( 0.01601477604151182663, -0.9998717552508123996, 0.000000000000000000 ) ) ;
#7028 = FACE_OUTER_BOUND ( 'NONE', #15823, .T. ) ;
#7029 = CARTESIAN_POINT ( 'NONE',  ( 0.1067246931122726866, 0.02962905676920215767, 0.000000000000000000 ) ) ;
#7030 = ORIENTED_EDGE ( 'NONE', *, *, #16659, .F. ) ;
#7031 = VECTOR ( 'NONE', #2269, 39.37007874015748143 ) ;
#7032 = CARTESIAN_POINT ( 'NONE',  ( 0.000000000000000000, 0.5070346321433212289, 0.9794755770252101534 ) ) ;
#7033 = CARTESIAN_POINT ( 'NONE',  ( -0.8329809839909440017, 1.205361022782829114E-17, -2.833254665166566877 ) ) ;
#7034 = VECTOR ( 'NONE', #23239, 39.37007874015748143 ) ;
#7035 = CIRCLE ( 'NONE', #432, 2.244934639244525076 ) ;
#7036 = LINE ( 'NONE', #21945, #43011 ) ;
#7037 = VECTOR ( 'NONE', #14286, 39.37007874015748143 ) ;
#7038 = B_SPLINE_CURVE_WITH_KNOTS ( 'NONE', 3,
 ( #31978, #47673, #12350, #43823 ),
 .UNSPECIFIED., .F., .F.,
 ( 4, 4 ),
 ( 2.271256658651362855E-07, 0.002500295160485191577 ),
 .UNSPECIFIED. ) ;
#7039 = ORIENTED_EDGE ( 'NONE', *, *, #15683, .F. ) ;
#7040 = CARTESIAN_POINT ( 'NONE',  ( -2.258024766633058622, 3.267716535433071279, -0.1574803149606298636 ) ) ;
#7041 = CARTESIAN_POINT ( 'NONE',  ( -1.985260859929297794, 0.000000000000000000, -0.5118110236220464460 ) ) ;
#7042 = EDGE_CURVE ( 'NONE', #43305, #50744, #7074, .T. ) ;
#7043 = CARTESIAN_POINT ( 'NONE',  ( 0.000000000000000000, 3.267716535433071279, 0.000000000000000000 ) ) ;
#7044 = ORIENTED_EDGE ( 'NONE', *, *, #1185, .F. ) ;
#7045 = CARTESIAN_POINT ( 'NONE',  ( 1.287906020515829919, 3.346456692913386100, -1.574803149606294417 ) ) ;
#7046 = VECTOR ( 'NONE', #1141, 39.37007874015748143 ) ;
#7047 = EDGE_CURVE ( 'NONE', #16270, #20260, #12209, .T. ) ;
#7048 = ORIENTED_EDGE ( 'NONE', *, *, #23337, .T. ) ;
#7049 = LINE ( 'NONE', #38546, #1509 ) ;
#7050 = ORIENTED_EDGE ( 'NONE', *, *, #35108, .F. ) ;
#7051 = PLANE ( 'NONE',  #43493 ) ;
#7052 = VERTEX_POINT ( 'NONE', #43940 ) ;
#7053 = LINE ( 'NONE', #2669, #8697 ) ;
#7054 = CARTESIAN_POINT ( 'NONE',  ( 1.295932559131132811, 1.739450087534528233, -2.653223575501737486 ) ) ;
#7055 = DIRECTION ( 'NONE',  ( 1.000000000000000000, 0.000000000000000000, 0.000000000000000000 ) ) ;
#7056 = EDGE_CURVE ( 'NONE', #25849, #21432, #31495, .T. ) ;
#7057 = ORIENTED_EDGE ( 'NONE', *, *, #49747, .T. ) ;
#7058 = EDGE_LOOP ( 'NONE', ( #7366, #20579, #43241, #40992 ) ) ;
#7059 = ORIENTED_EDGE ( 'NONE', *, *, #1186, .F. ) ;
#7060 = CARTESIAN_POINT ( 'NONE',  ( 0.000000000000000000, 1.574803149606302854, 0.000000000000000000 ) ) ;
#7061 = CARTESIAN_POINT ( 'NONE',  ( -0.5455278134075214336, 3.346456692913386100, 2.204724409448808764 ) ) ;
#7062 = ORIENTED_EDGE ( 'NONE', *, *, #28196, .F. ) ;
#7063 = CARTESIAN_POINT ( 'NONE',  ( 1.247448100859587239, 0.000000000000000000, -1.633239539486209591 ) ) ;
#7064 = CARTESIAN_POINT ( 'NONE',  ( -2.491402175429631605, 1.680428061220146096, -1.585592796919542025 ) ) ;
#7065 = DIRECTION ( 'NONE',  ( 1.000000000000000000, 0.000000000000000000, 0.000000000000000000 ) ) ;
#7066 = ADVANCED_FACE ( 'NONE', ( #24852 ), #40087, .F. ) ;
#7067 = ADVANCED_BREP_SHAPE_REPRESENTATION ( '', ( #40963, #26741 ), #40758 ) ;
#7068 = ORIENTED_EDGE ( 'NONE', *, *, #15690, .F. ) ;
#7069 = ORIENTED_EDGE ( 'NONE', *, *, #26161, .F. ) ;
#7070 = LINE ( 'NONE', #46278, #29599 ) ;
#7071 = PLANE ( 'NONE',  #38192 ) ;
#7072 = DIRECTION ( 'NONE',  ( 0.6910626489868685329, -1.160734090543304907E-16, -0.7227948638273880011 ) ) ;
#7073 = ORIENTED_EDGE ( 'NONE', *, *, #26757, .F. ) ;
#7074 = LINE ( 'NONE', #36732, #10894 ) ;
#7075 = DIRECTION ( 'NONE',  ( -0.000000000000000000, 1.000000000000000000, -0.000000000000000000 ) ) ;
#7076 = VECTOR ( 'NONE', #15283, 39.37007874015748143 ) ;
#7077 = ORIENTED_EDGE ( 'NONE', *, *, #2709, .F. ) ;
#7078 = AXIS2_PLACEMENT_3D ( 'NONE', #29842, #16959, #28817 ) ;
#7079 = CARTESIAN_POINT ( 'NONE',  ( 1.560669927219590747, 3.346456692913386100, 1.102362204724403938 ) ) ;
#7080 = ORIENTED_EDGE ( 'NONE', *, *, #45335, .F. ) ;
#7081 = ORIENTED_EDGE ( 'NONE', *, *, #1497, .F. ) ;
#7082 = CARTESIAN_POINT ( 'NONE',  ( 1.628466770324754176, 1.733984826446373750, -1.625060189682509870 ) ) ;
#7083 = CARTESIAN_POINT ( 'NONE',  ( 1.181102362204724310, 0.4724409448818890911, -1.181102362204724754 ) ) ;
#7084 = VECTOR ( 'NONE', #5145, 39.37007874015748143 ) ;
#7085 = PLANE ( 'NONE',  #10757 ) ;
#7086 = CONICAL_SURFACE ( 'NONE', #26057, 2.246510896728926010, 0.01601546068027819014 ) ;
#7087 = DIRECTION ( 'NONE',  ( 0.000000000000000000, -1.000000000000000000, 0.000000000000000000 ) ) ;
#7088 = CARTESIAN_POINT ( 'NONE',  ( -0.6214413264104945434, 0.000000000000000000, -1.102362204724405492 ) ) ;
#7089 = EDGE_LOOP ( 'NONE', ( #19755, #48060, #18455, #49071 ) ) ;
#7090 = VECTOR ( 'NONE', #30040, 39.37007874015748143 ) ;
#7091 = PRODUCT_DEFINITION_SHAPE ( 'NONE', 'NONE',  #16821 ) ;
#7092 = EDGE_LOOP ( 'NONE', ( #9123, #240, #31636, #1467 ) ) ;
#7093 = CARTESIAN_POINT ( 'NONE',  ( -0.2727639067037608278, 3.267716535433071279, -0.9842519685039344823 ) ) ;
#7094 = CARTESIAN_POINT ( 'NONE',  ( -1.909347346926324462, 3.346456692913386100, -0.1574803149606297248 ) ) ;
#7095 = EDGE_CURVE ( 'NONE', #18320, #43157, #44203, .T. ) ;
#7096 = EDGE_CURVE ( 'NONE', #8220, #32363, #35963, .T. ) ;
#7097 = EDGE_CURVE ( 'NONE', #37613, #48933, #9355, .T. ) ;
#7098 = DIRECTION ( 'NONE',  ( -0.000000000000000000, 1.000000000000000000, -0.000000000000000000 ) ) ;
#7099 = DIRECTION ( 'NONE',  ( -0.000000000000000000, 1.000000000000000000, -0.000000000000000000 ) ) ;
#7100 = ORIENTED_EDGE ( 'NONE', *, *, #32168, .T. ) ;
#7101 = LINE ( 'NONE', #18723, #44809 ) ;
#7102 = DIRECTION ( 'NONE',  ( -0.000000000000000000, 0.000000000000000000, 1.000000000000000000 ) ) ;
#7103 = VERTEX_POINT ( 'NONE', #16858 ) ;
#7104 = LINE ( 'NONE', #45804, #26496 ) ;
#7105 = CARTESIAN_POINT ( 'NONE',  ( 2.378961647330872786, 0.000000000000000000, -1.161035397307311917E-15 ) ) ;
#7106 = CARTESIAN_POINT ( 'NONE',  ( -1.632855683316659867, 1.205361022782829114E-17, -0.6443965869051290207 ) ) ;
#7107 = AXIS2_PLACEMENT_3D ( 'NONE', #43704, #16622, #16103 ) ;
#7108 = CARTESIAN_POINT ( 'NONE',  ( 1.091055626815042645, 3.346456692913386100, -0.9448818897637765168 ) ) ;
#7109 = CARTESIAN_POINT ( 'NONE',  ( -0.2727639067037607723, 3.267716535433071279, 0.1574803149606283648 ) ) ;
#7110 = DIRECTION ( 'NONE',  ( -0.000000000000000000, 1.000000000000000000, -0.000000000000000000 ) ) ;
#7111 = AXIS2_PLACEMENT_3D ( 'NONE', #48935, #29625, #6384 ) ;
#7112 = VECTOR ( 'NONE', #20804, 39.37007874015748143 ) ;
#7113 = ORIENTED_EDGE ( 'NONE', *, *, #21562, .F. ) ;
#7114 = LINE ( 'NONE', #22606, #45271 ) ;
#7115 = EDGE_LOOP ( 'NONE', ( #27472, #33878, #3773, #18100 ) ) ;
#7116 = CARTESIAN_POINT ( 'NONE',  ( 0.000000000000000000, 3.267716535433071279, 0.000000000000000000 ) ) ;
#7117 = VECTOR ( 'NONE', #20452, 39.37007874015748143 ) ;
#7118 = FACE_OUTER_BOUND ( 'NONE', #6880, .T. ) ;
#7119 = CARTESIAN_POINT ( 'NONE',  ( 2.339241080213586343, 1.205361022782829114E-17, 1.802537235681917815 ) ) ;
#7120 = VECTOR ( 'NONE', #22256, 39.37007874015748143 ) ;
#7121 = EDGE_CURVE ( 'NONE', #9684, #43163, #4973, .T. ) ;
#7122 = AXIS2_PLACEMENT_3D ( 'NONE', #3815, #7936, #35317 ) ;
#7123 = ORIENTED_EDGE ( 'NONE', *, *, #15259, .T. ) ;
#7124 = ORIENTED_EDGE ( 'NONE', *, *, #20548, .T. ) ;
#7125 = CARTESIAN_POINT ( 'NONE',  ( 1.618143960770675349, 1.638891035385505290, 1.926912937609726484 ) ) ;
#7126 = CARTESIAN_POINT ( 'NONE',  ( -1.429001793884109528, 1.049866565877818125, -1.434352145260018974 ) ) ;
#7127 = LINE ( 'NONE', #34998, #25023 ) ;
#7128 = PLANE ( 'NONE',  #48269 ) ;
#7129 = CARTESIAN_POINT ( 'NONE',  ( -2.182111253630085290, 0.000000000000000000, -0.3149606299212589500 ) ) ;
#7130 = EDGE_CURVE ( 'NONE', #22332, #7807, #40705, .T. ) ;
#7131 = CARTESIAN_POINT ( 'NONE',  ( -2.793030215715272213, 5.905511811023623991, 0.9592557174602281966 ) ) ;
#7132 = ORIENTED_EDGE ( 'NONE', *, *, #15216, .F. ) ;
#7133 = DIRECTION ( 'NONE',  ( -0.01601477604151182663, 0.9998717552508123996, -0.000000000000000000 ) ) ;
#7134 = CARTESIAN_POINT ( 'NONE',  ( -0.3486774197067334380, 3.267716535433071279, 1.209717811016577106E-16 ) ) ;
#7135 = EDGE_CURVE ( 'NONE', #11168, #15727, #20977, .T. ) ;
#7136 = FACE_OUTER_BOUND ( 'NONE', #11307, .T. ) ;
#7137 = VERTEX_POINT ( 'NONE', #4463 ) ;
#7138 = EDGE_CURVE ( 'NONE', #21275, #43635, #32611, .T. ) ;
#7139 = FACE_OUTER_BOUND ( 'NONE', #3575, .T. ) ;
#7140 = ORIENTED_EDGE ( 'NONE', *, *, #48831, .F. ) ;
#7141 = ORIENTED_EDGE ( 'NONE', *, *, #7346, .T. ) ;
#7142 = ADVANCED_FACE ( 'NONE', ( #5222 ), #25108, .F. ) ;
#7143 = B_SPLINE_CURVE_WITH_KNOTS ( 'NONE', 3,
 ( #3843, #30458, #35338, #50268 ),
 .UNSPECIFIED., .F., .F.,
 ( 4, 4 ),
 ( 0.0002550707838865089627, 0.002755222585228180900 ),
 .UNSPECIFIED. ) ;
#7144 = VECTOR ( 'NONE', #42522, 39.37007874015748143 ) ;
#7145 = ORIENTED_EDGE ( 'NONE', *, *, #15216, .T. ) ;
#7146 = ORIENTED_EDGE ( 'NONE', *, *, #1847, .T. ) ;
#7147 = LINE ( 'NONE', #38390, #30215 ) ;
#7148 = AXIS2_PLACEMENT_3D ( 'NONE', #48190, #40492, #43581 ) ;
#7149 = VECTOR ( 'NONE', #24098, 39.37007874015748854 ) ;
#7150 = CARTESIAN_POINT ( 'NONE',  ( -1.439733046521777027, 0.000000000000000000, -1.771653543307080581 ) ) ;
#7151 = FACE_BOUND ( 'NONE', #40983, .T. ) ;
#7152 = EDGE_CURVE ( 'NONE', #29864, #43566, #48555, .T. ) ;
#7153 = VECTOR ( 'NONE', #10706, 39.37007874015748143 ) ;
#7154 = DIRECTION ( 'NONE',  ( 1.000000000000000000, 0.000000000000000000, 0.000000000000000000 ) ) ;
#7155 = ADVANCED_FACE ( 'NONE', ( #24081 ), #4721, .F. ) ;
#7156 = ADVANCED_FACE ( 'NONE', ( #16082 ), #47789, .T. ) ;
#7157 = VECTOR ( 'NONE', #4776, 39.37007874015748143 ) ;
#7158 = CARTESIAN_POINT ( 'NONE',  ( -0.5440951526915226433, 1.699187271209207983, -2.156468654116168171 ) ) ;
#7159 = CARTESIAN_POINT ( 'NONE',  ( 0.2727639067037604947, 3.346456692913386100, -1.417322834645664331 ) ) ;
#7160 = VERTEX_POINT ( 'NONE', #846 ) ;
#7161 = DIRECTION ( 'NONE',  ( 1.734723475976806848E-16, -0.000000000000000000, 1.000000000000000000 ) ) ;
#7162 = LINE ( 'NONE', #26765, #3609 ) ;
#7163 = CARTESIAN_POINT ( 'NONE',  ( -0.2052282226254269204, 0.000000000000000000, -1.731265419273310346 ) ) ;
#7164 = DIRECTION ( 'NONE',  ( 1.000000000000000000, 0.000000000000000000, -3.469446951953613696E-16 ) ) ;
#7165 = ORIENTED_EDGE ( 'NONE', *, *, #23474, .T. ) ;
#7166 = CARTESIAN_POINT ( 'NONE',  ( 4.268512490100411402E-16, 0.000000000000000000, 1.574803149606291974 ) ) ;
#7167 = LINE ( 'NONE', #15914, #8790 ) ;
#7168 = ORIENTED_EDGE ( 'NONE', *, *, #36072, .T. ) ;
#7169 = LINE ( 'NONE', #42524, #1556 ) ;
#7170 = PLANE ( 'NONE',  #11095 ) ;
#7171 = CARTESIAN_POINT ( 'NONE',  ( 0.000000000000000000, 3.267716535433071279, 1.220472440944875281 ) ) ;
#7172 = ORIENTED_EDGE ( 'NONE', *, *, #18048, .F. ) ;
#7173 = DIRECTION ( 'NONE',  ( -1.000000000000000000, 0.000000000000000000, -0.000000000000000000 ) ) ;
#7174 = FACE_OUTER_BOUND ( 'NONE', #47667, .T. ) ;
#7175 = DIRECTION ( 'NONE',  ( 8.741157232058135226E-17, -1.000000000000000000, 7.636919086868543885E-17 ) ) ;
#7176 = CARTESIAN_POINT ( 'NONE',  ( 1.062992125984251413, 0.4724409448818890911, -1.181102362204724754 ) ) ;
#7177 = CARTESIAN_POINT ( 'NONE',  ( 0.1968503937007872462, 0.000000000000000000, -1.771653543307081025 ) ) ;
#7178 = ORIENTED_EDGE ( 'NONE', *, *, #5811, .T. ) ;
#7179 = VECTOR ( 'NONE', #34228, 39.37007874015748143 ) ;
#7180 = EDGE_CURVE ( 'NONE', #45138, #46569, #40307, .T. ) ;
#7181 = DIRECTION ( 'NONE',  ( -0.000000000000000000, 1.000000000000000000, -0.000000000000000000 ) ) ;
#7182 = CONICAL_SURFACE ( 'NONE', #41787, 2.244934639244524632, 1.554780866114618743 ) ;
#7183 = VERTEX_POINT ( 'NONE', #12458 ) ;
#7184 = VERTEX_POINT ( 'NONE', #9869 ) ;
#7185 = LINE ( 'NONE', #50733, #13882 ) ;
#7186 = ORIENTED_EDGE ( 'NONE', *, *, #9271, .F. ) ;
#7187 = CARTESIAN_POINT ( 'NONE',  ( -2.623503965249869729, 1.569838463031876685, 1.355882097269834885 ) ) ;
#7188 = DIRECTION ( 'NONE',  ( 1.000000000000000000, 0.000000000000000000, 0.000000000000000000 ) ) ;
#7189 = VERTEX_POINT ( 'NONE', #41618 ) ;
#7190 = EDGE_CURVE ( 'NONE', #38704, #34644, #49320, .T. ) ;
#7191 = CARTESIAN_POINT ( 'NONE',  ( -2.100190309385016274, 0.000000000000000000, 0.5298329251847215815 ) ) ;
#7192 = EDGE_CURVE ( 'NONE', #9810, #48829, #6757, .T. ) ;
#7193 = VECTOR ( 'NONE', #6519, 39.37007874015748143 ) ;
#7194 = DIRECTION ( 'NONE',  ( 1.000000000000000000, -0.000000000000000000, 0.000000000000000000 ) ) ;
#7195 = EDGE_CURVE ( 'NONE', #49909, #50260, #13745, .T. ) ;
#7196 = ADVANCED_FACE ( 'NONE', ( #33380 ), #37501, .F. ) ;
#7197 = CARTESIAN_POINT ( 'NONE',  ( 0.9834642517162937025, 3.267716535433071279, -1.929133858267711110 ) ) ;
#7198 = EDGE_LOOP ( 'NONE', ( #50483, #28223, #29089, #4124 ) ) ;
#7199 = ORIENTED_EDGE ( 'NONE', *, *, #25766, .T. ) ;
#7200 = FACE_OUTER_BOUND ( 'NONE', #1337, .T. ) ;
#7201 = FACE_BOUND ( 'NONE', #14502, .T. ) ;
#7202 = VERTEX_POINT ( 'NONE', #2120 ) ;
#7203 = CARTESIAN_POINT ( 'NONE',  ( 0.9845150457423212931, 0.000000000000000000, -1.438794182654551390 ) ) ;
#7204 = ORIENTED_EDGE ( 'NONE', *, *, #21473, .F. ) ;
#7205 = ORIENTED_EDGE ( 'NONE', *, *, #15341, .F. ) ;
#7206 = B_SPLINE_CURVE_WITH_KNOTS ( 'NONE', 3,
 ( #34838, #43068, #19578, #35350 ),
 .UNSPECIFIED., .F., .F.,
 ( 4, 4 ),
 ( 0.0006178172717985424374, 0.04871068883268091926 ),
 .UNSPECIFIED. ) ;
#7207 = DIRECTION ( 'NONE',  ( -3.469446951953613696E-16, 0.000000000000000000, -1.000000000000000000 ) ) ;
#7208 = CARTESIAN_POINT ( 'NONE',  ( 0.000000000000000000, 3.267716535433071279, 1.850393700787392293 ) ) ;
#7209 = ORIENTED_EDGE ( 'NONE', *, *, #20895, .F. ) ;
#7210 = EDGE_CURVE ( 'NONE', #10793, #21434, #48803, .T. ) ;
#7211 = CARTESIAN_POINT ( 'NONE',  ( -2.454875160333845674, 3.223653470355286377, -0.2239369375554250974 ) ) ;
#7212 = ORIENTED_EDGE ( 'NONE', *, *, #20793, .T. ) ;
#7213 = LINE ( 'NONE', #18583, #32667 ) ;
#7214 = DIRECTION ( 'NONE',  ( -0.000000000000000000, 0.000000000000000000, 1.000000000000000000 ) ) ;
#7215 = EDGE_CURVE ( 'NONE', #46654, #16378, #5923, .T. ) ;
#7216 = VECTOR ( 'NONE', #1348, 39.37007874015748143 ) ;
#7217 = AXIS2_PLACEMENT_3D ( 'NONE', #19094, #34852, #50537 ) ;
#7218 = FACE_OUTER_BOUND ( 'NONE', #13221, .T. ) ;
#7219 = ADVANCED_FACE ( 'NONE', ( #6249 ), #33883, .F. ) ;
#7220 = EDGE_LOOP ( 'NONE', ( #26836, #26223, #27133, #40613 ) ) ;
#7221 = EDGE_LOOP ( 'NONE', ( #6696, #21794, #19276, #11106 ) ) ;
#7223 = DIRECTION ( 'NONE',  ( 0.000000000000000000, -1.000000000000000000, 0.000000000000000000 ) ) ;
#7222 = AXIS2_PLACEMENT_3D ( 'NONE', #26454, #3472, #38346 ) ;
#7224 = CARTESIAN_POINT ( 'NONE',  ( 1.560669927219590525, 3.346456692913386100, -0.9842519685039348154 ) ) ;
#7225 = EDGE_CURVE ( 'NONE', #37788, #45331, #985, .T. ) ;
#7226 = CARTESIAN_POINT ( 'NONE',  ( -1.062992125984251635, 0.5905511811023621549, 1.014069264286641570 ) ) ;
#7227 = CYLINDRICAL_SURFACE ( 'NONE', #35851, 1.181102362204723200 ) ;
#7228 = FACE_OUTER_BOUND ( 'NONE', #17541, .T. ) ;
#7229 = DIRECTION ( 'NONE',  ( 1.000000000000000000, 0.000000000000000000, 0.000000000000000000 ) ) ;
#7230 = CARTESIAN_POINT ( 'NONE',  ( -0.5455278134075214336, 3.267716535433071279, -1.574803149606293529 ) ) ;
#7231 = B_SPLINE_CURVE_WITH_KNOTS ( 'NONE', 3,
 ( #47584, #19487, #15624, #16132 ),
 .UNSPECIFIED., .F., .F.,
 ( 4, 4 ),
 ( 0.0003597596266483848982, 0.004912093308215493247 ),
 .UNSPECIFIED. ) ;
#7232 = ORIENTED_EDGE ( 'NONE', *, *, #32651, .F. ) ;
#7233 = CARTESIAN_POINT ( 'NONE',  ( -0.6214413264104938772, 3.267716535433071279, 2.156057715732898561E-16 ) ) ;
#7234 = CARTESIAN_POINT ( 'NONE',  ( -0.5455278134075214336, 3.346456692913386100, -1.259842519685035134 ) ) ;
#7235 = VECTOR ( 'NONE', #17197, 39.37007874015748143 ) ;
#7236 = EDGE_LOOP ( 'NONE', ( #46073, #26255, #2571, #47838 ) ) ;
#7237 = ORIENTED_EDGE ( 'NONE', *, *, #20051, .T. ) ;
#7238 = CARTESIAN_POINT ( 'NONE',  ( -2.437180031585919782, 1.582844051365913662, -1.667735833703134718 ) ) ;
#7239 = CARTESIAN_POINT ( 'NONE',  ( -3.346456692913385211, 0.000000000000000000, -4.133858267716536083 ) ) ;
#7240 = EDGE_LOOP ( 'NONE', ( #32311, #12957, #13491, #24534 ) ) ;
#7241 = VERTEX_POINT ( 'NONE', #6510 ) ;
#7242 = LINE ( 'NONE', #49542, #11377 ) ;
#7243 = VERTEX_POINT ( 'NONE', #1610 ) ;
#7244 = DIRECTION ( 'NONE',  ( 0.000000000000000000, 0.000000000000000000, -1.000000000000000000 ) ) ;
#7245 = CARTESIAN_POINT ( 'NONE',  ( 1.779568955232893268, 1.574803149606302854, -1.233650562797287797 ) ) ;
#7246 = ADVANCED_FACE ( 'NONE', ( #17364 ), #45966, .F. ) ;
#7247 = VECTOR ( 'NONE', #20242, 39.37007874015748854 ) ;
#7248 = VECTOR ( 'NONE', #48717, 39.37007874015748143 ) ;
#7249 = VERTEX_POINT ( 'NONE', #2379 ) ;
#7250 = ADVANCED_FACE ( 'NONE', ( #34127 ), #42218, .T. ) ;
#7251 = DIRECTION ( 'NONE',  ( 1.000000000000000000, 0.000000000000000000, 0.000000000000000000 ) ) ;
#7252 = ADVANCED_FACE ( 'NONE', ( #26120 ), #29993, .T. ) ;
#7253 = VERTEX_POINT ( 'NONE', #21487 ) ;
#7254 = ORIENTED_EDGE ( 'NONE', *, *, #39554, .T. ) ;
#7255 = CARTESIAN_POINT ( 'NONE',  ( 0.08139965876239094178, 1.610780518492231694, 0.000000000000000000 ) ) ;
#7256 = DIRECTION ( 'NONE',  ( -3.986037398843765983E-20, -1.000000000000000000, -1.160734090543304660E-16 ) ) ;
#7257 = DIRECTION ( 'NONE',  ( -0.000000000000000000, 0.000000000000000000, 1.000000000000000000 ) ) ;
#7258 = VECTOR ( 'NONE', #28901, 39.37007874015748143 ) ;
#7259 = ORIENTED_EDGE ( 'NONE', *, *, #19669, .F. ) ;
#7260 = PLANE ( 'NONE',  #30330 ) ;
#7261 = PLANE ( 'NONE',  #23347 ) ;
#7262 = ORIENTED_EDGE ( 'NONE', *, *, #33865, .T. ) ;
#7263 = VECTOR ( 'NONE', #20074, 39.37007874015748143 ) ;
#7264 = DIRECTION ( 'NONE',  ( -3.469446951953613696E-16, 0.000000000000000000, -1.000000000000000000 ) ) ;
#7265 = ORIENTED_EDGE ( 'NONE', *, *, #26128, .T. ) ;
#7266 = ORIENTED_EDGE ( 'NONE', *, *, #47229, .F. ) ;
#7267 = EDGE_CURVE ( 'NONE', #3143, #13018, #10633, .T. ) ;
#7268 =( LENGTH_UNIT ( ) NAMED_UNIT ( * ) SI_UNIT ( $, .METRE. ) );
#7269 = VECTOR ( 'NONE', #3405, 39.37007874015748143 ) ;
#7270 = ORIENTED_EDGE ( 'NONE', *, *, #39535, .T. ) ;
#7271 = CARTESIAN_POINT ( 'NONE',  ( 0.5455278134075211005, 3.267716535433071279, -1.456692913385822630 ) ) ;
#7272 = LINE ( 'NONE', #23014, #39836 ) ;
#7273 = ADVANCED_FACE ( 'NONE', ( #26371 ), #33124, .F. ) ;
#7274 = CARTESIAN_POINT ( 'NONE',  ( 2.074049943651431693, 2.755905511811027164, 0.6221544894624241318 ) ) ;
#7275 = DIRECTION ( 'NONE',  ( -3.986037398843765983E-20, -1.000000000000000000, -1.160734090543304660E-16 ) ) ;
#7276 = ORIENTED_EDGE ( 'NONE', *, *, #24575, .T. ) ;
#7277 = ORIENTED_EDGE ( 'NONE', *, *, #14972, .F. ) ;
#7278 = EDGE_CURVE ( 'NONE', #6632, #19367, #49819, .T. ) ;
#7279 = DIRECTION ( 'NONE',  ( 1.000000000000000000, 0.000000000000000000, -3.469446951953613696E-16 ) ) ;
#7280 = VERTEX_POINT ( 'NONE', #13487 ) ;
#7281 = LINE ( 'NONE', #22271, #1879 ) ;
#7282 = DIRECTION ( 'NONE',  ( 0.000000000000000000, 1.000000000000000000, 0.000000000000000000 ) ) ;
#7283 = VECTOR ( 'NONE', #34555, 39.37007874015748143 ) ;
#7284 = DIRECTION ( 'NONE',  ( -3.986037398843765983E-20, -1.000000000000000000, -1.160734090543304660E-16 ) ) ;
#7285 = PLANE ( 'NONE',  #21150 ) ;
#7286 = PLANE ( 'NONE',  #43514 ) ;
#7287 = VERTEX_POINT ( 'NONE', #29227 ) ;
#7288 = DIRECTION ( 'NONE',  ( -1.000000000000000000, 0.000000000000000000, 0.000000000000000000 ) ) ;
#7289 = CARTESIAN_POINT ( 'NONE',  ( 0.08139965876239094178, 1.610780518492231694, 0.000000000000000000 ) ) ;
#7290 = VECTOR ( 'NONE', #47542, 39.37007874015748143 ) ;
#7291 = ORIENTED_EDGE ( 'NONE', *, *, #23341, .T. ) ;
#7293 = FACE_OUTER_BOUND ( 'NONE', #33107, .T. ) ;
#7292 = AXIS2_PLACEMENT_3D ( 'NONE', #43347, #11864, #23996 ) ;
#7294 = LINE ( 'NONE', #34911, #34416 ) ;
#7295 = CARTESIAN_POINT ( 'NONE',  ( 0.2727639067037610499, 3.267716535433071279, 1.732283464566921172 ) ) ;
#7296 = VERTEX_POINT ( 'NONE', #44961 ) ;
#7297 = VECTOR ( 'NONE', #48434, 39.37007874015748143 ) ;
#7298 = FACE_OUTER_BOUND ( 'NONE', #26721, .T. ) ;
#7299 = ORIENTED_EDGE ( 'NONE', *, *, #8153, .F. ) ;
#7300 = PLANE ( 'NONE',  #4059 ) ;
#7301 = ORIENTED_EDGE ( 'NONE', *, *, #10806, .T. ) ;
#7302 = VECTOR ( 'NONE', #16442, 39.37007874015748143 ) ;
#7303 = CARTESIAN_POINT ( 'NONE',  ( 1.084824920504545324E-16, 0.000000000000000000, 0.8858267716535433989 ) ) ;
#7304 = ORIENTED_EDGE ( 'NONE', *, *, #46443, .F. ) ;
#7305 = DIRECTION ( 'NONE',  ( 0.000000000000000000, 0.000000000000000000, 1.000000000000000000 ) ) ;
#7307 = VECTOR ( 'NONE', #30393, 39.37007874015748143 ) ;
#7306 = CARTESIAN_POINT ( 'NONE',  ( -1.909347346926324906, 3.346456692913386100, -1.299212598425193210 ) ) ;
#7308 = LINE ( 'NONE', #11431, #20270 ) ;
#7309 = EDGE_LOOP ( 'NONE', ( #49828, #43211, #718, #25288 ) ) ;
#7310 = EDGE_CURVE ( 'NONE', #1759, #38943, #45207, .T. ) ;
#7311 = ORIENTED_EDGE ( 'NONE', *, *, #20561, .T. ) ;
#7312 = ORIENTED_EDGE ( 'NONE', *, *, #10696, .T. ) ;
#7313 = DIRECTION ( 'NONE',  ( 0.000000000000000000, 0.000000000000000000, 1.000000000000000000 ) ) ;
#7314 = DIRECTION ( 'NONE',  ( 1.734723475976806848E-16, -0.000000000000000000, 1.000000000000000000 ) ) ;
#7315 = EDGE_CURVE ( 'NONE', #17605, #29278, #11880, .T. ) ;
#7316 = ORIENTED_EDGE ( 'NONE', *, *, #42078, .T. ) ;
#7317 = ORIENTED_EDGE ( 'NONE', *, *, #17402, .F. ) ;
#7318 = FACE_OUTER_BOUND ( 'NONE', #26608, .T. ) ;
#7319 = LINE ( 'NONE', #23060, #46655 ) ;
#7320 = CARTESIAN_POINT ( 'NONE',  ( -0.2727639067037607723, 0.000000000000000000, 0.4724409448818869817 ) ) ;
#7321 = ADVANCED_FACE ( 'NONE', ( #7757 ), #14991, .T. ) ;
#7322 = EDGE_CURVE ( 'NONE', #5467, #19694, #11382, .T. ) ;
#7323 = VERTEX_POINT ( 'NONE', #39252 ) ;
#7324 = ORIENTED_EDGE ( 'NONE', *, *, #20107, .T. ) ;
#7325 = FACE_OUTER_BOUND ( 'NONE', #23473, .T. ) ;
#7326 = DIRECTION ( 'NONE',  ( 1.734723475976806848E-16, 0.000000000000000000, 1.000000000000000000 ) ) ;
#7327 = AXIS2_PLACEMENT_3D ( 'NONE', #50182, #6623, #6367 ) ;
#7328 = DIRECTION ( 'NONE',  ( 1.000000000000000000, 0.000000000000000000, 0.000000000000000000 ) ) ;
#7329 = EDGE_CURVE ( 'NONE', #47752, #46412, #46464, .T. ) ;
#7330 = EDGE_LOOP ( 'NONE', ( #21924, #44507, #49002, #48547, #29006 ) ) ;
#7331 = DIRECTION ( 'NONE',  ( 0.000000000000000000, 0.000000000000000000, -1.000000000000000000 ) ) ;
#7332 = ORIENTED_EDGE ( 'NONE', *, *, #50373, .F. ) ;
#7333 = CARTESIAN_POINT ( 'NONE',  ( 0.000000000000000000, 3.346456692913386100, 0.000000000000000000 ) ) ;
#7334 = ORIENTED_EDGE ( 'NONE', *, *, #41074, .F. ) ;
#7335 = VERTEX_POINT ( 'NONE', #35134 ) ;
#7336 = CARTESIAN_POINT ( 'NONE',  ( -0.07591351300297333182, 3.346456692913386100, -0.1574803149606301411 ) ) ;
#7337 = CARTESIAN_POINT ( 'NONE',  ( -0.8942052331142552601, 3.267716535433071279, 2.007874015748021268 ) ) ;
#7338 = VECTOR ( 'NONE', #25928, 39.37007874015748143 ) ;
#7339 = VECTOR ( 'NONE', #6172, 39.37007874015748143 ) ;
#7340 = DIRECTION ( 'NONE',  ( 0.000000000000000000, 1.000000000000000000, -0.000000000000000000 ) ) ;
#7341 = ADVANCED_FACE ( 'NONE', ( #5 ), #33181, .T. ) ;
#7342 = LINE ( 'NONE', #23082, #21163 ) ;
#7344 = CARTESIAN_POINT ( 'NONE',  ( 0.5859249214857252808, 1.049866565877817237, -1.938067127299249792 ) ) ;
#7343=STYLED_ITEM('',(#51080),#40963);
#7345 = VERTEX_POINT ( 'NONE', #42862 ) ;
#7346 = EDGE_CURVE ( 'NONE', #22651, #33992, #35389, .T. ) ;
#7347 = AXIS2_PLACEMENT_3D ( 'NONE', #25386, #49850, #17390 ) ;
#7348 = ORIENTED_EDGE ( 'NONE', *, *, #50118, .F. ) ;
#7349 = CARTESIAN_POINT ( 'NONE',  ( 0.1968503937007878291, 3.346456692913386100, 2.097080421798980687 ) ) ;
#7350 = LINE ( 'NONE', #34965, #31689 ) ;
#7351 = DIRECTION ( 'NONE',  ( 0.9998717552508121775, 0.01601477604151182663, 0.000000000000000000 ) ) ;
#7352 = CARTESIAN_POINT ( 'NONE',  ( 9.902948977032876513E-17, 3.267716535433071279, -1.717887807185943447E-32 ) ) ;
#7353 = ORIENTED_EDGE ( 'NONE', *, *, #18990, .T. ) ;
#7354 = CARTESIAN_POINT ( 'NONE',  ( -2.947574761915765063, 1.673315526576397261, -0.1816379373805333819 ) ) ;
#7355 = EDGE_CURVE ( 'NONE', #16989, #33135, #24090, .T. ) ;
#7356 = DIRECTION ( 'NONE',  ( 1.000000000000000000, 0.000000000000000000, -3.469446951953613696E-16 ) ) ;
#7357 = EDGE_LOOP ( 'NONE', ( #46284, #22099, #24070, #34534 ) ) ;
#7358 = LINE ( 'NONE', #38850, #50399 ) ;
#7359 = DIRECTION ( 'NONE',  ( 1.734723475976806848E-16, -0.000000000000000000, 1.000000000000000000 ) ) ;
#7360 = FACE_OUTER_BOUND ( 'NONE', #49193, .T. ) ;
#7361 = FACE_OUTER_BOUND ( 'NONE', #21589, .T. ) ;
#7362 = LINE ( 'NONE', #23601, #29964 ) ;
#7363 = DIRECTION ( 'NONE',  ( -0.000000000000000000, 1.000000000000000000, -0.000000000000000000 ) ) ;
#7364 = ORIENTED_EDGE ( 'NONE', *, *, #39375, .F. ) ;
#7365 = CARTESIAN_POINT ( 'NONE',  ( -0.2727639067037602172, 0.000000000000000000, 1.732283464566921172 ) ) ;
#7366 = ORIENTED_EDGE ( 'NONE', *, *, #49012, .T. ) ;
#7367 = LINE ( 'NONE', #23108, #19571 ) ;
#7368 = VECTOR ( 'NONE', #13248, 39.37007874015748143 ) ;
#7369 = CARTESIAN_POINT ( 'NONE',  ( -1.547992802794810663, 1.592736631120135860, -2.214354780049298199 ) ) ;
#7370 = CARTESIAN_POINT ( 'NONE',  ( 0.1968503937007871074, 3.267716535433071279, -6.829619984160646953E-17 ) ) ;
#7371 = VECTOR ( 'NONE', #15613, 39.37007874015748143 ) ;
#7372 = ORIENTED_EDGE ( 'NONE', *, *, #40594, .F. ) ;
#7373 = ORIENTED_EDGE ( 'NONE', *, *, #5620, .T. ) ;
#7374 = CARTESIAN_POINT ( 'NONE',  ( -0.2727639067037607723, 0.000000000000000000, 0.4724409448818869817 ) ) ;
#7375 = DIRECTION ( 'NONE',  ( -1.000000000000000000, 0.000000000000000000, 1.734723475976806848E-16 ) ) ;
#7376 = EDGE_CURVE ( 'NONE', #15755, #49388, #23248, .T. ) ;
#7377 = LINE ( 'NONE', #43229, #49704 ) ;
#7378 = CARTESIAN_POINT ( 'NONE',  ( 0.07982360342473591996, 1.709180471932028711, 0.000000000000000000 ) ) ;
#7379 = AXIS2_PLACEMENT_3D ( 'NONE', #7043, #27404, #22789 ) ;
#7380 = CARTESIAN_POINT ( 'NONE',  ( 0.08119777152254364916, 1.623385212329073957, 0.000000000000000000 ) ) ;
#7381 = EDGE_CURVE ( 'NONE', #39165, #31511, #1830, .T. ) ;
#7382 = PLANE ( 'NONE',  #29745 ) ;
#7383 = ORIENTED_EDGE ( 'NONE', *, *, #11346, .T. ) ;
#7384 = EDGE_CURVE ( 'NONE', #43635, #22497, #23007, .T. ) ;
#7385 = ORIENTED_EDGE ( 'NONE', *, *, #12845, .F. ) ;
#7386 = LINE ( 'NONE', #7134, #47152 ) ;
#7387 = ADVANCED_FACE ( 'NONE', ( #38258 ), #30507, .T. ) ;
#7388 = DIRECTION ( 'NONE',  ( 0.9639628606958511314, 0.000000000000000000, 0.2660368455666826115 ) ) ;
#7389 = ORIENTED_EDGE ( 'NONE', *, *, #7697, .T. ) ;
#7390 = DIRECTION ( 'NONE',  ( 5.779879058772725700E-18, 1.000000000000000000, -1.286990067732317241E-16 ) ) ;
#7391 = ORIENTED_EDGE ( 'NONE', *, *, #13146, .F. ) ;
#7392 = ORIENTED_EDGE ( 'NONE', *, *, #7530, .T. ) ;
#7393 = EDGE_CURVE ( 'NONE', #48759, #48160, #28208, .T. ) ;
#7394 = VECTOR ( 'NONE', #40160, 39.37007874015748143 ) ;
#7395 = ORIENTED_EDGE ( 'NONE', *, *, #35, .T. ) ;
#7396 = VERTEX_POINT ( 'NONE', #50076 ) ;
#7397 = DIRECTION ( 'NONE',  ( -3.469446951953613696E-16, 0.000000000000000000, -1.000000000000000000 ) ) ;
#7398 = B_SPLINE_CURVE_WITH_KNOTS ( 'NONE', 3,
 ( #13012, #8112, #11984, #8370 ),
 .UNSPECIFIED., .F., .F.,
 ( 4, 4 ),
 ( 0.01416295713610008465, 0.03074759226334981832 ),
 .UNSPECIFIED. ) ;
#7399 = EDGE_CURVE ( 'NONE', #36975, #3200, #43046, .T. ) ;
#7400 = LINE ( 'NONE', #42998, #36154 ) ;
#7401 = CARTESIAN_POINT ( 'NONE',  ( -2.151809081513409438, 1.574803149606302854, 0.2418202932658341242 ) ) ;
#7402 = PLANE ( 'NONE',  #25901 ) ;
#7403 = AXIS2_PLACEMENT_3D ( 'NONE', #14196, #34082, #29947 ) ;
#7404 = EDGE_CURVE ( 'NONE', #45000, #27097, #45514, .T. ) ;
#7405 = LINE ( 'NONE', #34018, #13231 ) ;
#7406 = DIRECTION ( 'NONE',  ( 0.000000000000000000, 0.000000000000000000, -1.000000000000000000 ) ) ;
#7407 = LINE ( 'NONE', #27009, #19560 ) ;
#7408 = VERTEX_POINT ( 'NONE', #7007 ) ;
#7409 = CARTESIAN_POINT ( 'NONE',  ( 0.000000000000000000, 3.267716535433071279, -6.146657985744592735E-16 ) ) ;
#7410 = CARTESIAN_POINT ( 'NONE',  ( -0.8182917201112819283, 0.000000000000000000, -0.1574803149606301411 ) ) ;
#7411 = AXIS2_PLACEMENT_3D ( 'NONE', #18358, #45946, #34369 ) ;
#7412 = DIRECTION ( 'NONE',  ( -3.469446951953613696E-16, 0.000000000000000000, -1.000000000000000000 ) ) ;
#7413 = ADVANCED_FACE ( 'NONE', ( #22755 ), #38511, .T. ) ;
#7414 = CARTESIAN_POINT ( 'NONE',  ( -1.691705575432908004, 0.0005574328069680100587, -0.4365989502721870363 ) ) ;
#7415 = ORIENTED_EDGE ( 'NONE', *, *, #49599, .T. ) ;
#7416 = CARTESIAN_POINT ( 'NONE',  ( 1.560669927219590747, 3.346456692913386100, 0.1574803149606283648 ) ) ;
#7417 = DIRECTION ( 'NONE',  ( -1.045785279492541006E-16, -1.000000000000000000, -5.036236473261559574E-17 ) ) ;
#7418 = VERTEX_POINT ( 'NONE', #50316 ) ;
#7419 = FACE_OUTER_BOUND ( 'NONE', #16415, .T. ) ;
#7420 = CARTESIAN_POINT ( 'NONE',  ( 2.615580629650553046, 0.9847334299463360585, -0.1667280637083841666 ) ) ;
#7421 = EDGE_CURVE ( 'NONE', #14850, #9971, #3380, .T. ) ;
#7422 = CARTESIAN_POINT ( 'NONE',  ( 2.164971648505046975, 6.692913385826772199, -0.04070796836118355938 ) ) ;
#7423 = ORIENTED_EDGE ( 'NONE', *, *, #31093, .T. ) ;
#7424 = CARTESIAN_POINT ( 'NONE',  ( -0.2727639067037608278, 0.000000000000000000, -0.03937007874015908959 ) ) ;
#7425 = EDGE_CURVE ( 'NONE', #4026, #48864, #46712, .T. ) ;
#7426 = FACE_OUTER_BOUND ( 'NONE', #22803, .T. ) ;
#7427 = LINE ( 'NONE', #31177, #29219 ) ;
#7428 = CARTESIAN_POINT ( 'NONE',  ( -0.9836083787002326551, 6.692913385826772199, -1.929060376159713597 ) ) ;
#7429 = ORIENTED_EDGE ( 'NONE', *, *, #47549, .F. ) ;
#7430 = B_SPLINE_CURVE_WITH_KNOTS ( 'NONE', 3,
 ( #9909, #9396, #36515, #16896 ),
 .UNSPECIFIED., .F., .F.,
 ( 4, 4 ),
 ( 6.447518927879251161E-07, 0.003992160187270875696 ),
 .UNSPECIFIED. ) ;
#7431 = ORIENTED_EDGE ( 'NONE', *, *, #48755, .T. ) ;
#7432 = ORIENTED_EDGE ( 'NONE', *, *, #15908, .F. ) ;
#7433 = CARTESIAN_POINT ( 'NONE',  ( -1.651646936617113148, 1.205361022782829114E-17, 0.5883978091303396774 ) ) ;
#7434 = ORIENTED_EDGE ( 'NONE', *, *, #40449, .F. ) ;
#7435 = CARTESIAN_POINT ( 'NONE',  ( 1.880560108460158419, 1.049866565877817681, -0.7502705392085819991 ) ) ;
#7436 = CARTESIAN_POINT ( 'NONE',  ( -1.636583440222564301, 3.267716535433071279, -1.259842519685034468 ) ) ;
#7437 = ORIENTED_EDGE ( 'NONE', *, *, #34010, .F. ) ;
#7438 = EDGE_CURVE ( 'NONE', #34884, #48573, #47723, .T. ) ;
#7439 = DIRECTION ( 'NONE',  ( -0.000000000000000000, 1.000000000000000000, -0.000000000000000000 ) ) ;
#7440 = AXIS2_PLACEMENT_3D ( 'NONE', #27958, #50636, #15586 ) ;
#7441 = VERTEX_POINT ( 'NONE', #8524 ) ;
#7442 = CYLINDRICAL_SURFACE ( 'NONE', #2648, 2.106299212598425008 ) ;
#7443 = EDGE_CURVE ( 'NONE', #41084, #12747, #524, .T. ) ;
#7444 = ORIENTED_EDGE ( 'NONE', *, *, #16165, .F. ) ;
#7445 = EDGE_LOOP ( 'NONE', ( #18188, #11432, #12901, #657 ) ) ;
#7446 = FACE_OUTER_BOUND ( 'NONE', #27167, .T. ) ;
#7447 = EDGE_LOOP ( 'NONE', ( #11875, #14325, #46459, #50683 ) ) ;
#7448 = AXIS2_PLACEMENT_3D ( 'NONE', #39235, #15736, #23999 ) ;
#7449 = CARTESIAN_POINT ( 'NONE',  ( -1.166969139818016199, 0.000000000000000000, -1.929133858267710000 ) ) ;
#7450 = ORIENTED_EDGE ( 'NONE', *, *, #735, .T. ) ;
#7451 = ORIENTED_EDGE ( 'NONE', *, *, #47807, .F. ) ;
#7452 = DIRECTION ( 'NONE',  ( -0.000000000000000000, 1.000000000000000000, -0.000000000000000000 ) ) ;
#7453 = DIRECTION ( 'NONE',  ( 1.000000000000000000, 0.000000000000000000, 0.000000000000000000 ) ) ;
#7454 = ORIENTED_EDGE ( 'NONE', *, *, #35915, .T. ) ;
#7455 = DIRECTION ( 'NONE',  ( -0.000000000000000000, 1.000000000000000000, -0.000000000000000000 ) ) ;
#7456 = ORIENTED_EDGE ( 'NONE', *, *, #3598, .T. ) ;
#7457 = CARTESIAN_POINT ( 'NONE',  ( -0.9948011493083110945, 0.4042499682059492172, 1.112911385528783992 ) ) ;
#7458 = PLANE ( 'NONE',  #4416 ) ;
#7459 = EDGE_CURVE ( 'NONE', #18552, #35065, #12145, .T. ) ;
#7460 = DIRECTION ( 'NONE',  ( 1.734723475976806848E-16, 0.000000000000000000, 1.000000000000000000 ) ) ;
#7461 = B_SPLINE_CURVE_WITH_KNOTS ( 'NONE', 3,
 ( #40203, #36328, #48403, #48156 ),
 .UNSPECIFIED., .F., .F.,
 ( 4, 4 ),
 ( 0.0004689409862730576284, 0.04913255646355430689 ),
 .UNSPECIFIED. ) ;
#7462 = ORIENTED_EDGE ( 'NONE', *, *, #25838, .T. ) ;
#7463 = ORIENTED_EDGE ( 'NONE', *, *, #8411, .F. ) ;
#7464 = APPLICATION_CONTEXT ( 'automotive_design' ) ;
#7465 = LINE ( 'NONE', #3592, #25310 ) ;
#7466 = CARTESIAN_POINT ( 'NONE',  ( -1.166969139818015977, 0.000000000000000000, -0.7874015748031470974 ) ) ;
#7467 = FACE_OUTER_BOUND ( 'NONE', #44777, .T. ) ;
#7468 = CARTESIAN_POINT ( 'NONE',  ( -1.712496953225537411, 3.267716535433071279, 5.941417334598190051E-16 ) ) ;
#7469 = EDGE_CURVE ( 'NONE', #23187, #8950, #39763, .T. ) ;
#7470 = CARTESIAN_POINT ( 'NONE',  ( -1.738757879605812073, 7.027592017269983715E-05, -0.1273499085982673085 ) ) ;
#7471 = VECTOR ( 'NONE', #44031, 39.37007874015748143 ) ;
#7472 = AXIS2_PLACEMENT_3D ( 'NONE', #14811, #11686, #34685 ) ;
#7473 = EDGE_CURVE ( 'NONE', #17100, #21759, #12920, .T. ) ;
#7474 = CARTESIAN_POINT ( 'NONE',  ( -2.454875160333845674, 3.189042514953126961, -0.3543307086614173040 ) ) ;
#7475 = EDGE_CURVE ( 'NONE', #32131, #22636, #34017, .T. ) ;
#7476 = CARTESIAN_POINT ( 'NONE',  ( 2.190654571063535005, 1.742989292944022939, 0.7635320059819211691 ) ) ;
#7477 = VERTEX_POINT ( 'NONE', #27881 ) ;
#7478 = DIRECTION ( 'NONE',  ( 1.734723475976806848E-16, 0.000000000000000000, 1.000000000000000000 ) ) ;
#7479 = VECTOR ( 'NONE', #47907, 39.37007874015748143 ) ;
#7480 = ORIENTED_EDGE ( 'NONE', *, *, #47894, .T. ) ;
#7481 = ORIENTED_EDGE ( 'NONE', *, *, #16363, .T. ) ;
#7482 = LINE ( 'NONE', #46933, #37421 ) ;
#7483 = CARTESIAN_POINT ( 'NONE',  ( 0.7513820654849657776, 1.719936709731724189, 2.142107623314860376 ) ) ;
#7484 = VERTEX_POINT ( 'NONE', #16012 ) ;
#7485 = EDGE_CURVE ( 'NONE', #37048, #47504, #4656, .T. ) ;
#7486 = B_SPLINE_CURVE_WITH_KNOTS ( 'NONE', 3,
 ( #43025, #46876, #438, #7927 ),
 .UNSPECIFIED., .F., .F.,
 ( 4, 4 ),
 ( 2.220418065680204351E-07, 0.01710792206032625551 ),
 .UNSPECIFIED. ) ;
#7487 = DIRECTION ( 'NONE',  ( 1.000000000000000000, 0.000000000000000000, -3.469446951953613696E-16 ) ) ;
#7488 = ORIENTED_EDGE ( 'NONE', *, *, #29260, .T. ) ;
#7489 = CARTESIAN_POINT ( 'NONE',  ( -0.2727639067037602727, 3.346456692913386100, 0.9055118110236167750 ) ) ;
#7490 = ORIENTED_EDGE ( 'NONE', *, *, #42857, .F. ) ;
#7491 = EDGE_CURVE ( 'NONE', #23622, #50196, #3020, .T. ) ;
#7492 = DIRECTION ( 'NONE',  ( 0.000000000000000000, 0.000000000000000000, 1.000000000000000000 ) ) ;
#7493 = DIRECTION ( 'NONE',  ( -0.01601477604151182663, 0.9998717552508123996, -0.000000000000000000 ) ) ;
#7494 = EDGE_CURVE ( 'NONE', #34034, #46418, #783, .T. ) ;
#7495 = EDGE_CURVE ( 'NONE', #7692, #6991, #32286, .T. ) ;
#7496 = ORIENTED_EDGE ( 'NONE', *, *, #27487, .T. ) ;
#7497 = CARTESIAN_POINT ( 'NONE',  ( -1.712496953225537188, 3.267716535433071279, -0.1574803149606297248 ) ) ;
#7498 = VERTEX_POINT ( 'NONE', #44139 ) ;
#7499 = VERTEX_POINT ( 'NONE', #12654 ) ;
#7500 = PRODUCT_DEFINITION_SHAPE ( 'NONE', 'NONE',  #31336 ) ;
#7501 = DIRECTION ( 'NONE',  ( 0.9009688679024218105, -1.160734090543304660E-16, -0.4338837391175526803 ) ) ;
#7502 = DIRECTION ( 'NONE',  ( 1.000000000000000000, 0.000000000000000000, 0.000000000000000000 ) ) ;
#7503 = CARTESIAN_POINT ( 'NONE',  ( 0.4350747367505080065, 6.692913385826772199, -2.121846421795415605 ) ) ;
#7504 = AXIS2_PLACEMENT_3D ( 'NONE', #29893, #18266, #13642 ) ;
#7505 = VERTEX_POINT ( 'NONE', #1291 ) ;
#7506 = VECTOR ( 'NONE', #20966, 39.37007874015748143 ) ;
#7507 = PLANE ( 'NONE',  #47605 ) ;
#7508 = CARTESIAN_POINT ( 'NONE',  ( 1.979793062125284608, 1.750113821271474857, 2.191257344206569257 ) ) ;
#7509 = VERTEX_POINT ( 'NONE', #8269 ) ;
#7510 = CARTESIAN_POINT ( 'NONE',  ( 0.000000000000000000, 1.574803149606302854, 0.000000000000000000 ) ) ;
#7511 = VERTEX_POINT ( 'NONE', #28388 ) ;
#7512 = ORIENTED_EDGE ( 'NONE', *, *, #5679, .F. ) ;
#7513 = VECTOR ( 'NONE', #42355, 39.37007874015748143 ) ;
#7514 = ORIENTED_EDGE ( 'NONE', *, *, #34299, .T. ) ;
#7515 = DIRECTION ( 'NONE',  ( 1.000000000000000000, 0.000000000000000000, 0.000000000000000000 ) ) ;
#7516 = VECTOR ( 'NONE', #31936, 39.37007874015748143 ) ;
#7517 = DIRECTION ( 'NONE',  ( 1.000000000000000000, 0.000000000000000000, 0.000000000000000000 ) ) ;
#7518 = DIRECTION ( 'NONE',  ( 1.000000000000000000, 0.000000000000000000, 0.000000000000000000 ) ) ;
#7519 = CARTESIAN_POINT ( 'NONE',  ( 0.000000000000000000, 3.267716535433071279, 0.000000000000000000 ) ) ;
#7520 = ORIENTED_EDGE ( 'NONE', *, *, #33139, .F. ) ;
#7521 = ORIENTED_EDGE ( 'NONE', *, *, #9107, .F. ) ;
#7522 = CARTESIAN_POINT ( 'NONE',  ( 0.2727639067037602172, 3.267716535433071279, -2.244094488188969727 ) ) ;
#7523 = DIRECTION ( 'NONE',  ( -0.000000000000000000, 1.000000000000000000, -0.000000000000000000 ) ) ;
#7524 = ORIENTED_EDGE ( 'NONE', *, *, #4583, .F. ) ;
#7525 = CARTESIAN_POINT ( 'NONE',  ( -1.363819533518803473, 0.000000000000000000, 2.047244094488179567 ) ) ;
#7526 = PLANE ( 'NONE',  #11119 ) ;
#7527 = EDGE_CURVE ( 'NONE', #36336, #46441, #36668, .T. ) ;
#7528 = EDGE_CURVE ( 'NONE', #4542, #35067, #11738, .T. ) ;
#7529 = CARTESIAN_POINT ( 'NONE',  ( 0.000000000000000000, 3.267716535433071279, 0.000000000000000000 ) ) ;
#7530 = EDGE_CURVE ( 'NONE', #35509, #18363, #10936, .T. ) ;
#7531 = CARTESIAN_POINT ( 'NONE',  ( 1.909347346926324684, 3.267716535433071279, 1.102362204724403938 ) ) ;
#7532 = LINE ( 'NONE', #45990, #17997 ) ;
#7533 = EDGE_LOOP ( 'NONE', ( #32206, #19321, #34891, #42182 ) ) ;
#7534 = CARTESIAN_POINT ( 'NONE',  ( 1.363819533518803251, 3.346456692913386100, 0.2755905511810996522 ) ) ;
#7535 = LINE ( 'NONE', #23275, #19433 ) ;
#7536 = VECTOR ( 'NONE', #16950, 39.37007874015748143 ) ;
#7538 = EDGE_CURVE ( 'NONE', #27191, #34440, #28653, .T. ) ;
#7537 = ORIENTED_EDGE ( 'NONE', *, *, #8663, .T. ) ;
#7539 = CARTESIAN_POINT ( 'NONE',  ( -2.097080421798980687, 3.346456692913386100, -0.1968503937007880511 ) ) ;
#7540 = COLOUR_RGB ( '',0.7921568627450980005, 0.8196078431372548767, 0.9333333333333333481 ) ;
#7541 = DIRECTION ( 'NONE',  ( -0.000000000000000000, 1.000000000000000000, -0.000000000000000000 ) ) ;
#7542 = DIRECTION ( 'NONE',  ( -0.000000000000000000, -1.000000000000000000, -0.000000000000000000 ) ) ;
#7543 = ORIENTED_EDGE ( 'NONE', *, *, #41962, .T. ) ;
#7544 = CIRCLE ( 'NONE', #32287, 2.244934639244525076 ) ;
#7545 = ORIENTED_EDGE ( 'NONE', *, *, #33311, .T. ) ;
#7546 = FACE_OUTER_BOUND ( 'NONE', #14457, .T. ) ;
#7547 = AXIS2_PLACEMENT_3D ( 'NONE', #10808, #22939, #46154 ) ;
#7549 = EDGE_LOOP ( 'NONE', ( #43921, #41304, #25724, #32061 ) ) ;
#7548 = EDGE_CURVE ( 'NONE', #29935, #15133, #40286, .T. ) ;
#7550 = CARTESIAN_POINT ( 'NONE',  ( -1.461782879395278290, 0.000000000000000000, -1.598346982901829527 ) ) ;
#7551 = ORIENTED_EDGE ( 'NONE', *, *, #31581, .T. ) ;
#7552 = VECTOR ( 'NONE', #31605, 39.37007874015748143 ) ;
#7553 = CARTESIAN_POINT ( 'NONE',  ( 0.2727639067037610499, 0.000000000000000000, 1.102362204724404160 ) ) ;
#7554 = EDGE_CURVE ( 'NONE', #25081, #41228, #20651, .T. ) ;
#7555 = CARTESIAN_POINT ( 'NONE',  ( 1.236813753895251722, 1.205361022782829114E-17, -2.681693691597563767 ) ) ;
#7556 = DIRECTION ( 'NONE',  ( -0.000000000000000000, 1.000000000000000000, -0.000000000000000000 ) ) ;
#7557 = EDGE_CURVE ( 'NONE', #39081, #9101, #28905, .T. ) ;
#7558 = VERTEX_POINT ( 'NONE', #23761 ) ;
#7559 = ORIENTED_EDGE ( 'NONE', *, *, #25261, .T. ) ;
#7560 = ORIENTED_EDGE ( 'NONE', *, *, #11458, .T. ) ;
#7561 = DIRECTION ( 'NONE',  ( -0.000000000000000000, 1.000000000000000000, -0.000000000000000000 ) ) ;
#7562 = DIRECTION ( 'NONE',  ( -0.000000000000000000, -1.000000000000000000, -0.000000000000000000 ) ) ;
#7564 = VERTEX_POINT ( 'NONE', #37186 ) ;
#7563 = EDGE_CURVE ( 'NONE', #20150, #30476, #19870, .T. ) ;
#7565 = ORIENTED_EDGE ( 'NONE', *, *, #43024, .F. ) ;
#7566 = PLANE ( 'NONE',  #33070 ) ;
#7567 = CARTESIAN_POINT ( 'NONE',  ( 1.560669927219590747, 3.346456692913386100, -0.7874015748031473194 ) ) ;
#7568 = CARTESIAN_POINT ( 'NONE',  ( -1.536664496436148184E-16, 3.346456692913386100, 0.1181102362204701633 ) ) ;
#7569 = ADVANCED_FACE ( 'NONE', ( #29428 ), #25298, .F. ) ;
#7570 = EDGE_LOOP ( 'NONE', ( #24201, #32730, #30048, #11757 ) ) ;
#7571 = VERTEX_POINT ( 'NONE', #1802 ) ;
#7572 = CARTESIAN_POINT ( 'NONE',  ( 2.059322335531026837, 3.346456692913386100, -0.6692913385826764205 ) ) ;
#7573 = DIRECTION ( 'NONE',  ( -1.000000000000000000, -0.000000000000000000, -0.000000000000000000 ) ) ;
#7574 = LINE ( 'NONE', #19687, #17943 ) ;
#7575 = ORIENTED_EDGE ( 'NONE', *, *, #26322, .F. ) ;
#7576 = DIRECTION ( 'NONE',  ( 0.9749279121818227312, -2.586762438145473843E-17, 0.2225209339563184452 ) ) ;
#7577 = ORIENTED_EDGE ( 'NONE', *, *, #27685, .F. ) ;
#7578 = CARTESIAN_POINT ( 'NONE',  ( 0.1067246931122726866, 0.02962905676920215767, 0.000000000000000000 ) ) ;
#7579 = ORIENTED_EDGE ( 'NONE', *, *, #20305, .F. ) ;
#7580 = EDGE_LOOP ( 'NONE', ( #49385, #34554, #24325, #6697 ) ) ;
#7581 = DIRECTION ( 'NONE',  ( 0.000000000000000000, 0.000000000000000000, -1.000000000000000000 ) ) ;
#7582 = LINE ( 'NONE', #26691, #25866 ) ;
#7583 = VECTOR ( 'NONE', #33905, 39.37007874015748143 ) ;
#7585 = VECTOR ( 'NONE', #42431, 39.37007874015748143 ) ;
#7584 = DIRECTION ( 'NONE',  ( 0.7818314824680221431, 0.000000000000000000, 0.6234898018587431423 ) ) ;
#7586 = CARTESIAN_POINT ( 'NONE',  ( -2.165574327476177174, 1.677377729380559845, 1.109459651199706576 ) ) ;
#7587 = DIRECTION ( 'NONE',  ( 0.9998717552508121775, 0.01601477604151182663, 0.000000000000000000 ) ) ;
#7588 = VERTEX_POINT ( 'NONE', #49758 ) ;
#7589 = EDGE_LOOP ( 'NONE', ( #35385, #19970, #16934, #11085 ) ) ;
#7590 = VECTOR ( 'NONE', #37936, 39.37007874015748143 ) ;
#7591 = CONICAL_SURFACE ( 'NONE', #26565, 2.244934639244524632, 1.554780866114618743 ) ;
#7592 = VERTEX_POINT ( 'NONE', #45148 ) ;
#7593 = DIRECTION ( 'NONE',  ( 0.000000000000000000, -1.000000000000000000, 0.000000000000000000 ) ) ;
#7594 = DIRECTION ( 'NONE',  ( 1.000000000000000000, 0.000000000000000000, 0.000000000000000000 ) ) ;
#7595 = VECTOR ( 'NONE', #40567, 39.37007874015748143 ) ;
#7596 = EDGE_CURVE ( 'NONE', #9369, #9748, #17554, .T. ) ;
#7597 = PLANE ( 'NONE',  #13825 ) ;
#7598 = CARTESIAN_POINT ( 'NONE',  ( 1.083598637574781920, 1.736150426126270130, 2.747180975113346246 ) ) ;
#7599 = EDGE_LOOP ( 'NONE', ( #38048, #10678, #20373 ) ) ;
#7600 = EDGE_CURVE ( 'NONE', #24676, #34367, #25043, .T. ) ;
#7601 = CARTESIAN_POINT ( 'NONE',  ( -1.205050450470247725, 0.008618577144216254052, 1.304493073717302165 ) ) ;
#7602 = LINE ( 'NONE', #23092, #25683 ) ;
#7603 = EDGE_CURVE ( 'NONE', #39521, #8450, #2682, .T. ) ;
#7604 = VERTEX_POINT ( 'NONE', #33062 ) ;
#7605 = CARTESIAN_POINT ( 'NONE',  ( -1.775400203342670347, 1.593155925640307835, -2.359903268218729089 ) ) ;
#7606 = DIRECTION ( 'NONE',  ( -0.000000000000000000, 1.000000000000000000, -0.000000000000000000 ) ) ;
#7607 = LINE ( 'NONE', #18973, #4063 ) ;
#7608 = CARTESIAN_POINT ( 'NONE',  ( 0.2727639067037609943, 3.346456692913386100, 1.535433070866133898 ) ) ;
#7609 = DIRECTION ( 'NONE',  ( 1.734723475976806848E-16, -0.000000000000000000, 1.000000000000000000 ) ) ;
#7610 = FACE_OUTER_BOUND ( 'NONE', #25668, .T. ) ;
#7611 = ORIENTED_EDGE ( 'NONE', *, *, #5634, .T. ) ;
#7612 = CARTESIAN_POINT ( 'NONE',  ( -1.636583440222563635, 3.346456692913386100, 0.9448818897637749625 ) ) ;
#7613 = ORIENTED_EDGE ( 'NONE', *, *, #14616, .T. ) ;
#7614 = CARTESIAN_POINT ( 'NONE',  ( -2.378214753669538162, 1.674009934365706220, -0.4923338061332758198 ) ) ;
#7615 = AXIS2_PLACEMENT_3D ( 'NONE', #31005, #26863, #14759 ) ;
#7616 = CARTESIAN_POINT ( 'NONE',  ( 0.000000000000000000, 7.874015748031496287, 0.000000000000000000 ) ) ;
#7617 = EDGE_CURVE ( 'NONE', #35577, #26630, #10063, .T. ) ;
#7618 = DIRECTION ( 'NONE',  ( 1.000000000000000000, 0.000000000000000000, 0.000000000000000000 ) ) ;
#7619 = CIRCLE ( 'NONE', #36488, 2.165354330708661568 ) ;
#7620 = ORIENTED_EDGE ( 'NONE', *, *, #390, .T. ) ;
#7621 = ORIENTED_EDGE ( 'NONE', *, *, #4111, .F. ) ;
#7622 = DIRECTION ( 'NONE',  ( -1.000000000000000000, 0.000000000000000000, 0.000000000000000000 ) ) ;
#7623 = LINE ( 'NONE', #47328, #25451 ) ;
#7624 = EDGE_CURVE ( 'NONE', #16195, #3395, #42423, .T. ) ;
#7625 = EDGE_CURVE ( 'NONE', #25938, #17945, #21684, .T. ) ;
#7626 = ORIENTED_EDGE ( 'NONE', *, *, #50115, .F. ) ;
#7627 = AXIS2_PLACEMENT_3D ( 'NONE', #9020, #48468, #8504 ) ;
#7628 = DIRECTION ( 'NONE',  ( -1.000000000000000000, 0.000000000000000000, 0.000000000000000000 ) ) ;
#7629 = CARTESIAN_POINT ( 'NONE',  ( -0.2727639067037608278, 3.267716535433071279, -0.03937007874015908959 ) ) ;
#7630 = CARTESIAN_POINT ( 'NONE',  ( 1.363819533518803029, 3.346456692913386100, -1.102362204724405714 ) ) ;
#7631 = VECTOR ( 'NONE', #37138, 39.37007874015748143 ) ;
#7632 = CARTESIAN_POINT ( 'NONE',  ( -1.748857564090981809, 1.691995931334618453, -2.379187624440585402 ) ) ;
#7633 = AXIS2_PLACEMENT_3D ( 'NONE', #5945, #10080, #6711 ) ;
#7634 = ORIENTED_EDGE ( 'NONE', *, *, #41930, .T. ) ;
#7635 = EDGE_LOOP ( 'NONE', ( #40109, #10309, #18116, #46703 ) ) ;
#7636 = CARTESIAN_POINT ( 'NONE',  ( 0.000000000000000000, 5.905511811023623991, 0.000000000000000000 ) ) ;
#7637 = CARTESIAN_POINT ( 'NONE',  ( -2.182111253630085290, 3.267716535433071279, -0.1968503937007880511 ) ) ;
#7638 = ORIENTED_EDGE ( 'NONE', *, *, #38082, .T. ) ;
#7639 = CARTESIAN_POINT ( 'NONE',  ( 1.015142113812069979, 3.346456692913386100, 1.417322834645662777 ) ) ;
#7640 = ORIENTED_EDGE ( 'NONE', *, *, #27711, .F. ) ;
#7641 = ORIENTED_EDGE ( 'NONE', *, *, #11859, .T. ) ;
#7642 = CARTESIAN_POINT ( 'NONE',  ( -2.044241703397525978, 1.205361022782829114E-17, -0.7159595814952911530 ) ) ;
#7643 = ORIENTED_EDGE ( 'NONE', *, *, #43693, .T. ) ;
#7644 = VERTEX_POINT ( 'NONE', #1551 ) ;
#7645 = CARTESIAN_POINT ( 'NONE',  ( -0.4433489891367851654, -2.598029575652208120E-16, 2.167441310503416041 ) ) ;
#7646 = ORIENTED_EDGE ( 'NONE', *, *, #12257, .F. ) ;
#7647 = CARTESIAN_POINT ( 'NONE',  ( 1.015142113812069313, 3.267716535433071279, -1.299212598425193210 ) ) ;
#7648 = DIRECTION ( 'NONE',  ( 1.734723475976806848E-16, -0.000000000000000000, 1.000000000000000000 ) ) ;
#7649 = CARTESIAN_POINT ( 'NONE',  ( -0.2727639067037611054, 3.346456692913386100, -2.244094488188968395 ) ) ;
#7650 = LINE ( 'NONE', #42250, #40438 ) ;
#7651 = VECTOR ( 'NONE', #24663, 39.37007874015748143 ) ;
#7652 = CARTESIAN_POINT ( 'NONE',  ( 2.100227814008711835, 1.751990118145921649, -2.076109931251913565 ) ) ;
#7653 = FACE_OUTER_BOUND ( 'NONE', #18067, .T. ) ;
#7654 = VERTEX_POINT ( 'NONE', #45652 ) ;
#7655 = EDGE_CURVE ( 'NONE', #42444, #5670, #44898, .T. ) ;
#7656 = CARTESIAN_POINT ( 'NONE',  ( -1.712496953225537633, 3.346456692913386100, 1.417322834645662333 ) ) ;
#7657 = CARTESIAN_POINT ( 'NONE',  ( -2.544472138398716332, 1.577093961458839511, 0.8784943024822983171 ) ) ;
#7658 = CARTESIAN_POINT ( 'NONE',  ( 4.268512490100411402E-16, 3.267716535433071279, 1.259842519685033357 ) ) ;
#7659 = ADVANCED_FACE ( 'NONE', ( #2316 ), #9812, .T. ) ;
#7660 = VECTOR ( 'NONE', #37957, 39.37007874015748143 ) ;
#7661 = AXIS2_PLACEMENT_3D ( 'NONE', #37459, #14201, #33333 ) ;
#7662 = ORIENTED_EDGE ( 'NONE', *, *, #13281, .T. ) ;
#7663 = DIRECTION ( 'NONE',  ( -1.000000000000000000, 0.000000000000000000, 0.000000000000000000 ) ) ;
#7664 = EDGE_CURVE ( 'NONE', #32363, #32877, #50450, .T. ) ;
#7665 = PLANE ( 'NONE',  #13742 ) ;
#7666 = EDGE_LOOP ( 'NONE', ( #31190, #7996, #41338, #38938 ) ) ;
#7667 = DIRECTION ( 'NONE',  ( 1.734723475976806848E-16, -0.000000000000000000, 1.000000000000000000 ) ) ;
#7668 = EDGE_CURVE ( 'NONE', #20338, #38076, #37699, .T. ) ;
#7669 = CARTESIAN_POINT ( 'NONE',  ( 2.889674983507178219, 1.448941827424379936, -0.6090712660037606030 ) ) ;
#7670 = VECTOR ( 'NONE', #46114, 39.37007874015748143 ) ;
#7671 = CARTESIAN_POINT ( 'NONE',  ( -0.5455278134075208785, 0.000000000000000000, 0.4330708661417290162 ) ) ;
#7672 = ORIENTED_EDGE ( 'NONE', *, *, #49775, .F. ) ;
#7673 = DIRECTION ( 'NONE',  ( -0.000000000000000000, 1.000000000000000000, -0.000000000000000000 ) ) ;
#7674 = CARTESIAN_POINT ( 'NONE',  ( 1.091055626815042645, 3.346456692913386100, 0.6299212598425161236 ) ) ;
#7675 = DIRECTION ( 'NONE',  ( 0.9749279121818227312, 0.000000000000000000, 0.2225209339563184452 ) ) ;
#7676 = EDGE_CURVE ( 'NONE', #7505, #50172, #30728, .T. ) ;
#7677 = DIRECTION ( 'NONE',  ( -0.000000000000000000, 0.000000000000000000, 1.000000000000000000 ) ) ;
#7678 = VERTEX_POINT ( 'NONE', #49261 ) ;
#7679 = ORIENTED_EDGE ( 'NONE', *, *, #17911, .F. ) ;
#7680 = ORIENTED_EDGE ( 'NONE', *, *, #32428, .F. ) ;
#7681 = DIRECTION ( 'NONE',  ( 1.734723475976806848E-16, -0.000000000000000000, 1.000000000000000000 ) ) ;
#7682 = ORIENTED_EDGE ( 'NONE', *, *, #20356, .T. ) ;
#7683 = EDGE_CURVE ( 'NONE', #25794, #33804, #48810, .T. ) ;
#7684 = CARTESIAN_POINT ( 'NONE',  ( -2.043170538425928662, 3.346456692913386100, -0.5118110236220464460 ) ) ;
#7685 = DIRECTION ( 'NONE',  ( -5.207613805428889878E-18, -1.000000000000000000, 1.159565308550899675E-16 ) ) ;
#7686 = ORIENTED_EDGE ( 'NONE', *, *, #44788, .F. ) ;
#7687 = PLANE ( 'NONE',  #8285 ) ;
#7688 = VERTEX_POINT ( 'NONE', #25549 ) ;
#7689 = EDGE_CURVE ( 'NONE', #30948, #29664, #13941, .T. ) ;
#7690 = LINE ( 'NONE', #42799, #23235 ) ;
#7691 = AXIS2_PLACEMENT_3D ( 'NONE', #32284, #3, #40021 ) ;
#7692 = VERTEX_POINT ( 'NONE', #14443 ) ;
#7693 = ORIENTED_EDGE ( 'NONE', *, *, #14066, .F. ) ;
#7694 = DIRECTION ( 'NONE',  ( 0.000000000000000000, 0.000000000000000000, -1.000000000000000000 ) ) ;
#7695 = VECTOR ( 'NONE', #28748, 39.37007874015748143 ) ;
#7696 = ORIENTED_EDGE ( 'NONE', *, *, #6960, .F. ) ;
#7697 = EDGE_CURVE ( 'NONE', #34149, #13984, #30191, .T. ) ;
#7698 = AXIS2_PLACEMENT_3D ( 'NONE', #12659, #20403, #20658 ) ;
#7699 = AXIS2_PLACEMENT_3D ( 'NONE', #34153, #7027, #14525 ) ;
#7700 = CARTESIAN_POINT ( 'NONE',  ( 1.091055626815042645, 3.267716535433071279, 0.3149606299212578953 ) ) ;
#7701 = ORIENTED_EDGE ( 'NONE', *, *, #51018, .F. ) ;
#7702 = EDGE_LOOP ( 'NONE', ( #37085, #42448, #41875, #19793 ) ) ;
#7703 = LINE ( 'NONE', #42811, #1019 ) ;
#7704 = VECTOR ( 'NONE', #19148, 39.37007874015748143 ) ;
#7705 = CARTESIAN_POINT ( 'NONE',  ( 0.8329809839909850799, 1.633788288308783976, -2.833254665166554442 ) ) ;
#7706 = VERTEX_POINT ( 'NONE', #13427 ) ;
#7707 = LINE ( 'NONE', #51015, #35272 ) ;
#7708 = VERTEX_POINT ( 'NONE', #41306 ) ;
#7709 = CARTESIAN_POINT ( 'NONE',  ( 3.937007874015748143, 5.118110236220475784, 1.181102362204724310 ) ) ;
#7710 = CARTESIAN_POINT ( 'NONE',  ( 3.937007874015748143, 4.960629921259846142, 1.023622047244094446 ) ) ;
#7711 = DIRECTION ( 'NONE',  ( -3.469446951953613696E-16, 0.000000000000000000, -1.000000000000000000 ) ) ;
#7712 = EDGE_LOOP ( 'NONE', ( #21443, #35019, #27850, #16548 ) ) ;
#7713 = VERTEX_POINT ( 'NONE', #14946 ) ;
#7714 = FACE_OUTER_BOUND ( 'NONE', #5512, .T. ) ;
#7715 = DIRECTION ( 'NONE',  ( -1.000000000000000000, 0.000000000000000000, 0.000000000000000000 ) ) ;
#7716 = DIRECTION ( 'NONE',  ( 1.000000000000000000, 0.000000000000000000, 0.000000000000000000 ) ) ;
#7717 = CARTESIAN_POINT ( 'NONE',  ( 1.779568955232893268, 5.905511811023623991, -1.233650562797287575 ) ) ;
#7718 = PLANE ( 'NONE',  #14919 ) ;
#7719 = EDGE_CURVE ( 'NONE', #45211, #50302, #17536, .T. ) ;
#7720 = DIRECTION ( 'NONE',  ( 0.000000000000000000, -1.000000000000000000, 0.000000000000000000 ) ) ;
#7721 = EDGE_LOOP ( 'NONE', ( #50629, #44839, #30146, #42831 ) ) ;
#7722 = ADVANCED_FACE ( 'NONE', ( #38453 ), #50261, .F. ) ;
#7723 = CARTESIAN_POINT ( 'NONE',  ( 0.000000000000000000, 3.267716535433071279, 0.000000000000000000 ) ) ;
#7724 = AXIS2_PLACEMENT_3D ( 'NONE', #17942, #5810, #33707 ) ;
#7725 = ORIENTED_EDGE ( 'NONE', *, *, #7475, .F. ) ;
#7726 = CARTESIAN_POINT ( 'NONE',  ( 0.2727639067037602172, 0.000000000000000000, -1.732283464566922726 ) ) ;
#7727 = AXIS2_PLACEMENT_3D ( 'NONE', #15167, #174, #35049 ) ;
#7728 = ORIENTED_EDGE ( 'NONE', *, *, #11383, .F. ) ;
#7729 = VECTOR ( 'NONE', #19570, 39.37007874015748143 ) ;
#7730 = ORIENTED_EDGE ( 'NONE', *, *, #9136, .T. ) ;
#7732 = VECTOR ( 'NONE', #4365, 39.37007874015748143 ) ;
#7731 = DIRECTION ( 'NONE',  ( 1.000000000000000000, 0.000000000000000000, 0.000000000000000000 ) ) ;
#7733 = CARTESIAN_POINT ( 'NONE',  ( -2.258024766633058622, 0.000000000000000000, 0.1574803149606286423 ) ) ;
#7734 = ORIENTED_EDGE ( 'NONE', *, *, #5054, .F. ) ;
#7735 = CONICAL_SURFACE ( 'NONE', #17668, 1.850107469027523210, 0.6386652850508578450 ) ;
#7736 = CARTESIAN_POINT ( 'NONE',  ( 0.000000000000000000, 3.267716535433071279, -0.3543307086614175816 ) ) ;
#7737 = EDGE_LOOP ( 'NONE', ( #14910, #4636, #7383, #38881 ) ) ;
#7738 = PLANE ( 'NONE',  #31176 ) ;
#7739 = VERTEX_POINT ( 'NONE', #50506 ) ;
#7740 = DIRECTION ( 'NONE',  ( -0.3090169943749582204, -1.160734090543304660E-16, 0.9510565162951500895 ) ) ;
#7741 = LINE ( 'NONE', #8256, #46187 ) ;
#7742 = ADVANCED_FACE ( 'NONE', ( #30698 ), #34819, .F. ) ;
#7743 = ORIENTED_EDGE ( 'NONE', *, *, #14506, .T. ) ;
#7744 = CARTESIAN_POINT ( 'NONE',  ( -0.6214413264104940993, 3.267716535433071279, 2.156057715732899547E-16 ) ) ;
#7745 = ORIENTED_EDGE ( 'NONE', *, *, #33854, .F. ) ;
#7746 = ORIENTED_EDGE ( 'NONE', *, *, #2141, .F. ) ;
#7747 = CARTESIAN_POINT ( 'NONE',  ( -0.3742159057234073494, 0.02192591290182492950, 1.786486621533327712 ) ) ;
#7748 = CARTESIAN_POINT ( 'NONE',  ( 0.3734705886643994721, -0.6299212598425202314, -0.02018660888377523527 ) ) ;
#7749 = FACE_OUTER_BOUND ( 'NONE', #44443, .T. ) ;
#7750 = ADVANCED_FACE ( 'NONE', ( #46409 ), #10093, .T. ) ;
#7751 = ORIENTED_EDGE ( 'NONE', *, *, #3076, .F. ) ;
#7752 = EDGE_CURVE ( 'NONE', #19355, #23628, #18824, .T. ) ;
#7753 = FACE_OUTER_BOUND ( 'NONE', #44676, .T. ) ;
#7754 = DIRECTION ( 'NONE',  ( -3.469446951953613696E-16, 0.000000000000000000, -1.000000000000000000 ) ) ;
#7755 = ADVANCED_FACE ( 'NONE', ( #22948 ), #42307, .F. ) ;
#7756 = EDGE_LOOP ( 'NONE', ( #576, #38498, #14120, #5630 ) ) ;
#7757 = FACE_OUTER_BOUND ( 'NONE', #42751, .T. ) ;
#7758 = VECTOR ( 'NONE', #28539, 39.37007874015748143 ) ;
#7759 = EDGE_CURVE ( 'NONE', #4498, #19371, #9237, .T. ) ;
#7760 = ORIENTED_EDGE ( 'NONE', *, *, #36473, .T. ) ;
#7761 = VECTOR ( 'NONE', #862, 39.37007874015748854 ) ;
#7762 = ORIENTED_EDGE ( 'NONE', *, *, #8355, .T. ) ;
#7763 = VECTOR ( 'NONE', #37043, 39.37007874015748143 ) ;
#7765 = EDGE_CURVE ( 'NONE', #42413, #39696, #11326, .T. ) ;
#7764 = ORIENTED_EDGE ( 'NONE', *, *, #36020, .F. ) ;
#7766 = DIRECTION ( 'NONE',  ( -0.01601477604151182663, 0.9998717552508123996, -0.000000000000000000 ) ) ;
#7767 = VECTOR ( 'NONE', #38724, 39.37007874015748143 ) ;
#7768 = LINE ( 'NONE', #35394, #16776 ) ;
#7769 = CARTESIAN_POINT ( 'NONE',  ( 2.017116292511733633, 3.346456692913386100, 0.7874015748031456541 ) ) ;
#7770 = FACE_OUTER_BOUND ( 'NONE', #13531, .T. ) ;
#7771 = VERTEX_POINT ( 'NONE', #23189 ) ;
#7772 = ORIENTED_EDGE ( 'NONE', *, *, #34386, .F. ) ;
#7773 = CONICAL_SURFACE ( 'NONE', #5315, 3.033577403570480779, 1.554780866114618743 ) ;
#7774 = DIRECTION ( 'NONE',  ( -0.000000000000000000, 1.000000000000000000, -0.000000000000000000 ) ) ;
#7775 = CARTESIAN_POINT ( 'NONE',  ( 2.298430379965446857, 1.646290322915411997, 0.3610056012771685197 ) ) ;
#7776 = VERTEX_POINT ( 'NONE', #38702 ) ;
#7777 = DIRECTION ( 'NONE',  ( -1.000000000000000000, 0.000000000000000000, 0.000000000000000000 ) ) ;
#7778 = FACE_OUTER_BOUND ( 'NONE', #4477, .T. ) ;
#7779 = DIRECTION ( 'NONE',  ( 1.734723475976806848E-16, -0.000000000000000000, 1.000000000000000000 ) ) ;
#7780 = EDGE_CURVE ( 'NONE', #46932, #8029, #7703, .T. ) ;
#7781 = EDGE_CURVE ( 'NONE', #45728, #49614, #6949, .T. ) ;
#7782 = DIRECTION ( 'NONE',  ( -0.8584487936018727616, -5.949974954004205321E-17, 0.5128992774058948045 ) ) ;
#7783 = FACE_OUTER_BOUND ( 'NONE', #20573, .T. ) ;
#7784 = LINE ( 'NONE', #28613, #10591 ) ;
#7785 = ORIENTED_EDGE ( 'NONE', *, *, #19979, .T. ) ;
#7786 = EDGE_CURVE ( 'NONE', #20580, #912, #22446, .T. ) ;
#7787 = LINE ( 'NONE', #27648, #47281 ) ;
#7788 = DIRECTION ( 'NONE',  ( -0.000000000000000000, 1.000000000000000000, -0.000000000000000000 ) ) ;
#7789 = ORIENTED_EDGE ( 'NONE', *, *, #32395, .F. ) ;
#7790 = EDGE_LOOP ( 'NONE', ( #46824, #50217, #19341, #6048, #8898, #25320, #45794, #28968, #324, #24316, #47067, #27145, #50018 ) ) ;
#7791 = FACE_OUTER_BOUND ( 'NONE', #43242, .T. ) ;
#7792 = LINE ( 'NONE', #12171, #2277 ) ;
#7793 = DIRECTION ( 'NONE',  ( -0.000000000000000000, 1.000000000000000000, -0.000000000000000000 ) ) ;
#7794 = ORIENTED_EDGE ( 'NONE', *, *, #40061, .T. ) ;
#7795 = AXIS2_PLACEMENT_3D ( 'NONE', #5757, #21504, #1878 ) ;
#7796 = ORIENTED_EDGE ( 'NONE', *, *, #10349, .F. ) ;
#7797 = VECTOR ( 'NONE', #4931, 39.37007874015748143 ) ;
#7798 = CARTESIAN_POINT ( 'NONE',  ( 2.164658444855302122, 5.905511811023623991, -0.04795272066889885720 ) ) ;
#7799 = ORIENTED_EDGE ( 'NONE', *, *, #50183, .F. ) ;
#7800 = CARTESIAN_POINT ( 'NONE',  ( 1.062992125984251635, 0.5905511811023621549, 1.181102362204724088 ) ) ;
#7801 = VECTOR ( 'NONE', #8699, 39.37007874015748143 ) ;
#7802 = ORIENTED_EDGE ( 'NONE', *, *, #1102, .T. ) ;
#7803 = VECTOR ( 'NONE', #1452, 39.37007874015748143 ) ;
#7804 = CARTESIAN_POINT ( 'NONE',  ( -1.129536109867572691, 1.599305403152165184, -2.458929368400313287 ) ) ;
#7805 = DIRECTION ( 'NONE',  ( -0.01601477604151182663, 0.9998717552508123996, -0.000000000000000000 ) ) ;
#7806 = CARTESIAN_POINT ( 'NONE',  ( -1.909347346926324462, 3.267716535433071279, 1.102362204724404160 ) ) ;
#7807 = VERTEX_POINT ( 'NONE', #14698 ) ;
#7808 = ORIENTED_EDGE ( 'NONE', *, *, #11920, .F. ) ;
#7809 = ORIENTED_EDGE ( 'NONE', *, *, #30209, .F. ) ;
#7810 = CARTESIAN_POINT ( 'NONE',  ( 0.000000000000000000, 3.267716535433071279, 0.000000000000000000 ) ) ;
#7811 = AXIS2_PLACEMENT_3D ( 'NONE', #24194, #39938, #28054 ) ;
#7812 = CARTESIAN_POINT ( 'NONE',  ( 1.363819533518803251, 3.346456692913386100, -0.6692913385826764205 ) ) ;
#7813 = ORIENTED_EDGE ( 'NONE', *, *, #13103, .T. ) ;
#7814 = ORIENTED_EDGE ( 'NONE', *, *, #42838, .F. ) ;
#7815 = CARTESIAN_POINT ( 'NONE',  ( 0.3673703023927838429, 0.000000000000000000, 1.932961348296883042 ) ) ;
#7816 = DIRECTION ( 'NONE',  ( 1.000000000000000000, 0.000000000000000000, 0.000000000000000000 ) ) ;
#7817 = CARTESIAN_POINT ( 'NONE',  ( -1.636583440222564301, 3.346456692913386100, -1.456692913385822186 ) ) ;
#7818 = ORIENTED_EDGE ( 'NONE', *, *, #8208, .F. ) ;
#7819 = VERTEX_POINT ( 'NONE', #19564 ) ;
#7820 = EDGE_CURVE ( 'NONE', #46097, #43386, #14215, .T. ) ;
#7821 = CARTESIAN_POINT ( 'NONE',  ( 2.021817418930639931, 3.267716535433071279, 0.5905511811023582691 ) ) ;
#7822 = CARTESIAN_POINT ( 'NONE',  ( 0.5455278134075212115, 3.267716535433071279, -9.463399047163220715E-17 ) ) ;
#7823 = LINE ( 'NONE', #8076, #50022 ) ;
#7824 = EDGE_CURVE ( 'NONE', #4657, #23441, #39194, .T. ) ;
#7825 = VERTEX_POINT ( 'NONE', #38205 ) ;
#7826 = CARTESIAN_POINT ( 'NONE',  ( -1.091055626815042645, 3.346456692913386100, -0.3149606299212593941 ) ) ;
#7827 = EDGE_CURVE ( 'NONE', #47028, #20197, #3834, .T. ) ;
#7828 = CARTESIAN_POINT ( 'NONE',  ( 0.4696143004045484348, 0.000000000000000000, 1.535433070866133898 ) ) ;
#7829 = ORIENTED_EDGE ( 'NONE', *, *, #38413, .T. ) ;
#7830 = CARTESIAN_POINT ( 'NONE',  ( 1.091055626815043311, 3.267716535433071279, 1.377952755905504256 ) ) ;
#7831 = ORIENTED_EDGE ( 'NONE', *, *, #34026, .F. ) ;
#7832 = ORIENTED_EDGE ( 'NONE', *, *, #23387, .F. ) ;
#7833 = CARTESIAN_POINT ( 'NONE',  ( -2.121469926805683137, 1.574803149606302854, -0.4337334748181708721 ) ) ;
#7834 = DIRECTION ( 'NONE',  ( 0.9998717552508121775, 0.01601477604151182663, 0.000000000000000000 ) ) ;
#7835 = CARTESIAN_POINT ( 'NONE',  ( 0.4696143004045478797, 3.267716535433071279, -0.03937007874015908959 ) ) ;
#7836 = CARTESIAN_POINT ( 'NONE',  ( -0.8182917201112817063, 3.267716535433071279, 1.419509857074483046E-16 ) ) ;
#7837 = CARTESIAN_POINT ( 'NONE',  ( 1.909347346926324684, 3.346456692913386100, 0.5905511811023582691 ) ) ;
#7838 = ORIENTED_EDGE ( 'NONE', *, *, #11258, .F. ) ;
#7839 = ORIENTED_EDGE ( 'NONE', *, *, #25427, .T. ) ;
#7840 = VECTOR ( 'NONE', #16005, 39.37007874015748143 ) ;
#7841 = VECTOR ( 'NONE', #50281, 39.37007874015748143 ) ;
#7842 = EDGE_CURVE ( 'NONE', #9971, #34006, #15701, .T. ) ;
#7843 = ORIENTED_EDGE ( 'NONE', *, *, #13485, .F. ) ;
#7844 = CARTESIAN_POINT ( 'NONE',  ( -0.2727639067037602172, 3.346456692913386100, 1.417322834645662777 ) ) ;
#7845 = DIRECTION ( 'NONE',  ( 0.01601477604151182663, -0.9998717552508123996, 0.000000000000000000 ) ) ;
#7846 = AXIS2_PLACEMENT_3D ( 'NONE', #29336, #45068, #33488 ) ;
#7847 = EDGE_CURVE ( 'NONE', #19800, #3259, #34332, .T. ) ;
#7848 = EDGE_CURVE ( 'NONE', #27397, #12593, #22694, .T. ) ;
#7849 = LINE ( 'NONE', #20738, #5440 ) ;
#7850 = DIRECTION ( 'NONE',  ( -0.000000000000000000, -1.000000000000000000, -0.000000000000000000 ) ) ;
#7851 = VECTOR ( 'NONE', #30359, 39.37007874015748143 ) ;
#7852 = ORIENTED_EDGE ( 'NONE', *, *, #49180, .T. ) ;
#7853 = ADVANCED_FACE ( 'NONE', ( #24478 ), #47151, .F. ) ;
#7854 = DIRECTION ( 'NONE',  ( -1.267583980596140612E-16, 1.000000000000000000, 2.300325776299552367E-17 ) ) ;
#7855 = ADVANCED_FACE ( 'NONE', ( #24221 ), #12343, .T. ) ;
#7856 = CARTESIAN_POINT ( 'NONE',  ( -2.159905143290286045, 6.692913385826772199, 0.1535224723189609897 ) ) ;
#7857 = ORIENTED_EDGE ( 'NONE', *, *, #35304, .F. ) ;
#7858 = LINE ( 'NONE', #36253, #40547 ) ;
#7859 = CARTESIAN_POINT ( 'NONE',  ( -1.909347346926324462, 3.346456692913386100, 0.4724409448818871482 ) ) ;
#7860 = ORIENTED_EDGE ( 'NONE', *, *, #48881, .T. ) ;
#7861 = DIRECTION ( 'NONE',  ( 0.000000000000000000, 0.000000000000000000, 1.000000000000000000 ) ) ;
#7862 = DIRECTION ( 'NONE',  ( 1.000000000000000000, 0.000000000000000000, -3.469446951953613696E-16 ) ) ;
#7863 = CARTESIAN_POINT ( 'NONE',  ( -0.8942052331142551491, 3.267716535433071279, 3.102397620449222974E-16 ) ) ;
#7864 = EDGE_LOOP ( 'NONE', ( #16020, #39466 ) ) ;
#7865 = LINE ( 'NONE', #47318, #8183 ) ;
#7866 = VERTEX_POINT ( 'NONE', #11825 ) ;
#7867 = LINE ( 'NONE', #11241, #16307 ) ;
#7868 = PLANE ( 'NONE',  #23494 ) ;
#7869 = CARTESIAN_POINT ( 'NONE',  ( 1.243077785924837197, 0.8677437501918831009, -1.240380476265473098 ) ) ;
#7870 = ORIENTED_EDGE ( 'NONE', *, *, #3003, .F. ) ;
#7871 = ORIENTED_EDGE ( 'NONE', *, *, #39283, .T. ) ;
#7872 = DIRECTION ( 'NONE',  ( -1.000000000000000000, -0.000000000000000000, -0.000000000000000000 ) ) ;
#7873 = VECTOR ( 'NONE', #38404, 39.37007874015748143 ) ;
#7874 = LINE ( 'NONE', #23621, #13926 ) ;
#7875 = AXIS2_PLACEMENT_3D ( 'NONE', #46814, #38607, #34233 ) ;
#7876 = ORIENTED_EDGE ( 'NONE', *, *, #9113, .T. ) ;
#7877 = DIRECTION ( 'NONE',  ( -3.469446951953613696E-16, 0.000000000000000000, -1.000000000000000000 ) ) ;
#7878 = FACE_OUTER_BOUND ( 'NONE', #50725, .T. ) ;
#7879 = CARTESIAN_POINT ( 'NONE',  ( -0.8942052331142552601, 3.346456692913386100, 1.889763779527550147 ) ) ;
#7880 = VECTOR ( 'NONE', #28946, 39.37007874015748143 ) ;
#7881 = DIRECTION ( 'NONE',  ( -0.000000000000000000, 0.000000000000000000, 1.000000000000000000 ) ) ;
#7882 = VERTEX_POINT ( 'NONE', #1234 ) ;
#7883 = ORIENTED_EDGE ( 'NONE', *, *, #19205, .T. ) ;
#7884 = PLANE ( 'NONE',  #5962 ) ;
#7885 = VECTOR ( 'NONE', #13989, 39.37007874015748143 ) ;
#7886 = DIRECTION ( 'NONE',  ( 1.734723475976806848E-16, -0.000000000000000000, 1.000000000000000000 ) ) ;
#7887 = EDGE_CURVE ( 'NONE', #34340, #30894, #47923, .T. ) ;
#7888 = VECTOR ( 'NONE', #34428, 39.37007874015748143 ) ;
#7889 = ORIENTED_EDGE ( 'NONE', *, *, #38149, .T. ) ;
#7890 = EDGE_CURVE ( 'NONE', #50120, #42995, #23959, .T. ) ;
#7891 = CARTESIAN_POINT ( 'NONE',  ( 2.539930011093434192, 1.755364253847478961, -1.032098760813036531 ) ) ;
#7892 = ORIENTED_EDGE ( 'NONE', *, *, #13702, .F. ) ;
#7893 = ORIENTED_EDGE ( 'NONE', *, *, #46858, .T. ) ;
#7894 = LINE ( 'NONE', #23637, #2798 ) ;
#7895 = EDGE_CURVE ( 'NONE', #40070, #3116, #39967, .T. ) ;
#7896 = ORIENTED_EDGE ( 'NONE', *, *, #13694, .F. ) ;
#7897 = ORIENTED_EDGE ( 'NONE', *, *, #19589, .T. ) ;
#7898 = CARTESIAN_POINT ( 'NONE',  ( 2.106333035502527373, 3.267716535433071279, 0.006892066987321476823 ) ) ;
#7899 = VERTEX_POINT ( 'NONE', #4338 ) ;
#7900 = FACE_OUTER_BOUND ( 'NONE', #36084, .T. ) ;
#7901 = LINE ( 'NONE', #4802, #44207 ) ;
#7902 = LINE ( 'NONE', #6458, #17651 ) ;
#7903 = EDGE_CURVE ( 'NONE', #3510, #46048, #13444, .T. ) ;
#7904 = DIRECTION ( 'NONE',  ( -1.000000000000000000, -0.000000000000000000, -0.000000000000000000 ) ) ;
#7905 = LINE ( 'NONE', #23654, #13782 ) ;
#7906 = CARTESIAN_POINT ( 'NONE',  ( 0.4001787029124908024, 1.205361022782829114E-17, 1.929553426015793605 ) ) ;
#7907 = VECTOR ( 'NONE', #9066, 39.37007874015748143 ) ;
#7908 = VERTEX_POINT ( 'NONE', #31456 ) ;
#7909 = CARTESIAN_POINT ( 'NONE',  ( -3.346456692913385211, 0.000000000000000000, -4.133858267716536083 ) ) ;
#7910 = AXIS2_PLACEMENT_3D ( 'NONE', #48128, #28282, #4546 ) ;
#7911 = EDGE_CURVE ( 'NONE', #4986, #13914, #12087, .T. ) ;
#7912 = DIRECTION ( 'NONE',  ( -0.000000000000000000, 1.000000000000000000, -0.000000000000000000 ) ) ;
#7913 = VECTOR ( 'NONE', #20898, 39.37007874015748143 ) ;
#7914 = CARTESIAN_POINT ( 'NONE',  ( 0.000000000000000000, 3.267716535433071279, -0.1968503937007883287 ) ) ;
#7915 = ORIENTED_EDGE ( 'NONE', *, *, #27459, .F. ) ;
#7916 = CARTESIAN_POINT ( 'NONE',  ( 4.821444091131312140E-17, 0.000000000000000000, 0.3937007874015748254 ) ) ;
#7917 = LINE ( 'NONE', #23662, #10459 ) ;
#7918 = ORIENTED_EDGE ( 'NONE', *, *, #7494, .F. ) ;
#7919 = CARTESIAN_POINT ( 'NONE',  ( 1.636583440222563635, 0.000000000000000000, -1.259842519685035800 ) ) ;
#7920 = VECTOR ( 'NONE', #25014, 39.37007874015748143 ) ;
#7921 = CARTESIAN_POINT ( 'NONE',  ( 2.882373499243445103, 1.448344807863587436, -0.6410611587410768308 ) ) ;
#7922 = CARTESIAN_POINT ( 'NONE',  ( 0.000000000000000000, 3.346456692913386100, 0.000000000000000000 ) ) ;
#7923 = CIRCLE ( 'NONE', #12054, 2.165354330708661568 ) ;
#7924 = LINE ( 'NONE', #47889, #39758 ) ;
#7925 = ORIENTED_EDGE ( 'NONE', *, *, #25100, .T. ) ;
#7926 = CARTESIAN_POINT ( 'NONE',  ( -0.8942052331142552601, 3.267716535433071279, 2.204724409448808764 ) ) ;
#7927 = CARTESIAN_POINT ( 'NONE',  ( 1.033334490728470723, 1.724452693827607908, -2.032317711754626277 ) ) ;
#7928 = CARTESIAN_POINT ( 'NONE',  ( 2.044241703397536636, 0.000000000000000000, -0.7159595814952622872 ) ) ;
#7929 = LINE ( 'NONE', #35556, #50650 ) ;
#7930 = VERTEX_POINT ( 'NONE', #44081 ) ;
#7931 = VERTEX_POINT ( 'NONE', #4857 ) ;
#7932 = ORIENTED_EDGE ( 'NONE', *, *, #28615, .F. ) ;
#7933 = DIRECTION ( 'NONE',  ( 0.9909497617679352555, 1.554141314384320336E-17, -0.1342332658176522420 ) ) ;
#7934 = VERTEX_POINT ( 'NONE', #36356 ) ;
#7935 = CARTESIAN_POINT ( 'NONE',  ( -0.3486774197067334380, 3.346456692913386100, 1.259842519685033357 ) ) ;
#7936 = DIRECTION ( 'NONE',  ( -0.000000000000000000, 0.000000000000000000, 1.000000000000000000 ) ) ;
#7937 = ORIENTED_EDGE ( 'NONE', *, *, #17240, .T. ) ;
#7938 = DIRECTION ( 'NONE',  ( 0.9749279121818259508, 0.000000000000000000, -0.2225209339563041788 ) ) ;
#7939 = ORIENTED_EDGE ( 'NONE', *, *, #4403, .F. ) ;
#7940 = DIRECTION ( 'NONE',  ( 0.000000000000000000, 0.000000000000000000, 1.000000000000000000 ) ) ;
#7941 = VECTOR ( 'NONE', #32897, 39.37007874015748143 ) ;
#7942 = DIRECTION ( 'NONE',  ( -1.000000000000000000, 0.000000000000000000, -0.000000000000000000 ) ) ;
#7943 = EDGE_CURVE ( 'NONE', #31137, #28697, #39677, .T. ) ;
#7944 = VECTOR ( 'NONE', #2000, 39.37007874015748143 ) ;
#7945 = ORIENTED_EDGE ( 'NONE', *, *, #22132, .F. ) ;
#7947 = ORIENTED_EDGE ( 'NONE', *, *, #2601, .F. ) ;
#7946 = EDGE_CURVE ( 'NONE', #16727, #33477, #43307, .T. ) ;
#7948 = VECTOR ( 'NONE', #18457, 39.37007874015748143 ) ;
#7949 = DIRECTION ( 'NONE',  ( 1.000000000000000000, 0.000000000000000000, 0.000000000000000000 ) ) ;
#7950 = VERTEX_POINT ( 'NONE', #16219 ) ;
#7951 = VECTOR ( 'NONE', #21802, 39.37007874015748143 ) ;
#7952 = EDGE_CURVE ( 'NONE', #2129, #43946, #17430, .T. ) ;
#7953 = DIRECTION ( 'NONE',  ( 1.000000000000000000, 0.000000000000000000, 0.000000000000000000 ) ) ;
#7954 = AXIS2_PLACEMENT_3D ( 'NONE', #29043, #41694, #45284 ) ;
#7956 = ORIENTED_EDGE ( 'NONE', *, *, #29980, .F. ) ;
#7955 = EDGE_CURVE ( 'NONE', #34623, #27824, #43818, .T. ) ;
#7957 = ORIENTED_EDGE ( 'NONE', *, *, #8082, .T. ) ;
#7958 = CARTESIAN_POINT ( 'NONE',  ( 0.000000000000000000, 0.000000000000000000, 0.000000000000000000 ) ) ;
#7959 = AXIS2_PLACEMENT_3D ( 'NONE', #7380, #11505, #42976 ) ;
#7960 = CARTESIAN_POINT ( 'NONE',  ( -1.181102362204724310, 0.000000000000000000, -1.181102362204724754 ) ) ;
#7961 = ORIENTED_EDGE ( 'NONE', *, *, #32530, .F. ) ;
#7962 = FACE_OUTER_BOUND ( 'NONE', #10402, .T. ) ;
#7963 = ORIENTED_EDGE ( 'NONE', *, *, #3746, .F. ) ;
#7964 = CARTESIAN_POINT ( 'NONE',  ( -1.439733046521777027, 0.000000000000000000, -1.456692913385822186 ) ) ;
#7965 = CARTESIAN_POINT ( 'NONE',  ( 0.7423782071083085965, 0.000000000000000000, -0.5118110236220467790 ) ) ;
#7966 = EDGE_CURVE ( 'NONE', #17533, #25678, #37220, .T. ) ;
#7967 = DIRECTION ( 'NONE',  ( 0.8345732537212999791, 0.000000000000000000, 0.5508969814521065267 ) ) ;
#7968 = ORIENTED_EDGE ( 'NONE', *, *, #48026, .T. ) ;
#7969 = ORIENTED_EDGE ( 'NONE', *, *, #9843, .T. ) ;
#7970 = LINE ( 'NONE', #4106, #36857 ) ;
#7971 = LINE ( 'NONE', #8230, #22054 ) ;
#7972 = CARTESIAN_POINT ( 'NONE',  ( 2.106197740627112402, 3.346456692913386100, 1.102362204724403938 ) ) ;
#7973 = EDGE_CURVE ( 'NONE', #14952, #41410, #5105, .T. ) ;
#7974 = DIRECTION ( 'NONE',  ( 1.000000000000000000, 0.000000000000000000, 0.000000000000000000 ) ) ;
#7975 = CARTESIAN_POINT ( 'NONE',  ( 0.002207914879453961969, 6.692913385826772199, 0.04916304461325451958 ) ) ;
#7976 = CARTESIAN_POINT ( 'NONE',  ( -1.909347346926324462, 3.346456692913386100, 0.1574803149606286423 ) ) ;
#7977 = ORIENTED_EDGE ( 'NONE', *, *, #44895, .F. ) ;
#7978 = AXIS2_PLACEMENT_3D ( 'NONE', #44042, #24183, #12821 ) ;
#7979 = CARTESIAN_POINT ( 'NONE',  ( 0.3303541855028671037, 0.3937007874015748254, 0.000000000000000000 ) ) ;
#7980 = DIMENSIONAL_EXPONENTS ( 1.000000000000000000, 0.000000000000000000, 0.000000000000000000, 0.000000000000000000, 0.000000000000000000, 0.000000000000000000, 0.000000000000000000 ) ;
#7981 = ORIENTED_EDGE ( 'NONE', *, *, #24462, .T. ) ;
#7982 = CIRCLE ( 'NONE', #47519, 2.106299212598425008 ) ;
#7983 = LINE ( 'NONE', #27086, #32490 ) ;
#7984 = VERTEX_POINT ( 'NONE', #48181 ) ;
#7985 = EDGE_CURVE ( 'NONE', #11918, #7241, #10334, .T. ) ;
#7986 = CARTESIAN_POINT ( 'NONE',  ( 0.1067246931122726866, 0.02962905676920215767, 0.000000000000000000 ) ) ;
#7987 = CARTESIAN_POINT ( 'NONE',  ( 0.5455278134075217666, 3.346456692913386100, 2.204724409448808764 ) ) ;
#7988 = VECTOR ( 'NONE', #24350, 39.37007874015748143 ) ;
#7989 = ORIENTED_EDGE ( 'NONE', *, *, #21926, .F. ) ;
#7990 = FACE_OUTER_BOUND ( 'NONE', #16358, .T. ) ;
#7991 = VERTEX_POINT ( 'NONE', #8982 ) ;
#7992 = DIRECTION ( 'NONE',  ( -1.000000000000000000, 0.000000000000000000, -0.000000000000000000 ) ) ;
#7993 = ORIENTED_EDGE ( 'NONE', *, *, #48676, .F. ) ;
#7994 = LINE ( 'NONE', #31493, #33486 ) ;
#7995 = PLANE ( 'NONE',  #852 ) ;
#7996 = ORIENTED_EDGE ( 'NONE', *, *, #4278, .F. ) ;
#7997 = CARTESIAN_POINT ( 'NONE',  ( 0.04921259842519667971, 1.708690180665275005, 2.244725876464058523 ) ) ;
#7998 = ORIENTED_EDGE ( 'NONE', *, *, #33732, .T. ) ;
#7999 = ORIENTED_EDGE ( 'NONE', *, *, #15303, .F. ) ;
#8000 = DIRECTION ( 'NONE',  ( 0.000000000000000000, 0.000000000000000000, -1.000000000000000000 ) ) ;
#8001 = CARTESIAN_POINT ( 'NONE',  ( -1.091055626815042645, 3.346456692913386100, -0.6299212598425177889 ) ) ;
#8002 = CARTESIAN_POINT ( 'NONE',  ( -2.168245791271168343, 1.587034731952809752, -2.004968704497279930 ) ) ;
#8003 = EDGE_CURVE ( 'NONE', #30012, #26738, #34851, .T. ) ;
#8004 = ORIENTED_EDGE ( 'NONE', *, *, #31857, .T. ) ;
#8005 = CARTESIAN_POINT ( 'NONE',  ( 2.121469926805689354, 6.692913385826772199, -0.4337334748181388422 ) ) ;
#8006 = CARTESIAN_POINT ( 'NONE',  ( 0.000000000000000000, 3.267716535433071279, 0.000000000000000000 ) ) ;
#8007 = EDGE_CURVE ( 'NONE', #50330, #3253, #31713, .T. ) ;
#8008 = VECTOR ( 'NONE', #21741, 39.37007874015748143 ) ;
#8009 = VECTOR ( 'NONE', #26153, 39.37007874015748143 ) ;
#8010 = EDGE_CURVE ( 'NONE', #38642, #37024, #20190, .T. ) ;
#8011 = EDGE_LOOP ( 'NONE', ( #11681, #13362, #343, #40459 ) ) ;
#8012 = CARTESIAN_POINT ( 'NONE',  ( -1.083598637574820334, 1.702374950942735499, 2.747180975113330259 ) ) ;
#8013 = VECTOR ( 'NONE', #16430, 39.37007874015748143 ) ;
#8014 = ORIENTED_EDGE ( 'NONE', *, *, #188, .F. ) ;
#8015 = ORIENTED_EDGE ( 'NONE', *, *, #30753, .F. ) ;
#8016 = CONTEXT_DEPENDENT_SHAPE_REPRESENTATION ( #8150, #20306 ) ;
#8017 = ORIENTED_EDGE ( 'NONE', *, *, #27428, .F. ) ;
#8018 = DIRECTION ( 'NONE',  ( 0.000000000000000000, 0.000000000000000000, 1.000000000000000000 ) ) ;
#8019 = CARTESIAN_POINT ( 'NONE',  ( -2.903572669614648660, 2.755905511811027164, 1.294565943894125715 ) ) ;
#8020 = EDGE_CURVE ( 'NONE', #3944, #39458, #34455, .T. ) ;
#8021 = CARTESIAN_POINT ( 'NONE',  ( 0.2430652128771959297, 1.574803149606302854, -2.151668812760857641 ) ) ;
#8022 = CARTESIAN_POINT ( 'NONE',  ( -1.057143431661237143, 3.267716535433071279, -1.889763779527552146 ) ) ;
#8023 = ORIENTED_EDGE ( 'NONE', *, *, #25009, .T. ) ;
#8024 = B_SPLINE_CURVE_WITH_KNOTS ( 'NONE', 3,
 ( #47310, #23857, #4235, #36507 ),
 .UNSPECIFIED., .F., .F.,
 ( 4, 4 ),
 ( 0.1211775127643062444, 0.1625894504277921315 ),
 .UNSPECIFIED. ) ;
#8025 = ORIENTED_EDGE ( 'NONE', *, *, #42509, .T. ) ;
#8026 = CARTESIAN_POINT ( 'NONE',  ( 1.929629134066521701, 5.118110236220475784, 0.9824921284572420976 ) ) ;
#8027 = CARTESIAN_POINT ( 'NONE',  ( 2.297395577996739213, 1.679082147652236845, 0.3608654278263103699 ) ) ;
#8028 = VECTOR ( 'NONE', #20740, 39.37007874015748143 ) ;
#8029 = VERTEX_POINT ( 'NONE', #46043 ) ;
#8030 = PLANE ( 'NONE',  #15244 ) ;
#8031 = CARTESIAN_POINT ( 'NONE',  ( 1.305557278495039775, 1.728812839972934334, -1.880670907523083191 ) ) ;
#8032 = EDGE_CURVE ( 'NONE', #7866, #30710, #26414, .T. ) ;
#8033 = CARTESIAN_POINT ( 'NONE',  ( 2.326943258702977246, 1.646747008850265370, -0.05524094006260020506 ) ) ;
#8034 = PLANE ( 'NONE',  #9574 ) ;
#8035 = CARTESIAN_POINT ( 'NONE',  ( 0.7090793742677682365, 0.03927686936677046714, 1.749277966691849429 ) ) ;
#8036 = ORIENTED_EDGE ( 'NONE', *, *, #11862, .F. ) ;
#8037 = FACE_OUTER_BOUND ( 'NONE', #16201, .T. ) ;
#8038 = LINE ( 'NONE', #27907, #20251 ) ;
#8039 = ORIENTED_EDGE ( 'NONE', *, *, #25325, .T. ) ;
#8040 = ADVANCED_FACE ( 'NONE', ( #42187 ), #37832, .F. ) ;
#8041 = EDGE_LOOP ( 'NONE', ( #24581, #25787, #15777, #34823 ) ) ;
#8042 = CARTESIAN_POINT ( 'NONE',  ( -0.04921259842519689481, -2.628659302178988761E-16, 2.213182383082910487 ) ) ;
#8043 = DIRECTION ( 'NONE',  ( -0.000000000000000000, 0.000000000000000000, 1.000000000000000000 ) ) ;
#8044 = CARTESIAN_POINT ( 'NONE',  ( -0.8942052331142547050, 0.000000000000000000, 0.3149606299212580063 ) ) ;
#8045 = AXIS2_PLACEMENT_3D ( 'NONE', #23353, #31369, #8381 ) ;
#8046 = VERTEX_POINT ( 'NONE', #18194 ) ;
#8047 = AXIS2_PLACEMENT_3D ( 'NONE', #5195, #36700, #36961 ) ;
#8048 = EDGE_CURVE ( 'NONE', #50385, #36720, #4199, .T. ) ;
#8049 = ORIENTED_EDGE ( 'NONE', *, *, #23122, .T. ) ;
#8050 = CARTESIAN_POINT ( 'NONE',  ( 0.2727639067037610499, 3.267716535433071279, 2.047244094488179567 ) ) ;
#8051 = AXIS2_PLACEMENT_3D ( 'NONE', #35893, #47718, #16265 ) ;
#8052 = EDGE_LOOP ( 'NONE', ( #6663, #22607, #35357, #23238, #48627, #37852, #44649, #43879, #23264, #23352, #36701, #27154, #40826, #39942, #10052, #4860, #22017, #7745, #46650, #24523, #18057, #9542, #39720, #22452, #3334, #17340, #8025, #14254, #3012, #42557, #21084, #30543, #36026, #13099, #7100, #41282, #19848, #44426, #30671, #43579, #24835, #32151, #1609, #36667, #13374, #11635, #193, #12040, #50655, #38572, #47450, #34740, #18928, #39539, #50559, #5847, #20745, #5992, #16831, #32355, #34050, #40578, #30168, #5316, #22450, #35771, #43490, #37623, #26101, #23010, #34926 ) ) ;
#8053 = CARTESIAN_POINT ( 'NONE',  ( 1.236813753895252166, 1.738537790538875027, -2.681693691597563767 ) ) ;
#8054 = ORIENTED_EDGE ( 'NONE', *, *, #47562, .T. ) ;
#8055 = EDGE_CURVE ( 'NONE', #4189, #25120, #25942, .T. ) ;
#8056 = LINE ( 'NONE', #27665, #12009 ) ;
#8057 = DIRECTION ( 'NONE',  ( 1.734723475976806848E-16, -0.000000000000000000, 1.000000000000000000 ) ) ;
#8058 = DIRECTION ( 'NONE',  ( -1.000000000000000000, 0.000000000000000000, -0.000000000000000000 ) ) ;
#8059 = AXIS2_PLACEMENT_3D ( 'NONE', #21430, #48496, #33317 ) ;
#8060 = VERTEX_POINT ( 'NONE', #38334 ) ;
#8061 = ORIENTED_EDGE ( 'NONE', *, *, #24349, .T. ) ;
#8062 = EDGE_LOOP ( 'NONE', ( #27589, #48368, #10518, #18589 ) ) ;
#8063 = CARTESIAN_POINT ( 'NONE',  ( 1.091055626815042645, 3.267716535433071279, -1.892679809432644882E-16 ) ) ;
#8064 = CARTESIAN_POINT ( 'NONE',  ( 1.363819533518803029, 3.267716535433071279, -1.732283464566923170 ) ) ;
#8065 = ORIENTED_EDGE ( 'NONE', *, *, #42297, .T. ) ;
#8066 = EDGE_LOOP ( 'NONE', ( #11629, #39282, #19670, #47003 ) ) ;
#8067 = CARTESIAN_POINT ( 'NONE',  ( -0.8615171516511902494, 0.5249316475426858419, -1.675535330858600291 ) ) ;
#8068 = CARTESIAN_POINT ( 'NONE',  ( 0.000000000000000000, 3.267716535433071279, 2.204724409448808764 ) ) ;
#8069 = CARTESIAN_POINT ( 'NONE',  ( 0.8182917201112819283, 3.346456692913386100, 1.102362204724403938 ) ) ;
#8070 = AXIS2_PLACEMENT_3D ( 'NONE', #15840, #24876, #47810 ) ;
#8071 = EDGE_CURVE ( 'NONE', #46953, #1801, #38080, .T. ) ;
#8072 = ORIENTED_EDGE ( 'NONE', *, *, #35, .F. ) ;
#8073 = ORIENTED_EDGE ( 'NONE', *, *, #49907, .T. ) ;
#8074 = CARTESIAN_POINT ( 'NONE',  ( -0.04921259842519706829, 1.516406576848131849, 2.952755905511811108 ) ) ;
#8075 = LINE ( 'NONE', #7822, #19185 ) ;
#8076 = CARTESIAN_POINT ( 'NONE',  ( -0.3486774197067340486, 0.000000000000000000, -0.1968503937007883287 ) ) ;
#8077 = ADVANCED_FACE ( 'NONE', ( #30070 ), #7085, .F. ) ;
#8078 = ADVANCED_FACE ( 'NONE', ( #22831 ), #29815, .F. ) ;
#8079 = ORIENTED_EDGE ( 'NONE', *, *, #2784, .F. ) ;
#8080 = CARTESIAN_POINT ( 'NONE',  ( 0.07982360342473591996, 1.709180471932028711, 0.000000000000000000 ) ) ;
#8081 = ORIENTED_EDGE ( 'NONE', *, *, #26701, .F. ) ;
#8082 = EDGE_CURVE ( 'NONE', #49027, #10066, #45787, .T. ) ;
#8083 = CARTESIAN_POINT ( 'NONE',  ( -0.6214413264104945434, 3.346456692913386100, -1.299212598425193210 ) ) ;
#8084 = ORIENTED_EDGE ( 'NONE', *, *, #34914, .F. ) ;
#8085 = ORIENTED_EDGE ( 'NONE', *, *, #28181, .F. ) ;
#8086 = DIRECTION ( 'NONE',  ( -0.9998717552508122886, -0.01601477604151181275, 0.000000000000000000 ) ) ;
#8087 = CARTESIAN_POINT ( 'NONE',  ( 0.7381027496705269142, 1.205361022782829114E-17, -2.859439394060913298 ) ) ;
#8088 = CARTESIAN_POINT ( 'NONE',  ( -1.166969139818016643, 3.267716535433071279, 4.048737525165548620E-16 ) ) ;
#8089 = VECTOR ( 'NONE', #22426, 39.37007874015748854 ) ;
#8090 = CARTESIAN_POINT ( 'NONE',  ( 1.363819533518803695, 0.000000000000000000, 1.535433070866133898 ) ) ;
#8091 = LINE ( 'NONE', #46297, #3235 ) ;
#8092 = ORIENTED_EDGE ( 'NONE', *, *, #28651, .T. ) ;
#8093 = EDGE_LOOP ( 'NONE', ( #42746, #22562, #2330, #43246 ) ) ;
#8094 = VECTOR ( 'NONE', #8852, 39.37007874015748143 ) ;
#8095 = VERTEX_POINT ( 'NONE', #9233 ) ;
#8096 = CARTESIAN_POINT ( 'NONE',  ( -2.734482843737247038, 1.578211097029592169, -1.115254632218712016 ) ) ;
#8097 = CARTESIAN_POINT ( 'NONE',  ( -1.636583440222563635, 0.000000000000000000, 1.259842519685033357 ) ) ;
#8098 = CLOSED_SHELL ( 'NONE', ( #30526, #35131, #44291, #14092, #37450, #485 ) ) ;
#8099 = VECTOR ( 'NONE', #37983, 39.37007874015748143 ) ;
#8100 = ADVANCED_FACE ( 'NONE', ( #30578 ), #21115, .F. ) ;
#8101 = VECTOR ( 'NONE', #44338, 39.37007874015748143 ) ;
#8102 = FACE_OUTER_BOUND ( 'NONE', #45746, .T. ) ;
#8103 = DIRECTION ( 'NONE',  ( -1.000000000000000000, -0.000000000000000000, -0.000000000000000000 ) ) ;
#8104 = VERTEX_POINT ( 'NONE', #22073 ) ;
#8105 = CARTESIAN_POINT ( 'NONE',  ( 2.106197740627112402, 3.346456692913386100, -0.02067487291359444701 ) ) ;
#8106 = VECTOR ( 'NONE', #41638, 39.37007874015748143 ) ;
#8107 = DIRECTION ( 'NONE',  ( -6.104789737168205836E-17, 1.000000000000000000, 1.134460028949762747E-16 ) ) ;
#8108 = EDGE_CURVE ( 'NONE', #12124, #24792, #34205, .T. ) ;
#8109 = ORIENTED_EDGE ( 'NONE', *, *, #23002, .F. ) ;
#8110 = FACE_OUTER_BOUND ( 'NONE', #30275, .T. ) ;
#8111 = EDGE_CURVE ( 'NONE', #36377, #29102, #49891, .T. ) ;
#8112 = CARTESIAN_POINT ( 'NONE',  ( 1.785720468602152611, 1.739985735216158291, -1.775410119839885059 ) ) ;
#8113 = CARTESIAN_POINT ( 'NONE',  ( -1.363819533518803473, 0.000000000000000000, 1.850393700787392293 ) ) ;
#8115 = EDGE_CURVE ( 'NONE', #17096, #25478, #38581, .T. ) ;
#8114 = VERTEX_POINT ( 'NONE', #28851 ) ;
#8116 = CARTESIAN_POINT ( 'NONE',  ( -1.735275627622573369, 1.647299937921974822, 1.320890859436214981 ) ) ;
#8117 = CARTESIAN_POINT ( 'NONE',  ( -1.985260859929297572, 3.346456692913386100, 0.6299212598425164567 ) ) ;
#8118 = DIRECTION ( 'NONE',  ( 0.000000000000000000, 0.000000000000000000, 1.000000000000000000 ) ) ;
#8119 = ORIENTED_EDGE ( 'NONE', *, *, #31265, .F. ) ;
#8120 = CARTESIAN_POINT ( 'NONE',  ( 0.2727639067037604947, 0.000000000000000000, 0.7874015748031454320 ) ) ;
#8121 = CYLINDRICAL_SURFACE ( 'NONE', #10101, 2.165354330708661568 ) ;
#8122 = ORIENTED_EDGE ( 'NONE', *, *, #19872, .F. ) ;
#8123 = PLANE ( 'NONE',  #37773 ) ;
#8124 = LINE ( 'NONE', #48091, #5346 ) ;
#8125 = PLANE ( 'NONE',  #32977 ) ;
#8126 = CARTESIAN_POINT ( 'NONE',  ( 2.100227814008711391, 1.205361022782829114E-17, -2.076109931251913565 ) ) ;
#8127 = VECTOR ( 'NONE', #40653, 39.37007874015748143 ) ;
#8128 = ORIENTED_EDGE ( 'NONE', *, *, #14437, .F. ) ;
#8129 = ORIENTED_EDGE ( 'NONE', *, *, #28104, .F. ) ;
#8130 = CARTESIAN_POINT ( 'NONE',  ( 1.636583440222563857, 3.267716535433071279, -0.5118110236220471121 ) ) ;
#8131 = LINE ( 'NONE', #23880, #36177 ) ;
#8132 = EDGE_LOOP ( 'NONE', ( #10456, #3479, #12842, #35760, #38257, #40095, #3558, #50362, #32166, #19210, #21526 ) ) ;
#8133 = LINE ( 'NONE', #4256, #14299 ) ;
#8134 = AXIS2_PLACEMENT_3D ( 'NONE', #503, #19345, #36907 ) ;
#8135 = DIRECTION ( 'NONE',  ( -0.1342332658176667026, 0.000000000000000000, 0.9909497617679331460 ) ) ;
#8136 = CARTESIAN_POINT ( 'NONE',  ( -1.405314191946755997, 1.685393272164901646, 1.683309666213049560 ) ) ;
#8137 = EDGE_CURVE ( 'NONE', #42344, #26476, #48431, .T. ) ;
#8138 = DIRECTION ( 'NONE',  ( 1.000000000000000000, -0.000000000000000000, 0.000000000000000000 ) ) ;
#8139 = AXIS2_PLACEMENT_3D ( 'NONE', #21230, #41614, #9863 ) ;
#8140 = VECTOR ( 'NONE', #16773, 39.37007874015748143 ) ;
#8141 = ORIENTED_EDGE ( 'NONE', *, *, #11180, .F. ) ;
#8142 = ORIENTED_EDGE ( 'NONE', *, *, #29445, .F. ) ;
#8143 = ORIENTED_EDGE ( 'NONE', *, *, #11830, .F. ) ;
#8144 = LINE ( 'NONE', #43492, #3495 ) ;
#8145 = CARTESIAN_POINT ( 'NONE',  ( 1.091055626815042645, 3.346456692913386100, -0.8267716535433055070 ) ) ;
#8146 = EDGE_CURVE ( 'NONE', #2168, #40155, #1488, .T. ) ;
#8147 = EDGE_CURVE ( 'NONE', #16522, #2113, #36861, .T. ) ;
#8148 = VECTOR ( 'NONE', #17439, 39.37007874015748143 ) ;
#8149 = CARTESIAN_POINT ( 'NONE',  ( -1.909347346926324906, 3.346456692913386100, -0.7874015748031470974 ) ) ;
#8150 =( REPRESENTATION_RELATIONSHIP ('NONE','NONE', #50198, #15265 ) REPRESENTATION_RELATIONSHIP_WITH_TRANSFORMATION ( #12399 )SHAPE_REPRESENTATION_RELATIONSHIP( ) );
#8151 = FACE_BOUND ( 'NONE', #42238, .T. ) ;
#8152 = VERTEX_POINT ( 'NONE', #7835 ) ;
#8153 = EDGE_CURVE ( 'NONE', #8620, #27696, #36305, .T. ) ;
#8154 = CARTESIAN_POINT ( 'NONE',  ( 2.106197740627112402, 3.267716535433071279, -0.02067487291359444701 ) ) ;
#8155 = ORIENTED_EDGE ( 'NONE', *, *, #17879, .F. ) ;
#8156 = EDGE_LOOP ( 'NONE', ( #49636, #14082, #38758, #11857, #37984, #33506, #14864, #27441, #41258, #2119, #24412, #4726, #43380 ) ) ;
#8157 = VECTOR ( 'NONE', #42267, 39.37007874015748143 ) ;
#8158 = CARTESIAN_POINT ( 'NONE',  ( 1.636583440222563857, 3.267716535433071279, 0.9448818897637746295 ) ) ;
#8159 = ORIENTED_EDGE ( 'NONE', *, *, #30582, .F. ) ;
#8160 = ORIENTED_EDGE ( 'NONE', *, *, #50307, .T. ) ;
#8161 = DIRECTION ( 'NONE',  ( 1.000000000000000000, 0.000000000000000000, 0.000000000000000000 ) ) ;
#8162 = ORIENTED_EDGE ( 'NONE', *, *, #1010, .T. ) ;
#8163 = LINE ( 'NONE', #20803, #45190 ) ;
#8164 = DIRECTION ( 'NONE',  ( -1.000000000000000000, -1.908195823574487557E-16, 0.000000000000000000 ) ) ;
#8165 = CARTESIAN_POINT ( 'NONE',  ( 0.08139965876239094178, 1.610780518492231694, 0.000000000000000000 ) ) ;
#8166 = CONICAL_SURFACE ( 'NONE', #14764, 2.165354330708661568, 0.2617993877991570129 ) ;
#8167 = DIRECTION ( 'NONE',  ( -3.469446951953613696E-16, 0.000000000000000000, -1.000000000000000000 ) ) ;
#8168 = LINE ( 'NONE', #44293, #17905 ) ;
#8169 = CARTESIAN_POINT ( 'NONE',  ( -1.062992125984251635, 0.4235180831842794702, 1.014069264286641570 ) ) ;
#8170 = ORIENTED_EDGE ( 'NONE', *, *, #3647, .T. ) ;
#8171 = DIRECTION ( 'NONE',  ( -0.000000000000000000, 0.000000000000000000, 1.000000000000000000 ) ) ;
#8172 = LINE ( 'NONE', #39664, #44932 ) ;
#8173 = DIRECTION ( 'NONE',  ( 0.3930250316539147803, -1.067483894049308527E-16, 0.9195277725514544587 ) ) ;
#8174 = VECTOR ( 'NONE', #1087, 39.37007874015748143 ) ;
#8175 = AXIS2_PLACEMENT_3D ( 'NONE', #38831, #31592, #14833 ) ;
#8176 = ORIENTED_EDGE ( 'NONE', *, *, #23901, .F. ) ;
#8177 = DIRECTION ( 'NONE',  ( 0.000000000000000000, 0.000000000000000000, -1.000000000000000000 ) ) ;
#8178 = EDGE_CURVE ( 'NONE', #7571, #10927, #34957, .T. ) ;
#8179 = DIRECTION ( 'NONE',  ( -0.000000000000000000, 1.000000000000000000, -0.000000000000000000 ) ) ;
#8180 = ORIENTED_EDGE ( 'NONE', *, *, #13908, .T. ) ;
#8181 = DIRECTION ( 'NONE',  ( -0.000000000000000000, 1.000000000000000000, -0.000000000000000000 ) ) ;
#8182 = FACE_OUTER_BOUND ( 'NONE', #39609, .T. ) ;
#8183 = VECTOR ( 'NONE', #883, 39.37007874015748143 ) ;
#8184 = EDGE_CURVE ( 'NONE', #36555, #26915, #27447, .T. ) ;
#8185 = CARTESIAN_POINT ( 'NONE',  ( 1.833433833923351353, 3.346456692913386100, 0.9448818897637746295 ) ) ;
#8186 = CARTESIAN_POINT ( 'NONE',  ( 0.8182917201112819283, 3.346456692913386100, 0.7874015748031454320 ) ) ;
#8187 = AXIS2_PLACEMENT_3D ( 'NONE', #6020, #25643, #33155 ) ;
#8188 = B_SPLINE_CURVE_WITH_KNOTS ( 'NONE', 3,
 ( #35839, #39710, #36098, #16478 ),
 .UNSPECIFIED., .F., .F.,
 ( 4, 4 ),
 ( 6.555779620287635616E-07, 0.004917953202330906451 ),
 .UNSPECIFIED. ) ;
#8189 = ORIENTED_EDGE ( 'NONE', *, *, #38275, .T. ) ;
#8190 = DIRECTION ( 'NONE',  ( -0.01601477604151182663, 0.9998717552508123996, -0.000000000000000000 ) ) ;
#8191 = DIRECTION ( 'NONE',  ( -0.9998717552508122886, -0.01601477604151185785, 0.000000000000000000 ) ) ;
#8192 = DIRECTION ( 'NONE',  ( -0.01601477604151182663, 0.9998717552508123996, -0.000000000000000000 ) ) ;
#8193 = DIRECTION ( 'NONE',  ( 1.734723475976806848E-16, 0.000000000000000000, 1.000000000000000000 ) ) ;
#8194 = ORIENTED_EDGE ( 'NONE', *, *, #7538, .F. ) ;
#8195 = VERTEX_POINT ( 'NONE', #27195 ) ;
#8196 = ORIENTED_EDGE ( 'NONE', *, *, #30976, .T. ) ;
#8197 = CARTESIAN_POINT ( 'NONE',  ( 2.152441353505198940, 5.905511811023623991, -0.2419059403264807173 ) ) ;
#8198 = VERTEX_POINT ( 'NONE', #35712 ) ;
#8199 = DIRECTION ( 'NONE',  ( -1.000000000000000000, 0.000000000000000000, 0.000000000000000000 ) ) ;
#8200 = EDGE_CURVE ( 'NONE', #35993, #5779, #31357, .T. ) ;
#8201 = LINE ( 'NONE', #449, #32684 ) ;
#8202 = ORIENTED_EDGE ( 'NONE', *, *, #23994, .T. ) ;
#8203 = LINE ( 'NONE', #35064, #41288 ) ;
#8204 = EDGE_CURVE ( 'NONE', #37100, #27093, #11210, .T. ) ;
#8205 = VECTOR ( 'NONE', #6743, 39.37007874015748143 ) ;
#8206 = ORIENTED_EDGE ( 'NONE', *, *, #31071, .F. ) ;
#8207 = CARTESIAN_POINT ( 'NONE',  ( -1.613060539954027872, 1.682065834201676324, -1.474157253483306507 ) ) ;
#8208 = EDGE_CURVE ( 'NONE', #1491, #33429, #50389, .T. ) ;
#8209 = CARTESIAN_POINT ( 'NONE',  ( 0.000000000000000000, 3.267716535433071279, -1.299212598425193210 ) ) ;
#8210 = VERTEX_POINT ( 'NONE', #19196 ) ;
#8211 = EDGE_CURVE ( 'NONE', #28900, #739, #31337, .T. ) ;
#8212 = DIRECTION ( 'NONE',  ( -0.9998717552508121775, -0.01601477604151182316, 0.000000000000000000 ) ) ;
#8213 = ORIENTED_EDGE ( 'NONE', *, *, #27994, .T. ) ;
#8214 = AXIS2_PLACEMENT_3D ( 'NONE', #7519, #38765, #19631 ) ;
#8215 = DIRECTION ( 'NONE',  ( 0.000000000000000000, -1.000000000000000000, 0.000000000000000000 ) ) ;
#8216 = VERTEX_POINT ( 'NONE', #4213 ) ;
#8217 = ORIENTED_EDGE ( 'NONE', *, *, #6799, .T. ) ;
#8218 = CARTESIAN_POINT ( 'NONE',  ( 0.000000000000000000, 3.346456692913386100, 0.000000000000000000 ) ) ;
#8219 = LINE ( 'NONE', #7960, #28664 ) ;
#8220 = VERTEX_POINT ( 'NONE', #46785 ) ;
#8221 = VECTOR ( 'NONE', #37034, 39.37007874015748143 ) ;
#8222 = PLANE ( 'NONE',  #43543 ) ;
#8223 = ORIENTED_EDGE ( 'NONE', *, *, #2265, .F. ) ;
#8224 = LINE ( 'NONE', #36360, #19474 ) ;
#8225 = LINE ( 'NONE', #16743, #38231 ) ;
#8226 = CARTESIAN_POINT ( 'NONE',  ( 0.4696143004045478242, 3.267716535433071279, -1.629301903132387013E-16 ) ) ;
#8227 = VERTEX_POINT ( 'NONE', #12218 ) ;
#8228 = ORIENTED_EDGE ( 'NONE', *, *, #41925, .F. ) ;
#8229 = CARTESIAN_POINT ( 'NONE',  ( -1.477797890860239383, 1.651423915540254361, 1.616677638457519883 ) ) ;
#8230 = CARTESIAN_POINT ( 'NONE',  ( 1.015142113812069757, 3.267716535433071279, -3.521981712565033375E-16 ) ) ;
#8231 = DIRECTION ( 'NONE',  ( -0.000000000000000000, 0.000000000000000000, 1.000000000000000000 ) ) ;
#8232 = CARTESIAN_POINT ( 'NONE',  ( 2.867773316779195447, 1.665472095473279790, -0.7050287376752005786 ) ) ;
#8233 = CARTESIAN_POINT ( 'NONE',  ( 2.823445274216730638, 5.118110236220475784, 0.8656477926280686797 ) ) ;
#8234 = CARTESIAN_POINT ( 'NONE',  ( 0.000000000000000000, 3.267716535433071279, -0.3543307086614178592 ) ) ;
#8235 = VECTOR ( 'NONE', #41425, 39.37007874015748143 ) ;
#8236 = EDGE_LOOP ( 'NONE', ( #49712, #36416, #7524, #42488 ) ) ;
#8237 = PLANE ( 'NONE',  #34976 ) ;
#8238 = ADVANCED_FACE ( 'NONE', ( #19700 ), #42934, .T. ) ;
#8239 = ORIENTED_EDGE ( 'NONE', *, *, #18132, .T. ) ;
#8240 = DIRECTION ( 'NONE',  ( 1.734723475976806848E-16, -0.000000000000000000, 1.000000000000000000 ) ) ;
#8241 = EDGE_CURVE ( 'NONE', #31373, #18885, #35462, .T. ) ;
#8242 = EDGE_LOOP ( 'NONE', ( #46959, #14470, #27188, #6878 ) ) ;
#8243 = EDGE_CURVE ( 'NONE', #36726, #12169, #39587, .T. ) ;
#8244 = PLANE ( 'NONE',  #22589 ) ;
#8245 = VECTOR ( 'NONE', #20863, 39.37007874015748143 ) ;
#8246 = DIRECTION ( 'NONE',  ( 0.000000000000000000, -1.000000000000000000, 0.000000000000000000 ) ) ;
#8247 = VECTOR ( 'NONE', #10955, 39.37007874015748143 ) ;
#8248 = CARTESIAN_POINT ( 'NONE',  ( 0.4696143004045476577, 3.346456692913386100, -2.047244094488182231 ) ) ;
#8249 = VERTEX_POINT ( 'NONE', #35207 ) ;
#8250 = CARTESIAN_POINT ( 'NONE',  ( 1.236813753895252166, 1.487789312410982445, -2.681693691597563767 ) ) ;
#8251 = ORIENTED_EDGE ( 'NONE', *, *, #4840, .F. ) ;
#8252 = LINE ( 'NONE', #35874, #17987 ) ;
#8253 = AXIS2_PLACEMENT_3D ( 'NONE', #23543, #20442, #823 ) ;
#8254 = VERTEX_POINT ( 'NONE', #43692 ) ;
#8255 = CARTESIAN_POINT ( 'NONE',  ( 0.5455278134075217666, 0.000000000000000000, 1.574803149606291974 ) ) ;
#8256 = CARTESIAN_POINT ( 'NONE',  ( -1.091055626815043089, 3.267716535433071279, 1.892679809432645376E-16 ) ) ;
#8257 = ADVANCED_FACE ( 'NONE', ( #15826 ), #47031, .T. ) ;
#8258 = DIRECTION ( 'NONE',  ( 1.160706738777443955E-16, 1.000000000000000000, -5.589669052740684758E-17 ) ) ;
#8259 = EDGE_LOOP ( 'NONE', ( #48408, #16044, #26021, #38677 ) ) ;
#8260 = EDGE_LOOP ( 'NONE', ( #18045, #38130, #20351, #7682 ) ) ;
#8261 = EDGE_CURVE ( 'NONE', #28015, #16004, #3711, .T. ) ;
#8262 = LINE ( 'NONE', #47460, #34247 ) ;
#8263 = CARTESIAN_POINT ( 'NONE',  ( 1.833433833923351353, 3.346456692913386100, -1.161035397307311917E-15 ) ) ;
#8264 = CARTESIAN_POINT ( 'NONE',  ( 1.015142113812069091, 3.346456692913386100, -1.929133858267711110 ) ) ;
#8265 = ORIENTED_EDGE ( 'NONE', *, *, #8115, .T. ) ;
#8266 = LINE ( 'NONE', #8005, #38589 ) ;
#8267 = CARTESIAN_POINT ( 'NONE',  ( 2.378961647330872786, 3.346456692913386100, -0.3149606299212596716 ) ) ;
#8268 = ORIENTED_EDGE ( 'NONE', *, *, #2538, .T. ) ;
#8269 = CARTESIAN_POINT ( 'NONE',  ( 1.598711713508005339, 5.905511811023623991, -1.460438370699377986 ) ) ;
#8270 = EDGE_LOOP ( 'NONE', ( #44960, #16277, #19900, #18913 ) ) ;
#8271 = ORIENTED_EDGE ( 'NONE', *, *, #47454, .F. ) ;
#8272 = CONTEXT_DEPENDENT_SHAPE_REPRESENTATION ( #3848, #944 ) ;
#8273 = EDGE_CURVE ( 'NONE', #33135, #8060, #43443, .T. ) ;
#8274 = ORIENTED_EDGE ( 'NONE', *, *, #19445, .T. ) ;
#8275 = LINE ( 'NONE', #21181, #48172 ) ;
#8276 = AXIS2_PLACEMENT_3D ( 'NONE', #33204, #5823, #5570 ) ;
#8277 = CARTESIAN_POINT ( 'NONE',  ( 0.000000000000000000, 6.692913385826772199, 0.000000000000000000 ) ) ;
#8278 = VECTOR ( 'NONE', #24588, 39.37007874015748143 ) ;
#8279 = CARTESIAN_POINT ( 'NONE',  ( -2.182111253630085734, 3.346456692913386100, -0.6299212598425177889 ) ) ;
#8280 = DIRECTION ( 'NONE',  ( 1.042246309068005903E-16, 1.000000000000000000, -7.572362681945165783E-17 ) ) ;
#8281 = EDGE_LOOP ( 'NONE', ( #10555, #14334, #1381, #43874 ) ) ;
#8282 = EDGE_LOOP ( 'NONE', ( #26342, #15270, #20596, #8983 ) ) ;
#8283 = PLANE ( 'NONE',  #14743 ) ;
#8284 = DIRECTION ( 'NONE',  ( -1.118904554427325505E-16, -1.000000000000000000, 3.087980359898369198E-17 ) ) ;
#8285 = AXIS2_PLACEMENT_3D ( 'NONE', #27045, #42547, #19049 ) ;
#8286 = EDGE_LOOP ( 'NONE', ( #35499, #50782, #4758, #37635 ) ) ;
#8287 = CARTESIAN_POINT ( 'NONE',  ( 1.560669927219591191, 3.267716535433071279, 1.535433070866133898 ) ) ;
#8288 = DIRECTION ( 'NONE',  ( 1.000000000000000000, -0.000000000000000000, 0.000000000000000000 ) ) ;
#8289 = CARTESIAN_POINT ( 'NONE',  ( -1.636583440222564301, 3.346456692913386100, -1.574803149606293307 ) ) ;
#8290 = DIRECTION ( 'NONE',  ( 1.000000000000000000, 0.000000000000000000, 0.000000000000000000 ) ) ;
#8291 = LINE ( 'NONE', #29645, #38474 ) ;
#8292 = ORIENTED_EDGE ( 'NONE', *, *, #25337, .T. ) ;
#8293 = FACE_OUTER_BOUND ( 'NONE', #13684, .T. ) ;
#8294 = ADVANCED_FACE ( 'NONE', ( #15083 ), #20627, .T. ) ;
#8295 = ORIENTED_EDGE ( 'NONE', *, *, #20272, .T. ) ;
#8296 = EDGE_CURVE ( 'NONE', #29864, #34114, #41247, .T. ) ;
#8297 = ORIENTED_EDGE ( 'NONE', *, *, #46727, .T. ) ;
#8298 = DIRECTION ( 'NONE',  ( -3.469446951953613696E-16, 0.000000000000000000, -1.000000000000000000 ) ) ;
#8299 = DIRECTION ( 'NONE',  ( 1.000000000000000000, 0.000000000000000000, 0.000000000000000000 ) ) ;
#8300 = LINE ( 'NONE', #20162, #35417 ) ;
#8301 = ADVANCED_FACE ( 'NONE', ( #48056 ), #13497, .F. ) ;
#8302 = VERTEX_POINT ( 'NONE', #36231 ) ;
#8303 = ADVANCED_FACE ( 'NONE', ( #1101 ), #13246, .F. ) ;
#8304 = EDGE_LOOP ( 'NONE', ( #16043, #6568, #8557, #46945 ) ) ;
#8305 = PLANE ( 'NONE',  #17183 ) ;
#8306 = ORIENTED_EDGE ( 'NONE', *, *, #11546, .F. ) ;
#8307 = DIRECTION ( 'NONE',  ( -0.01601477604151182663, 0.9998717552508123996, -0.000000000000000000 ) ) ;
#8308 = VERTEX_POINT ( 'NONE', #8856 ) ;
#8309 = CIRCLE ( 'NONE', #40498, 2.164630168518208109 ) ;
#8310 = DIRECTION ( 'NONE',  ( -1.000000000000000000, 0.000000000000000000, 1.734723475976806848E-16 ) ) ;
#8311 = FACE_OUTER_BOUND ( 'NONE', #1082, .T. ) ;
#8312 = PLANE ( 'NONE',  #21944 ) ;
#8313 = VECTOR ( 'NONE', #1478, 39.37007874015748143 ) ;
#8314 = EDGE_CURVE ( 'NONE', #25218, #26467, #841, .T. ) ;
#8315 = ORIENTED_EDGE ( 'NONE', *, *, #31170, .T. ) ;
#8316 = B_SPLINE_CURVE_WITH_KNOTS ( 'NONE', 3,
 ( #47511, #8568, #11429, #36201 ),
 .UNSPECIFIED., .F., .F.,
 ( 4, 4 ),
 ( 2.657285469857138443E-07, 0.002500653588094312214 ),
 .UNSPECIFIED. ) ;
#8317 = VERTEX_POINT ( 'NONE', #4472 ) ;
#8318 = ORIENTED_EDGE ( 'NONE', *, *, #49103, .T. ) ;
#8319 = CARTESIAN_POINT ( 'NONE',  ( -0.9914495361339010771, 1.205361022782829114E-17, 2.781765111341808705 ) ) ;
#8320 = FACE_OUTER_BOUND ( 'NONE', #13981, .T. ) ;
#8321 = EDGE_LOOP ( 'NONE', ( #33182, #37567 ) ) ;
#8322 = ORIENTED_EDGE ( 'NONE', *, *, #13328, .T. ) ;
#8323 = EDGE_CURVE ( 'NONE', #23316, #7708, #49157, .T. ) ;
#8324 = DIRECTION ( 'NONE',  ( 1.000000000000000000, 0.000000000000000000, 0.000000000000000000 ) ) ;
#8325 = CARTESIAN_POINT ( 'NONE',  ( -0.6214413264104945434, 0.000000000000000000, 1.850393700787391849 ) ) ;
#8326 = VECTOR ( 'NONE', #34253, 39.37007874015748143 ) ;
#8327 = LINE ( 'NONE', #20453, #9630 ) ;
#8328 = VERTEX_POINT ( 'NONE', #35973 ) ;
#8329 = CARTESIAN_POINT ( 'NONE',  ( 1.909347346926324684, 0.000000000000000000, 0.9055118110236164419 ) ) ;
#8330 = SHAPE_REPRESENTATION ( 'Front Cover', ( #26741 ), #4483 ) ;
#8331 = FACE_OUTER_BOUND ( 'NONE', #29926, .T. ) ;
#8332 = EDGE_CURVE ( 'NONE', #13971, #36157, #32879, .T. ) ;
#8333 = FACE_OUTER_BOUND ( 'NONE', #45394, .T. ) ;
#8334 = ORIENTED_EDGE ( 'NONE', *, *, #724, .F. ) ;
#8335 = CARTESIAN_POINT ( 'NONE',  ( -2.139038182717881487, 1.575216142802386754, 0.3394144611327329364 ) ) ;
#8336 = CARTESIAN_POINT ( 'NONE',  ( -0.07591351300297340121, 3.346456692913386100, -0.03937007874015908959 ) ) ;
#8337 = ORIENTED_EDGE ( 'NONE', *, *, #259, .T. ) ;
#8338 = DIRECTION ( 'NONE',  ( -3.469446951953613696E-16, 0.000000000000000000, -1.000000000000000000 ) ) ;
#8339 = ORIENTED_EDGE ( 'NONE', *, *, #1199, .T. ) ;
#8340 = ORIENTED_EDGE ( 'NONE', *, *, #22432, .T. ) ;
#8341 = CARTESIAN_POINT ( 'NONE',  ( 1.833433833923351353, 3.267716535433071279, 0.6299212598425164567 ) ) ;
#8342 = CARTESIAN_POINT ( 'NONE',  ( -1.083598637574820334, 1.603934357758587614, 2.747180975113330259 ) ) ;
#8343 = EDGE_CURVE ( 'NONE', #14514, #36209, #17370, .T. ) ;
#8344 = DIRECTION ( 'NONE',  ( 0.000000000000000000, 0.000000000000000000, -1.000000000000000000 ) ) ;
#8345 = CARTESIAN_POINT ( 'NONE',  ( 0.3544269074453565982, 1.680770349861149038, 2.228666219274223259 ) ) ;
#8346 = DIRECTION ( 'NONE',  ( 1.734723475976806848E-16, 0.000000000000000000, 1.000000000000000000 ) ) ;
#8347 = EDGE_LOOP ( 'NONE', ( #23306, #42798, #25496, #35056 ) ) ;
#8348 = ORIENTED_EDGE ( 'NONE', *, *, #22840, .F. ) ;
#8349 = ADVANCED_FACE ( 'NONE', ( #9106 ), #25114, .F. ) ;
#8350 = PRODUCT ( 'Top Cover', 'Top Cover', '', ( #4399 ) ) ;
#8351 = VECTOR ( 'NONE', #20072, 39.37007874015748143 ) ;
#8352 = ORIENTED_EDGE ( 'NONE', *, *, #15012, .F. ) ;
#8353 = FACE_OUTER_BOUND ( 'NONE', #13137, .T. ) ;
#8354 = CARTESIAN_POINT ( 'NONE',  ( -1.037524086854360483, 0.000000000000000000, 2.764473043227569260 ) ) ;
#8355 = EDGE_CURVE ( 'NONE', #28387, #17641, #40100, .T. ) ;
#8356 = VECTOR ( 'NONE', #5576, 39.37007874015748143 ) ;
#8357=STYLED_ITEM('',(#51073),#6895);
#8358 = DIRECTION ( 'NONE',  ( -0.000000000000000000, 0.000000000000000000, 1.000000000000000000 ) ) ;
#8359 = PLANE ( 'NONE',  #12893 ) ;
#8361 = CARTESIAN_POINT ( 'NONE',  ( -2.074656761898998170, 5.905511811023623991, -0.6223516566630905578 ) ) ;
#8360 = AXIS2_PLACEMENT_3D ( 'NONE', #23360, #3749, #3498 ) ;
#8362 = ORIENTED_EDGE ( 'NONE', *, *, #18332, .F. ) ;
#8363 = DIRECTION ( 'NONE',  ( 1.000000000000000000, 0.000000000000000000, -3.469446951953613696E-16 ) ) ;
#8364 = VECTOR ( 'NONE', #32801, 39.37007874015748143 ) ;
#8365 = LINE ( 'NONE', #48072, #20775 ) ;
#8366 = EDGE_CURVE ( 'NONE', #1230, #7184, #14854, .T. ) ;
#8367 = ORIENTED_EDGE ( 'NONE', *, *, #7557, .T. ) ;
#8368 = VECTOR ( 'NONE', #22652, 39.37007874015748143 ) ;
#8369 = CARTESIAN_POINT ( 'NONE',  ( -1.439733046521777027, 3.267716535433071279, -0.5118110236220466680 ) ) ;
#8370 = CARTESIAN_POINT ( 'NONE',  ( 2.100227814008711835, 1.751990118145921649, -2.076109931251913565 ) ) ;
#8371 = CARTESIAN_POINT ( 'NONE',  ( -0.4532322590609024759, 0.000000000000000000, -1.827234353172969561 ) ) ;
#8372 = ORIENTED_EDGE ( 'NONE', *, *, #33980, .T. ) ;
#8373 = CARTESIAN_POINT ( 'NONE',  ( -1.613190494289090227, 1.049866565877818125, 1.223531214424602220 ) ) ;
#8374 = CARTESIAN_POINT ( 'NONE',  ( 2.113646359261424745, 1.643330668647667858, -0.9569352356128659753 ) ) ;
#8375 = ADVANCED_FACE ( 'NONE', ( #12729 ), #16867, .F. ) ;
#8376 = DIRECTION ( 'NONE',  ( -3.469446951953613696E-16, 0.000000000000000000, -1.000000000000000000 ) ) ;
#8377 = ORIENTED_EDGE ( 'NONE', *, *, #31867, .F. ) ;
#8378 = DIRECTION ( 'NONE',  ( 1.000000000000000000, 0.000000000000000000, 0.000000000000000000 ) ) ;
#8379 = CARTESIAN_POINT ( 'NONE',  ( 0.3136974817028393425, 1.625700591256411531, -2.936457595020219635 ) ) ;
#8380 = ORIENTED_EDGE ( 'NONE', *, *, #6091, .F. ) ;
#8381 = DIRECTION ( 'NONE',  ( -1.000000000000000000, 0.000000000000000000, -0.000000000000000000 ) ) ;
#8382 = CARTESIAN_POINT ( 'NONE',  ( -1.139874548450032332, 0.006507011016954251416, 1.379489548043156377 ) ) ;
#8383 = CARTESIAN_POINT ( 'NONE',  ( -1.363819533518803473, 0.000000000000000000, -1.732283464566922726 ) ) ;
#8384 = LINE ( 'NONE', #24128, #29310 ) ;
#8385 = ORIENTED_EDGE ( 'NONE', *, *, #14185, .F. ) ;
#8386 = EDGE_LOOP ( 'NONE', ( #32552, #44770, #478, #41189 ) ) ;
#8387 = DIRECTION ( 'NONE',  ( 1.776356839400250149E-14, 0.000000000000000000, 1.000000000000000000 ) ) ;
#8388 = CYLINDRICAL_SURFACE ( 'NONE', #41969, 2.165354330708661568 ) ;
#8389 = ORIENTED_EDGE ( 'NONE', *, *, #14958, .T. ) ;
#8390 = FACE_OUTER_BOUND ( 'NONE', #1680, .T. ) ;
#8391 = DIRECTION ( 'NONE',  ( 1.734723475976806848E-16, -0.000000000000000000, 1.000000000000000000 ) ) ;
#8392 = PLANE ( 'NONE',  #43394 ) ;
#8393 = VECTOR ( 'NONE', #40628, 39.37007874015748143 ) ;
#8394 = CARTESIAN_POINT ( 'NONE',  ( -0.8182917201112814842, 3.267716535433071279, 0.5905511811023582691 ) ) ;
#8395 = VERTEX_POINT ( 'NONE', #24858 ) ;
#8396 = AXIS2_PLACEMENT_3D ( 'NONE', #37820, #37564, #2447 ) ;
#8397 = ORIENTED_EDGE ( 'NONE', *, *, #2663, .T. ) ;
#8398 = DIRECTION ( 'NONE',  ( -1.000000000000000000, 0.000000000000000000, -0.000000000000000000 ) ) ;
#8399 = CARTESIAN_POINT ( 'NONE',  ( 0.000000000000000000, 3.346456692913386100, 0.000000000000000000 ) ) ;
#8400 = EDGE_CURVE ( 'NONE', #15891, #29593, #28461, .T. ) ;
#8401 = CARTESIAN_POINT ( 'NONE',  ( -0.7381027496704858359, 1.609316782724114825, -2.859439394060923512 ) ) ;
#8402 = LINE ( 'NONE', #655, #10858 ) ;
#8403 = VECTOR ( 'NONE', #4253, 39.37007874015748143 ) ;
#8404 = FACE_BOUND ( 'NONE', #32621, .T. ) ;
#8405 = ORIENTED_EDGE ( 'NONE', *, *, #14954, .T. ) ;
#8406 = DIRECTION ( 'NONE',  ( 0.000000000000000000, 1.000000000000000000, 0.000000000000000000 ) ) ;
#8407 = EDGE_LOOP ( 'NONE', ( #45369, #47611, #11434 ) ) ;
#8408 = AXIS2_PLACEMENT_3D ( 'NONE', #19558, #46652, #458 ) ;
#8409 = VERTEX_POINT ( 'NONE', #48566 ) ;
#8410 = DIRECTION ( 'NONE',  ( -4.561975526775602830E-17, -1.000000000000000000, -1.067327232801823148E-16 ) ) ;
#8411 = EDGE_CURVE ( 'NONE', #10925, #37629, #47782, .T. ) ;
#8412 = CONICAL_SURFACE ( 'NONE', #46305, 2.165354330708661568, 0.2617993877991570129 ) ;
#8413 = EDGE_CURVE ( 'NONE', #30219, #13738, #42871, .T. ) ;
#8414 = EDGE_CURVE ( 'NONE', #39500, #1960, #40861, .T. ) ;
#8415 = ORIENTED_EDGE ( 'NONE', *, *, #30886, .T. ) ;
#8416 = EDGE_LOOP ( 'NONE', ( #590, #23683, #47336, #13951 ) ) ;
#8417 = DIRECTION ( 'NONE',  ( 0.9998717552508121775, 0.01601477604151182663, 0.000000000000000000 ) ) ;
#8418 = ORIENTED_EDGE ( 'NONE', *, *, #42498, .T. ) ;
#8419 = EDGE_CURVE ( 'NONE', #22619, #37657, #28971, .T. ) ;
#8420 = PLANE ( 'NONE',  #41905 ) ;
#8421 = LINE ( 'NONE', #20547, #14518 ) ;
#8422 = DIRECTION ( 'NONE',  ( 1.000000000000000000, 0.000000000000000000, 0.000000000000000000 ) ) ;
#8423 = FACE_OUTER_BOUND ( 'NONE', #18140, .T. ) ;
#8424 = PLANE ( 'NONE',  #50814 ) ;
#8425 = CARTESIAN_POINT ( 'NONE',  ( -2.258024766633058622, 0.000000000000000000, -0.3543307086614173040 ) ) ;
#8426 = EDGE_LOOP ( 'NONE', ( #40229, #42066, #25234, #12585 ) ) ;
#8427 = LINE ( 'NONE', #20291, #40669 ) ;
#8428 = DIRECTION ( 'NONE',  ( -0.07365742419378766559, -0.000000000000000000, 0.9972836025229415702 ) ) ;
#8429 = CARTESIAN_POINT ( 'NONE',  ( 1.363819533518803029, 3.346456692913386100, -1.417322834645665219 ) ) ;
#8430 = EDGE_CURVE ( 'NONE', #36606, #50546, #5493, .T. ) ;
#8431 = ORIENTED_EDGE ( 'NONE', *, *, #43146, .F. ) ;
#8432 = DIRECTION ( 'NONE',  ( 0.9195277725514544587, 4.558310254684937226E-17, -0.3930250316539147803 ) ) ;
#8433 = CARTESIAN_POINT ( 'NONE',  ( 0.4696143004045478797, 0.000000000000000000, -0.9842519685039348154 ) ) ;
#8434 = ORIENTED_EDGE ( 'NONE', *, *, #40195, .F. ) ;
#8435 = CARTESIAN_POINT ( 'NONE',  ( -1.166969139818016199, 3.267716535433071279, 1.850393700787392293 ) ) ;
#8436 = DIRECTION ( 'NONE',  ( -0.000000000000000000, 1.000000000000000000, -0.000000000000000000 ) ) ;
#8437 = EDGE_CURVE ( 'NONE', #27664, #32071, #49824, .T. ) ;
#8438 = LINE ( 'NONE', #20567, #16924 ) ;
#8439 = VECTOR ( 'NONE', #39560, 39.37007874015748854 ) ;
#8440 = EDGE_CURVE ( 'NONE', #9489, #14486, #34140, .T. ) ;
#8441 = VECTOR ( 'NONE', #5042, 39.37007874015748143 ) ;
#8442 = DIRECTION ( 'NONE',  ( -0.000000000000000000, 1.000000000000000000, -0.000000000000000000 ) ) ;
#8443 = VERTEX_POINT ( 'NONE', #18379 ) ;
#8444 = LINE ( 'NONE', #35808, #28915 ) ;
#8445 = LINE ( 'NONE', #39936, #49778 ) ;
#8446 = VECTOR ( 'NONE', #45312, 39.37007874015748143 ) ;
#8447 = DIRECTION ( 'NONE',  ( 5.063291518729136385E-17, 1.000000000000000000, -1.184615939703115601E-16 ) ) ;
#8448 = CARTESIAN_POINT ( 'NONE',  ( 0.7423782071083092626, 3.267716535433071279, 1.259842519685033357 ) ) ;
#8449 = EDGE_CURVE ( 'NONE', #1768, #42073, #26127, .T. ) ;
#8450 = VERTEX_POINT ( 'NONE', #45973 ) ;
#8451 = ORIENTED_EDGE ( 'NONE', *, *, #6234, .F. ) ;
#8452 = DIRECTION ( 'NONE',  ( 1.734723475976806848E-16, -0.000000000000000000, 1.000000000000000000 ) ) ;
#8453 = ORIENTED_EDGE ( 'NONE', *, *, #7624, .T. ) ;
#8454 = PLANE ( 'NONE',  #16971 ) ;
#8455 = ORIENTED_EDGE ( 'NONE', *, *, #14625, .T. ) ;
#8456 = DIRECTION ( 'NONE',  ( -0.000000000000000000, 1.000000000000000000, -0.000000000000000000 ) ) ;
#8457 = EDGE_LOOP ( 'NONE', ( #35607, #29361, #26607, #24156 ) ) ;
#8458 = LINE ( 'NONE', #24206, #34820 ) ;
#8459 = CARTESIAN_POINT ( 'NONE',  ( 2.145573199460771630, 1.654219156693913284, -2.028682376382505481 ) ) ;
#8460 = EDGE_LOOP ( 'NONE', ( #32086, #7701, #47016, #38522, #45587, #36125, #8119, #45578, #45850, #37069, #10508 ) ) ;
#8461 = CARTESIAN_POINT ( 'NONE',  ( 0.07982360342473591996, 1.709180471932028711, 0.000000000000000000 ) ) ;
#8462 = VERTEX_POINT ( 'NONE', #33637 ) ;
#8463 = VECTOR ( 'NONE', #45400, 39.37007874015748143 ) ;
#8464 = CARTESIAN_POINT ( 'NONE',  ( 1.560669927219590303, 3.213780742542635238, -1.912925693120431481 ) ) ;
#8465 = EDGE_CURVE ( 'NONE', #40849, #6366, #5995, .T. ) ;
#8466 = EDGE_CURVE ( 'NONE', #50824, #32285, #37507, .T. ) ;
#8467 = ORIENTED_EDGE ( 'NONE', *, *, #46770, .F. ) ;
#8468 = ORIENTED_EDGE ( 'NONE', *, *, #18862, .T. ) ;
#8469 = CARTESIAN_POINT ( 'NONE',  ( 0.5455278134075212115, 0.000000000000000000, 0.3149606299212576177 ) ) ;
#8470 = ADVANCED_FACE ( 'NONE', ( #14511 ), #41878, .F. ) ;
#8471 = VECTOR ( 'NONE', #47083, 39.37007874015748143 ) ;
#8472 = CARTESIAN_POINT ( 'NONE',  ( -0.9914495361339010771, 1.205361022782829114E-17, 2.781765111341808705 ) ) ;
#8473 = ORIENTED_EDGE ( 'NONE', *, *, #2064, .F. ) ;
#8474 = AXIS2_PLACEMENT_3D ( 'NONE', #22005, #18125, #41621 ) ;
#8475 = CARTESIAN_POINT ( 'NONE',  ( 0.5455278134075208785, 3.346456692913386100, -1.771653543307081025 ) ) ;
#8476 = ORIENTED_EDGE ( 'NONE', *, *, #27531, .T. ) ;
#8477 = CARTESIAN_POINT ( 'NONE',  ( -0.5455278134075214336, 0.000000000000000000, -1.141732283464563791 ) ) ;
#8478 = VECTOR ( 'NONE', #29889, 39.37007874015748143 ) ;
#8479 = VECTOR ( 'NONE', #47992, 39.37007874015748854 ) ;
#8480 = PLANE ( 'NONE',  #47226 ) ;
#8481 = CARTESIAN_POINT ( 'NONE',  ( 0.5455278134075208785, 0.000000000000000000, -2.086614173228340086 ) ) ;
#8482 = ORIENTED_EDGE ( 'NONE', *, *, #32297, .T. ) ;
#8483 = VERTEX_POINT ( 'NONE', #49065 ) ;
#8484 = DIRECTION ( 'NONE',  ( -0.000000000000000000, 1.000000000000000000, -0.000000000000000000 ) ) ;
#8485 = CARTESIAN_POINT ( 'NONE',  ( 1.909347346926324684, 3.267716535433071279, -0.3543307086614178592 ) ) ;
#8486 = VECTOR ( 'NONE', #43262, 39.37007874015748143 ) ;
#8487 = LINE ( 'NONE', #36882, #29107 ) ;
#8488 = EDGE_CURVE ( 'NONE', #18819, #24456, #25618, .T. ) ;
#8489 = CARTESIAN_POINT ( 'NONE',  ( 1.018961996185594021, 0.04424020667788951949, 1.609505285524495344 ) ) ;
#8490 = CARTESIAN_POINT ( 'NONE',  ( -1.985260859929297572, 3.267716535433071279, 6.887757239314511260E-16 ) ) ;
#8491 = ADVANCED_FACE ( 'NONE', ( #45722 ), #8510, .T. ) ;
#8492 = FACE_OUTER_BOUND ( 'NONE', #42747, .T. ) ;
#8493 = ORIENTED_EDGE ( 'NONE', *, *, #38275, .F. ) ;
#8494 = DIRECTION ( 'NONE',  ( -0.000000000000000000, -1.000000000000000000, -0.000000000000000000 ) ) ;
#8495 = EDGE_CURVE ( 'NONE', #29934, #8220, #2125, .T. ) ;
#8496 = VERTEX_POINT ( 'NONE', #45466 ) ;
#8497 = DIRECTION ( 'NONE',  ( -3.981026654148627524E-17, 1.000000000000000000, 1.225234019452863932E-16 ) ) ;
#8498 = EDGE_CURVE ( 'NONE', #23569, #4582, #10125, .T. ) ;
#8499 = ORIENTED_EDGE ( 'NONE', *, *, #28777, .F. ) ;
#8500 = CARTESIAN_POINT ( 'NONE',  ( 0.7381027496705270252, 1.499047760149736952, -2.859439394060913298 ) ) ;
#8501 = DIRECTION ( 'NONE',  ( -1.000000000000000000, -0.000000000000000000, -0.000000000000000000 ) ) ;
#8502 = CARTESIAN_POINT ( 'NONE',  ( -1.909347346926324906, 3.267716535433071279, 3.312189666507128668E-16 ) ) ;
#8503 = VERTEX_POINT ( 'NONE', #38267 ) ;
#8504 = DIRECTION ( 'NONE',  ( -9.701723960855733411E-17, 1.000000000000000000, -8.476140964546406840E-17 ) ) ;
#8505 = VECTOR ( 'NONE', #20195, 39.37007874015748143 ) ;
#8506 = CARTESIAN_POINT ( 'NONE',  ( 2.252332422952718183, 1.743977176619643910, -0.5645583697864726691 ) ) ;
#8507 = ORIENTED_EDGE ( 'NONE', *, *, #8296, .T. ) ;
#8508 = LINE ( 'NONE', #16253, #40248 ) ;
#8509 = EDGE_LOOP ( 'NONE', ( #50853, #40651, #23512, #2282 ) ) ;
#8510 = CONICAL_SURFACE ( 'NONE', #10176, 2.165354330708661568, 0.2617993877991570129 ) ;
#8511 = CIRCLE ( 'NONE', #10985, 2.165354330708661568 ) ;
#8512 = DIRECTION ( 'NONE',  ( -1.000000000000000000, 0.000000000000000000, 1.734723475976806848E-16 ) ) ;
#8513 = DIRECTION ( 'NONE',  ( -0.9998717552508122886, -0.01601477604151185785, 0.000000000000000000 ) ) ;
#8514 = VECTOR ( 'NONE', #7854, 39.37007874015748143 ) ;
#8515 = CARTESIAN_POINT ( 'NONE',  ( 0.2727639067037609943, 0.000000000000000000, 1.535433070866133898 ) ) ;
#8516 = ORIENTED_EDGE ( 'NONE', *, *, #12609, .F. ) ;
#8517 = ORIENTED_EDGE ( 'NONE', *, *, #48486, .F. ) ;
#8518 = CARTESIAN_POINT ( 'NONE',  ( 1.091055626815043311, 3.346456692913386100, 1.889763779527550369 ) ) ;
#8519 = CARTESIAN_POINT ( 'NONE',  ( -2.454875160333845674, 3.346456692913386100, -0.3543307086614173040 ) ) ;
#8520 = FACE_OUTER_BOUND ( 'NONE', #42216, .T. ) ;
#8521 = LINE ( 'NONE', #28385, #42698 ) ;
#8522 = CARTESIAN_POINT ( 'NONE',  ( 1.051609096396380449, 0.4349011127721511549, 1.025452293874513199 ) ) ;
#8523 = ORIENTED_EDGE ( 'NONE', *, *, #38565, .T. ) ;
#8524 = CARTESIAN_POINT ( 'NONE',  ( -1.363819533518803473, 3.267716535433071279, -0.3543307086614174151 ) ) ;
#8525 = EDGE_CURVE ( 'NONE', #1230, #37126, #3266, .T. ) ;
#8526 = EDGE_CURVE ( 'NONE', #681, #31838, #25876, .T. ) ;
#8527 = ORIENTED_EDGE ( 'NONE', *, *, #28273, .T. ) ;
#8528 = EDGE_LOOP ( 'NONE', ( #44862, #14861, #1224, #44192 ) ) ;
#8529 = APPLICATION_PROTOCOL_DEFINITION ( 'draft international standard', 'automotive_design', 1998, #40795 ) ;
#8530 = EDGE_CURVE ( 'NONE', #41536, #5523, #22008, .T. ) ;
#8531 = ORIENTED_EDGE ( 'NONE', *, *, #12688, .T. ) ;
#8532 = DIRECTION ( 'NONE',  ( -0.9998717552508122886, -0.01601477604151180928, 0.000000000000000000 ) ) ;
#8533 = DIRECTION ( 'NONE',  ( -0.000000000000000000, -1.000000000000000000, -0.000000000000000000 ) ) ;
#8534 = CARTESIAN_POINT ( 'NONE',  ( -1.166969139818015533, 3.267716535433071279, 4.048737525165544183E-16 ) ) ;
#8535 = CARTESIAN_POINT ( 'NONE',  ( 0.8182917201112819283, 3.346456692913386100, -0.4724409448818889246 ) ) ;
#8536 = ORIENTED_EDGE ( 'NONE', *, *, #47037, .T. ) ;
#8537 = ORIENTED_EDGE ( 'NONE', *, *, #4290, .F. ) ;
#8538 = DIRECTION ( 'NONE',  ( -1.000000000000000000, 0.000000000000000000, 1.734723475976806848E-16 ) ) ;
#8539 = CARTESIAN_POINT ( 'NONE',  ( -1.166969139818015977, 0.000000000000000000, -1.102362204724405270 ) ) ;
#8540 = DIRECTION ( 'NONE',  ( 1.000000000000000000, 0.000000000000000000, 0.000000000000000000 ) ) ;
#8541 = AXIS2_PLACEMENT_3D ( 'NONE', #39424, #43537, #38917 ) ;
#8542 = VERTEX_POINT ( 'NONE', #6254 ) ;
#8543 = DIRECTION ( 'NONE',  ( -0.000000000000000000, 0.000000000000000000, 1.000000000000000000 ) ) ;
#8544 = AXIS2_PLACEMENT_3D ( 'NONE', #19991, #38868, #42732 ) ;
#8545 = FACE_OUTER_BOUND ( 'NONE', #10694, .T. ) ;
#8546 = VECTOR ( 'NONE', #26266, 39.37007874015748143 ) ;
#8547 = EDGE_CURVE ( 'NONE', #41687, #13480, #30513, .T. ) ;
#8548 = CARTESIAN_POINT ( 'NONE',  ( -1.363819533518803473, 3.346456692913386100, 1.535433070866133232 ) ) ;
#8549 = DIRECTION ( 'NONE',  ( 1.000000000000000000, -0.000000000000000000, 0.000000000000000000 ) ) ;
#8550 = LINE ( 'NONE', #11652, #25235 ) ;
#8551 = AXIS2_PLACEMENT_3D ( 'NONE', #11101, #15225, #42328 ) ;
#8552 = ORIENTED_EDGE ( 'NONE', *, *, #30856, .F. ) ;
#8553 = CARTESIAN_POINT ( 'NONE',  ( -1.531618802077458597, 0.5250564235503655253, -1.532464050950231194 ) ) ;
#8554 =( NAMED_UNIT ( * ) SI_UNIT ( $, .STERADIAN. ) SOLID_ANGLE_UNIT ( ) );
#8555 = EDGE_CURVE ( 'NONE', #14497, #15505, #18131, .T. ) ;
#8556 = VERTEX_POINT ( 'NONE', #5748 ) ;
#8557 = ORIENTED_EDGE ( 'NONE', *, *, #31699, .F. ) ;
#8558 = FACE_OUTER_BOUND ( 'NONE', #45663, .T. ) ;
#8559 = LINE ( 'NONE', #24309, #18785 ) ;
#8560 = CARTESIAN_POINT ( 'NONE',  ( -1.712496953225537633, 0.000000000000000000, -0.9842519685039344823 ) ) ;
#8561 = ORIENTED_EDGE ( 'NONE', *, *, #17495, .T. ) ;
#8562 = VERTEX_POINT ( 'NONE', #37254 ) ;
#8563 = DIRECTION ( 'NONE',  ( -0.5128992774058949156, 0.000000000000000000, -0.8584487936018728726 ) ) ;
#8564 = ORIENTED_EDGE ( 'NONE', *, *, #28751, .F. ) ;
#8565 = DIRECTION ( 'NONE',  ( -1.000000000000000000, -0.000000000000000000, -0.000000000000000000 ) ) ;
#8566 = ORIENTED_EDGE ( 'NONE', *, *, #13570, .T. ) ;
#8567 = DIRECTION ( 'NONE',  ( -0.000000000000000000, 1.000000000000000000, -0.000000000000000000 ) ) ;
#8568 = CARTESIAN_POINT ( 'NONE',  ( 1.930368855416772611, 1.471021869409010030, 2.234437973217711093 ) ) ;
#8569 = DIRECTION ( 'NONE',  ( 1.734723475976806848E-16, -0.000000000000000000, 1.000000000000000000 ) ) ;
#8570 = ORIENTED_EDGE ( 'NONE', *, *, #15651, .F. ) ;
#8571 = AXIS2_PLACEMENT_3D ( 'NONE', #5925, #21680, #13938 ) ;
#8572 = ORIENTED_EDGE ( 'NONE', *, *, #22408, .F. ) ;
#8573 = ORIENTED_EDGE ( 'NONE', *, *, #45343, .F. ) ;
#8574 = FACE_OUTER_BOUND ( 'NONE', #46090, .T. ) ;
#8575 = CONICAL_SURFACE ( 'NONE', #15981, 2.246510896728926010, 0.01601546068027819014 ) ;
#8576 = ORIENTED_EDGE ( 'NONE', *, *, #19455, .F. ) ;
#8577 = VERTEX_POINT ( 'NONE', #49571 ) ;
#8578 = CARTESIAN_POINT ( 'NONE',  ( -0.07591351300297333182, 0.000000000000000000, 0.1574803149606283648 ) ) ;
#8579 = LINE ( 'NONE', #47524, #21159 ) ;
#8580 = CARTESIAN_POINT ( 'NONE',  ( -1.181102362204724310, 0.5905511811023621549, -1.062992125984252079 ) ) ;
#8581 = VECTOR ( 'NONE', #48608, 39.37007874015748143 ) ;
#8582 = CIRCLE ( 'NONE', #37466, 2.246510896728926010 ) ;
#8583 = VERTEX_POINT ( 'NONE', #17620 ) ;
#8584 = LINE ( 'NONE', #842, #28773 ) ;
#8585 = LINE ( 'NONE', #4969, #8505 ) ;
#8586 = DIRECTION ( 'NONE',  ( -0.000000000000000000, 1.000000000000000000, -0.000000000000000000 ) ) ;
#8587 = ORIENTED_EDGE ( 'NONE', *, *, #8414, .F. ) ;
#8588 = CARTESIAN_POINT ( 'NONE',  ( 1.363819533518803251, 0.000000000000000000, 1.102362204724403938 ) ) ;
#8589 = DIRECTION ( 'NONE',  ( 1.734723475976806848E-16, -0.000000000000000000, 1.000000000000000000 ) ) ;
#8590 = EDGE_CURVE ( 'NONE', #39122, #44945, #13752, .T. ) ;
#8591 = ORIENTED_EDGE ( 'NONE', *, *, #27706, .T. ) ;
#8592 = EDGE_CURVE ( 'NONE', #6504, #30555, #9876, .T. ) ;
#8593 = CARTESIAN_POINT ( 'NONE',  ( 0.002207914879453961969, 5.905511811023623991, 0.04916304461325442243 ) ) ;
#8594 = VERTEX_POINT ( 'NONE', #11641 ) ;
#8595 = ORIENTED_EDGE ( 'NONE', *, *, #2609, .F. ) ;
#8596 = DIRECTION ( 'NONE',  ( -1.000000000000000000, 0.000000000000000000, 0.000000000000000000 ) ) ;
#8597 = EDGE_CURVE ( 'NONE', #12593, #50064, #7272, .T. ) ;
#8598 = CARTESIAN_POINT ( 'NONE',  ( 0.002207914879453961969, 5.905511811023623991, 0.04916304461325442243 ) ) ;
#8599 = LINE ( 'NONE', #81, #45893 ) ;
#8600 = EDGE_CURVE ( 'NONE', #20045, #14432, #7768, .T. ) ;
#8601 = LINE ( 'NONE', #5496, #7368 ) ;
#8602 = ORIENTED_EDGE ( 'NONE', *, *, #27240, .T. ) ;
#8603 = ORIENTED_EDGE ( 'NONE', *, *, #22757, .F. ) ;
#8604 = FACE_OUTER_BOUND ( 'NONE', #43171, .T. ) ;
#8605 = VERTEX_POINT ( 'NONE', #269 ) ;
#8606 = PLANE ( 'NONE',  #31881 ) ;
#8607 = DIRECTION ( 'NONE',  ( -1.000000000000000000, 0.000000000000000000, 0.000000000000000000 ) ) ;
#8608 = ADVANCED_FACE ( 'NONE', ( #47215 ), #16023, .F. ) ;
#8609 = CARTESIAN_POINT ( 'NONE',  ( 2.715732320886252271, 5.118110236220475784, 1.948858261851765583 ) ) ;
#8610 = AXIS2_PLACEMENT_3D ( 'NONE', #6826, #38828, #7834 ) ;
#8611 = DIRECTION ( 'NONE',  ( -3.469446951953613696E-16, 0.000000000000000000, -1.000000000000000000 ) ) ;
#8612 = LINE ( 'NONE', #868, #36910 ) ;
#8613 = EDGE_LOOP ( 'NONE', ( #30438, #35733, #2498, #36194 ) ) ;
#8614 = VECTOR ( 'NONE', #46236, 39.37007874015748143 ) ;
#8615 = PLANE ( 'NONE',  #29151 ) ;
#8616 = EDGE_CURVE ( 'NONE', #20464, #19026, #47191, .T. ) ;
#8617 = VECTOR ( 'NONE', #8698, 39.37007874015748143 ) ;
#8618 = PLANE ( 'NONE',  #27349 ) ;
#8619 = AXIS2_PLACEMENT_3D ( 'NONE', #35615, #18158, #12370 ) ;
#8620 = VERTEX_POINT ( 'NONE', #46720 ) ;
#8621 = DIRECTION ( 'NONE',  ( 1.000000000000000000, 0.000000000000000000, 0.000000000000000000 ) ) ;
#8622 = CARTESIAN_POINT ( 'NONE',  ( -0.7381027496704855029, 1.707760278544290689, -2.859439394060923512 ) ) ;
#8623 = CARTESIAN_POINT ( 'NONE',  ( 2.711393191283637982, 1.758056152059489063, 0.4169452149318388368 ) ) ;
#8624 = EDGE_CURVE ( 'NONE', #29978, #39017, #15, .T. ) ;
#8625 = ORIENTED_EDGE ( 'NONE', *, *, #22011, .F. ) ;
#8626 = CARTESIAN_POINT ( 'NONE',  ( 1.909347346926324462, 3.346456692913386100, -0.7874015748031473194 ) ) ;
#8627 = CARTESIAN_POINT ( 'NONE',  ( 1.363819533518803473, 3.267716535433071279, -2.365849761790805980E-16 ) ) ;
#8628 = CARTESIAN_POINT ( 'NONE',  ( -1.097585813245683273, 0.5905511811023621549, -0.9794755770252108196 ) ) ;
#8629 = VECTOR ( 'NONE', #21646, 39.37007874015748143 ) ;
#8630 = ORIENTED_EDGE ( 'NONE', *, *, #48756, .T. ) ;
#8631 = CARTESIAN_POINT ( 'NONE',  ( 1.909347346926324684, 0.000000000000000000, 1.102362204724403938 ) ) ;
#8632 = DIRECTION ( 'NONE',  ( 8.881784197001252323E-16, 0.000000000000000000, -1.000000000000000000 ) ) ;
#8633 = ORIENTED_EDGE ( 'NONE', *, *, #16320, .F. ) ;
#8634 = DIRECTION ( 'NONE',  ( -0.9998717552508122886, -0.01601477604151180928, 0.000000000000000000 ) ) ;
#8635 = EDGE_CURVE ( 'NONE', #50807, #7499, #3899, .T. ) ;
#8636 = CARTESIAN_POINT ( 'NONE',  ( -1.636583440222563635, 0.000000000000000000, 0.7480314960629874665 ) ) ;
#8637 = PLANE ( 'NONE',  #39536 ) ;
#8638 = DIRECTION ( 'NONE',  ( -0.08963930890342654279, 1.156097046908844086E-16, -0.9959742939952397345 ) ) ;
#8639 = ORIENTED_EDGE ( 'NONE', *, *, #48430, .F. ) ;
#8640 = ORIENTED_EDGE ( 'NONE', *, *, #28715, .T. ) ;
#8641 = CARTESIAN_POINT ( 'NONE',  ( -1.363819533518803473, 0.000000000000000000, -0.6692913385826760875 ) ) ;
#8642 = CARTESIAN_POINT ( 'NONE',  ( -2.671951887028160666, 1.575085747223753829, 0.3122784236066050711 ) ) ;
#8643 = ORIENTED_EDGE ( 'NONE', *, *, #33338, .F. ) ;
#8644 = LINE ( 'NONE', #9156, #28327 ) ;
#8645 = CARTESIAN_POINT ( 'NONE',  ( 0.5455278134075216556, 3.267716535433071279, 2.007874015748021268 ) ) ;
#8646 = LINE ( 'NONE', #646, #40145 ) ;
#8647 = CARTESIAN_POINT ( 'NONE',  ( -2.074656761898998170, 0.000000000000000000, -0.6223516566630912239 ) ) ;
#8648 = ORIENTED_EDGE ( 'NONE', *, *, #44263, .F. ) ;
#8649 = ORIENTED_EDGE ( 'NONE', *, *, #30946, .F. ) ;
#8650 = CARTESIAN_POINT ( 'NONE',  ( 0.000000000000000000, 7.874015748031496287, -0.3740157480314960647 ) ) ;
#8651 = CARTESIAN_POINT ( 'NONE',  ( 0.000000000000000000, 3.267716535433071279, -1.141732283464564013 ) ) ;
#8652 = CARTESIAN_POINT ( 'NONE',  ( -0.8013547813281791665, 1.608322728230706655, -2.841982942506608989 ) ) ;
#8653 = DIRECTION ( 'NONE',  ( 0.000000000000000000, -1.000000000000000000, -0.000000000000000000 ) ) ;
#8654 = FACE_BOUND ( 'NONE', #36413, .T. ) ;
#8655 = AXIS2_PLACEMENT_3D ( 'NONE', #32051, #12416, #20414 ) ;
#8656 = ORIENTED_EDGE ( 'NONE', *, *, #22719, .T. ) ;
#8657 = CARTESIAN_POINT ( 'NONE',  ( 0.000000000000000000, 3.267716535433071279, -0.5118110236220471121 ) ) ;
#8658 = VECTOR ( 'NONE', #38023, 39.37007874015748143 ) ;
#8659 = ORIENTED_EDGE ( 'NONE', *, *, #9951, .T. ) ;
#8660 = VERTEX_POINT ( 'NONE', #35141 ) ;
#8661 = CARTESIAN_POINT ( 'NONE',  ( -2.182111253630085290, 3.267716535433071279, 0.3149606299212578953 ) ) ;
#8662 = AXIS2_PLACEMENT_3D ( 'NONE', #7616, #3236, #30357 ) ;
#8663 = EDGE_CURVE ( 'NONE', #36157, #15505, #31522, .T. ) ;
#8664 = EDGE_CURVE ( 'NONE', #12716, #23414, #31012, .T. ) ;
#8665 = ORIENTED_EDGE ( 'NONE', *, *, #48313, .T. ) ;
#8666 = ORIENTED_EDGE ( 'NONE', *, *, #22921, .T. ) ;
#8667 = CARTESIAN_POINT ( 'NONE',  ( -0.2727639067037607723, 0.000000000000000000, -1.732283464566922726 ) ) ;
#8668 = ADVANCED_FACE ( 'NONE', ( #31780 ), #15264, .F. ) ;
#8669 = UNCERTAINTY_MEASURE_WITH_UNIT (LENGTH_MEASURE( 1.000000000000000082E-05 ), #21318, 'distance_accuracy_value', 'NONE');
#8670 = ORIENTED_EDGE ( 'NONE', *, *, #19464, .T. ) ;
#8671 = VECTOR ( 'NONE', #19038, 39.37007874015748143 ) ;
#8672 = LINE ( 'NONE', #44288, #9774 ) ;
#8673 = CARTESIAN_POINT ( 'NONE',  ( -1.675814739737315540, 1.582635513994296250, 1.399362935606387470 ) ) ;
#8674 = DIRECTION ( 'NONE',  ( 1.000000000000000000, 0.000000000000000000, 0.000000000000000000 ) ) ;
#8675 = PLANE ( 'NONE',  #14885 ) ;
#8676 = CARTESIAN_POINT ( 'NONE',  ( 1.909347346926324684, 3.346456692913386100, 0.7874015748031456541 ) ) ;
#8677 = CARTESIAN_POINT ( 'NONE',  ( -1.363819533518803473, 0.000000000000000000, 1.535433070866133232 ) ) ;
#8678 = ORIENTED_EDGE ( 'NONE', *, *, #44287, .T. ) ;
#8679 = DIRECTION ( 'NONE',  ( -3.986037398843765983E-20, -1.000000000000000000, -1.160734090543304660E-16 ) ) ;
#8680 = DIRECTION ( 'NONE',  ( -3.986037398843765983E-20, -1.000000000000000000, -1.160734090543304660E-16 ) ) ;
#8681 = CARTESIAN_POINT ( 'NONE',  ( 0.1968503937007873850, 3.267716535433071279, -0.1968503937007874405 ) ) ;
#8682 = VERTEX_POINT ( 'NONE', #34887 ) ;
#8683 = DIRECTION ( 'NONE',  ( 1.000000000000000000, 0.000000000000000000, 0.000000000000000000 ) ) ;
#8684 = CARTESIAN_POINT ( 'NONE',  ( -0.3486774197067336045, 3.267716535433071279, 1.209717811016577845E-16 ) ) ;
#8685 = ORIENTED_EDGE ( 'NONE', *, *, #3772, .F. ) ;
#8686 = CARTESIAN_POINT ( 'NONE',  ( -0.6214413264104945434, 3.346456692913386100, -1.417322834645664331 ) ) ;
#8687 = ADVANCED_FACE ( 'NONE', ( #3389 ), #26868, .T. ) ;
#8688 = CARTESIAN_POINT ( 'NONE',  ( 1.215807329263347114, 1.628950133432788494, 1.938968878379255578 ) ) ;
#8689 = CARTESIAN_POINT ( 'NONE',  ( 4.268512490100411402E-16, 3.346456692913386100, 0.9448818897637749625 ) ) ;
#8690 = CONICAL_SURFACE ( 'NONE', #29293, 3.483074324928249421, 1.244861948955335196 ) ;
#8691 = VECTOR ( 'NONE', #43614, 39.37007874015748854 ) ;
#8692 = ORIENTED_EDGE ( 'NONE', *, *, #11893, .F. ) ;
#8693 = DIRECTION ( 'NONE',  ( 0.000000000000000000, -1.000000000000000000, 0.000000000000000000 ) ) ;
#8694 = VERTEX_POINT ( 'NONE', #15761 ) ;
#8695 = CARTESIAN_POINT ( 'NONE',  ( 2.695799277629594037, 1.761268146152256575, -1.205759334241453651 ) ) ;
#8696 = EDGE_CURVE ( 'NONE', #2462, #43721, #11392, .T. ) ;
#8697 = VECTOR ( 'NONE', #3679, 39.37007874015748143 ) ;
#8698 = DIRECTION ( 'NONE',  ( -0.000000000000000000, 1.000000000000000000, -0.000000000000000000 ) ) ;
#8699 = DIRECTION ( 'NONE',  ( -0.000000000000000000, 1.000000000000000000, -0.000000000000000000 ) ) ;
#8700 = LINE ( 'NONE', #40204, #43251 ) ;
#8701 = ADVANCED_FACE ( 'NONE', ( #3645 ), #46474, .F. ) ;
#8702 = AXIS2_PLACEMENT_3D ( 'NONE', #29602, #45318, #25721 ) ;
#8703 = ORIENTED_EDGE ( 'NONE', *, *, #11287, .F. ) ;
#8704 = ORIENTED_EDGE ( 'NONE', *, *, #15285, .F. ) ;
#8705 = DIRECTION ( 'NONE',  ( 1.000000000000000000, 0.000000000000000000, 0.000000000000000000 ) ) ;
#8706 = ORIENTED_EDGE ( 'NONE', *, *, #35063, .F. ) ;
#8707 = ADVANCED_FACE ( 'NONE', ( #39008 ), #15517, .F. ) ;
#8708 = CARTESIAN_POINT ( 'NONE',  ( -0.8182917201112819283, 3.267716535433071279, 0.1574803149606285035 ) ) ;
#8709 = ORIENTED_EDGE ( 'NONE', *, *, #33461, .F. ) ;
#8710 = EDGE_CURVE ( 'NONE', #32803, #47925, #23255, .T. ) ;
#8711 = DIRECTION ( 'NONE',  ( -3.469446951953613696E-16, 0.000000000000000000, -1.000000000000000000 ) ) ;
#8712 = VERTEX_POINT ( 'NONE', #4150 ) ;
#8713 = CARTESIAN_POINT ( 'NONE',  ( 0.1968503937007873017, 3.346456692913386100, -0.3149606299212591165 ) ) ;
#8714 = LINE ( 'NONE', #36601, #34714 ) ;
#8715 = EDGE_LOOP ( 'NONE', ( #22586, #42494, #43460, #30061 ) ) ;
#8716 = CARTESIAN_POINT ( 'NONE',  ( 0.000000000000000000, 3.267716535433071279, -2.244094488188969727 ) ) ;
#8717 = ORIENTED_EDGE ( 'NONE', *, *, #6683, .F. ) ;
#8718 = EDGE_CURVE ( 'NONE', #46669, #27924, #35646, .T. ) ;
#8719 = CARTESIAN_POINT ( 'NONE',  ( 1.673977678072228414, 0.5225566574842699374, -1.532400001105657106 ) ) ;
#8720 = EDGE_LOOP ( 'NONE', ( #26797, #39532, #47455, #16905 ) ) ;
#8721 = ORIENTED_EDGE ( 'NONE', *, *, #45834, .T. ) ;
#8722 = EDGE_CURVE ( 'NONE', #18090, #20587, #1041, .T. ) ;
#8723 = EDGE_CURVE ( 'NONE', #46164, #34660, #17061, .T. ) ;
#8724 = DIRECTION ( 'NONE',  ( -0.000000000000000000, 1.000000000000000000, -0.000000000000000000 ) ) ;
#8725 = VECTOR ( 'NONE', #14953, 39.37007874015748143 ) ;
#8726 = ORIENTED_EDGE ( 'NONE', *, *, #23448, .T. ) ;
#8727 = CARTESIAN_POINT ( 'NONE',  ( 2.867773316779195447, 1.763947033723992641, -0.7050287376752004675 ) ) ;
#8728 = VECTOR ( 'NONE', #44381, 39.37007874015748143 ) ;
#8729 = ORIENTED_EDGE ( 'NONE', *, *, #44896, .F. ) ;
#8730 = CARTESIAN_POINT ( 'NONE',  ( 0.5455278134075211005, 3.267716535433071279, -1.141732283464564013 ) ) ;
#8731 = DIRECTION ( 'NONE',  ( -0.000000000000000000, 1.000000000000000000, -0.000000000000000000 ) ) ;
#8732 = AXIS2_PLACEMENT_3D ( 'NONE', #25867, #10634, #41117 ) ;
#8733 = FACE_OUTER_BOUND ( 'NONE', #15885, .T. ) ;
#8734 = ORIENTED_EDGE ( 'NONE', *, *, #16855, .F. ) ;
#8735 = VECTOR ( 'NONE', #43666, 39.37007874015748143 ) ;
#8736 = CARTESIAN_POINT ( 'NONE',  ( 1.560669927219590747, 0.000000000000000000, 1.102362204724403938 ) ) ;
#8737 = DIRECTION ( 'NONE',  ( 1.000000000000000000, -0.000000000000000000, 0.000000000000000000 ) ) ;
#8738 = CARTESIAN_POINT ( 'NONE',  ( 2.607957125086718175, 1.759890798980135118, 1.384772967391346921 ) ) ;
#8739 = DIRECTION ( 'NONE',  ( 1.000000000000000000, 0.000000000000000000, 0.000000000000000000 ) ) ;
#8740 = LINE ( 'NONE', #24747, #26810 ) ;
#8741 = LINE ( 'NONE', #32246, #20689 ) ;
#8742 = DIRECTION ( 'NONE',  ( 0.000000000000000000, 0.000000000000000000, -1.000000000000000000 ) ) ;
#8743 = ORIENTED_EDGE ( 'NONE', *, *, #40634, .F. ) ;
#8744 = EDGE_CURVE ( 'NONE', #50070, #46776, #45596, .T. ) ;
#8745 = DIRECTION ( 'NONE',  ( -0.9998717552508122886, -0.01601477604151180928, 0.000000000000000000 ) ) ;
#8746 = ORIENTED_EDGE ( 'NONE', *, *, #43855, .F. ) ;
#8747 = DIRECTION ( 'NONE',  ( 0.000000000000000000, -0.000000000000000000, -1.000000000000000000 ) ) ;
#8748 = VERTEX_POINT ( 'NONE', #32818 ) ;
#8749 = EDGE_CURVE ( 'NONE', #50070, #26751, #36937, .T. ) ;
#8750 = FACE_OUTER_BOUND ( 'NONE', #9935, .T. ) ;
#8751 = CARTESIAN_POINT ( 'NONE',  ( 0.8182917201112824834, 3.346456692913386100, 1.732283464566921172 ) ) ;
#8752 = EDGE_CURVE ( 'NONE', #46970, #912, #25834, .T. ) ;
#8753 = CARTESIAN_POINT ( 'NONE',  ( 0.000000000000000000, 6.692913385826772199, 0.000000000000000000 ) ) ;
#8754 = LINE ( 'NONE', #13657, #11245 ) ;
#8755 = ORIENTED_EDGE ( 'NONE', *, *, #30047, .T. ) ;
#8756 = ADVANCED_FACE ( 'NONE', ( #12403 ), #20141, .F. ) ;
#8757 = AXIS2_PLACEMENT_3D ( 'NONE', #27643, #36181, #23783 ) ;
#8758 = DIRECTION ( 'NONE',  ( 1.000000000000000000, 0.000000000000000000, -3.469446951953613696E-16 ) ) ;
#8759 = VECTOR ( 'NONE', #1487, 39.37007874015748143 ) ;
#8760 = CARTESIAN_POINT ( 'NONE',  ( 0.6502734851936936566, 1.718317270777941941, -2.171228911417812046 ) ) ;
#8761 = VECTOR ( 'NONE', #3022, 39.37007874015748143 ) ;
#8762 = ORIENTED_EDGE ( 'NONE', *, *, #32213, .F. ) ;
#8763 = DIRECTION ( 'NONE',  ( -0.01601477604151182663, 0.9998717552508123996, -0.000000000000000000 ) ) ;
#8764 = VECTOR ( 'NONE', #29730, 39.37007874015748143 ) ;
#8765 = VERTEX_POINT ( 'NONE', #9304 ) ;
#8766 = CARTESIAN_POINT ( 'NONE',  ( 1.091055626815042645, 3.346456692913386100, 0.7480314960629872445 ) ) ;
#8767 = LINE ( 'NONE', #24520, #23955 ) ;
#8768 = VECTOR ( 'NONE', #50232, 39.37007874015748143 ) ;
#8769 = EDGE_CURVE ( 'NONE', #14380, #20677, #4662, .T. ) ;
#8770 = AXIS2_PLACEMENT_3D ( 'NONE', #49183, #13861, #45831 ) ;
#8771 = CARTESIAN_POINT ( 'NONE',  ( -0.7874015748031498729, 0.000000000000000000, -1.138269997360109921E-16 ) ) ;
#8772 = ORIENTED_EDGE ( 'NONE', *, *, #41715, .T. ) ;
#8773 = ORIENTED_EDGE ( 'NONE', *, *, #39535, .F. ) ;
#8774 = CARTESIAN_POINT ( 'NONE',  ( 1.951523201471517588, 0.05917688107560774985, -0.1369052102211298083 ) ) ;
#8775 = DIRECTION ( 'NONE',  ( -0.000000000000000000, 1.000000000000000000, -0.000000000000000000 ) ) ;
#8776 = LINE ( 'NONE', #24783, #44979 ) ;
#8777 = EDGE_CURVE ( 'NONE', #14924, #10014, #40855, .T. ) ;
#8778 = DIRECTION ( 'NONE',  ( -1.000000000000000000, 0.000000000000000000, -0.000000000000000000 ) ) ;
#8779 = LINE ( 'NONE', #39761, #19222 ) ;
#8780 = ORIENTED_EDGE ( 'NONE', *, *, #34627, .F. ) ;
#8781 = EDGE_CURVE ( 'NONE', #3510, #23904, #32447, .T. ) ;
#8782 = CARTESIAN_POINT ( 'NONE',  ( 0.4696143004045481018, 3.267716535433071279, -1.629301903132388246E-16 ) ) ;
#8783 = EDGE_CURVE ( 'NONE', #30043, #46764, #50038, .T. ) ;
#8784 = EDGE_LOOP ( 'NONE', ( #24882, #9743, #16857, #27576 ) ) ;
#8785 = VERTEX_POINT ( 'NONE', #4402 ) ;
#8786 = CONTEXT_DEPENDENT_SHAPE_REPRESENTATION ( #25947, #12472 ) ;
#8787 = EDGE_LOOP ( 'NONE', ( #33163, #34853, #24233, #50293 ) ) ;
#8788 = CARTESIAN_POINT ( 'NONE',  ( -1.712496953225537188, 3.267716535433071279, 5.941417334598190051E-16 ) ) ;
#8789 = DIRECTION ( 'NONE',  ( 0.000000000000000000, -1.000000000000000000, 0.000000000000000000 ) ) ;
#8791 = DIRECTION ( 'NONE',  ( -1.000000000000000000, 0.000000000000000000, 0.000000000000000000 ) ) ;
#8790 = VECTOR ( 'NONE', #7417, 39.37007874015748143 ) ;
#8792 = FACE_OUTER_BOUND ( 'NONE', #13756, .T. ) ;
#8793 = ORIENTED_EDGE ( 'NONE', *, *, #20165, .T. ) ;
#8794 = ORIENTED_EDGE ( 'NONE', *, *, #46353, .T. ) ;
#8796 = VECTOR ( 'NONE', #38714, 39.37007874015748143 ) ;
#8795 = CARTESIAN_POINT ( 'NONE',  ( -1.055804188380104813, 0.000000000000000000, -1.480985967717771690 ) ) ;
#8797 = PLANE ( 'NONE',  #49339 ) ;
#8798 = VECTOR ( 'NONE', #5567, 39.37007874015748143 ) ;
#8799 = DIRECTION ( 'NONE',  ( -1.000000000000000000, 0.000000000000000000, 0.000000000000000000 ) ) ;
#8800 = CARTESIAN_POINT ( 'NONE',  ( -1.363819533518803473, 3.346456692913386100, -1.605145679676863057 ) ) ;
#8801 = DIRECTION ( 'NONE',  ( -0.7660444431189771253, 0.6427876096865404731, 0.000000000000000000 ) ) ;
#8802 = CARTESIAN_POINT ( 'NONE',  ( -1.936750629140493007, 1.578456148182591168, 0.9863243683714766341 ) ) ;
#8803 = AXIS2_PLACEMENT_3D ( 'NONE', #32109, #35975, #44217 ) ;
#8804 = DIRECTION ( 'NONE',  ( -1.000000000000000000, 0.000000000000000000, -0.000000000000000000 ) ) ;
#8805 = CARTESIAN_POINT ( 'NONE',  ( 0.6529837180168069910, 0.8335264911517238362, 0.6529837180168082122 ) ) ;
#8806 = VECTOR ( 'NONE', #35190, 39.37007874015748143 ) ;
#8807 = EDGE_LOOP ( 'NONE', ( #37740, #32720, #3581, #44901 ) ) ;
#8808 = DIRECTION ( 'NONE',  ( 1.000000000000000000, 0.000000000000000000, 0.000000000000000000 ) ) ;
#8809 =( CONVERSION_BASED_UNIT ( 'INCH', #39790 ) LENGTH_UNIT ( ) NAMED_UNIT ( #53 ) );
#8810 = ORIENTED_EDGE ( 'NONE', *, *, #35364, .F. ) ;
#8811 = ORIENTED_EDGE ( 'NONE', *, *, #6799, .F. ) ;
#8812 = CARTESIAN_POINT ( 'NONE',  ( -1.712496953225537633, 3.267716535433071279, 1.417322834645662333 ) ) ;
#8813 = DIRECTION ( 'NONE',  ( -1.000000000000000000, 0.000000000000000000, 0.000000000000000000 ) ) ;
#8814 = FACE_OUTER_BOUND ( 'NONE', #30517, .T. ) ;
#8815 = ADVANCED_FACE ( 'NONE', ( #40548 ), #5170, .F. ) ;
#8816 = VERTEX_POINT ( 'NONE', #36678 ) ;
#8817 = ADVANCED_FACE ( 'NONE', ( #1298 ), #47477, .T. ) ;
#8818 = EDGE_CURVE ( 'NONE', #1340, #35947, #35903, .T. ) ;
#8819 = ORIENTED_EDGE ( 'NONE', *, *, #34591, .F. ) ;
#8820 = CARTESIAN_POINT ( 'NONE',  ( 1.062992125984252079, 0.000000000000000000, -1.014069264286642014 ) ) ;
#8821 = VERTEX_POINT ( 'NONE', #530 ) ;
#8822 = B_SPLINE_CURVE_WITH_KNOTS ( 'NONE', 3,
 ( #14273, #30021, #45740, #2910 ),
 .UNSPECIFIED., .F., .F.,
 ( 4, 4 ),
 ( 2.558985349373473962E-07, 0.002500451054789445439 ),
 .UNSPECIFIED. ) ;
#8823 = CARTESIAN_POINT ( 'NONE',  ( -1.721400284384397628, 0.0003482895740541699209, 0.2828415639128913361 ) ) ;
#8824 = ORIENTED_EDGE ( 'NONE', *, *, #50451, .F. ) ;
#8825 = CARTESIAN_POINT ( 'NONE',  ( -1.909347346926324906, 0.000000000000000000, -1.299212598425193210 ) ) ;
#8826 = CARTESIAN_POINT ( 'NONE',  ( 0.07982360342473591996, 1.709180471932028711, 0.000000000000000000 ) ) ;
#8827 = CARTESIAN_POINT ( 'NONE',  ( -0.2727639067037602172, 3.346456692913386100, 1.732283464566921172 ) ) ;
#8828 = AXIS2_PLACEMENT_3D ( 'NONE', #37786, #14276, #28999 ) ;
#8829 = ORIENTED_EDGE ( 'NONE', *, *, #38718, .T. ) ;
#8830 = EDGE_LOOP ( 'NONE', ( #1598, #37943, #35775, #2230 ) ) ;
#8831 = ORIENTED_EDGE ( 'NONE', *, *, #24971, .F. ) ;
#8832 = CARTESIAN_POINT ( 'NONE',  ( -0.5455278134075216556, 3.346456692913386100, -2.204724409448810540 ) ) ;
#8833 = ORIENTED_EDGE ( 'NONE', *, *, #13469, .T. ) ;
#8834 = ORIENTED_EDGE ( 'NONE', *, *, #15962, .F. ) ;
#8835 = CARTESIAN_POINT ( 'NONE',  ( -0.9836083787002332102, 1.574803149606302854, -1.929060376159713375 ) ) ;
#8836 = LINE ( 'NONE', #32603, #44213 ) ;
#8837 = CARTESIAN_POINT ( 'NONE',  ( -0.8942052331142552601, 3.346456692913386100, 2.204724409448808764 ) ) ;
#8838 = EDGE_CURVE ( 'NONE', #286, #37788, #16280, .T. ) ;
#8839 = EDGE_LOOP ( 'NONE', ( #1232, #37953, #48018, #48319 ) ) ;
#8840 = EDGE_CURVE ( 'NONE', #45259, #24676, #24286, .T. ) ;
#8841 = DIRECTION ( 'NONE',  ( 1.000000000000000000, 0.000000000000000000, 0.000000000000000000 ) ) ;
#8842 = CARTESIAN_POINT ( 'NONE',  ( 0.4696143004045478797, 0.000000000000000000, -0.3543307086614173040 ) ) ;
#8843 = LINE ( 'NONE', #13995, #12142 ) ;
#8844 = ORIENTED_EDGE ( 'NONE', *, *, #27196, .T. ) ;
#8845 = DIRECTION ( 'NONE',  ( 0.000000000000000000, 0.000000000000000000, -1.000000000000000000 ) ) ;
#8846 = CARTESIAN_POINT ( 'NONE',  ( -2.103998301714549157, 3.267716535433071279, -0.5118110236220464460 ) ) ;
#8847 = ORIENTED_EDGE ( 'NONE', *, *, #10414, .T. ) ;
#8848 = ADVANCED_FACE ( 'NONE', ( #40032 ), #789, .F. ) ;
#8849 = FACE_OUTER_BOUND ( 'NONE', #12535, .T. ) ;
#8850 = EDGE_LOOP ( 'NONE', ( #22844, #27179, #40350, #525 ) ) ;
#8851 = ORIENTED_EDGE ( 'NONE', *, *, #30946, .T. ) ;
#8852 = DIRECTION ( 'NONE',  ( 2.891205793294678326E-16, 0.000000000000000000, -1.000000000000000000 ) ) ;
#8853 = CARTESIAN_POINT ( 'NONE',  ( 0.3467207527347879736, 6.692913385826772199, 2.186201806782071877 ) ) ;
#8854 = AXIS2_PLACEMENT_3D ( 'NONE', #25498, #10517, #17756 ) ;
#8855 = EDGE_CURVE ( 'NONE', #29456, #28387, #40293, .T. ) ;
#8856 = CARTESIAN_POINT ( 'NONE',  ( -1.439733046521777027, 3.346456692913386100, -0.5118110236220466680 ) ) ;
#8857 = DIRECTION ( 'NONE',  ( -3.469446951953613696E-16, 0.000000000000000000, -1.000000000000000000 ) ) ;
#8858 = CARTESIAN_POINT ( 'NONE',  ( -0.5455278134075214336, 3.267716535433071279, 9.463399047163224412E-17 ) ) ;
#8859 = ORIENTED_EDGE ( 'NONE', *, *, #1186, .T. ) ;
#8860 = ORIENTED_EDGE ( 'NONE', *, *, #45843, .T. ) ;
#8861 = CARTESIAN_POINT ( 'NONE',  ( 0.2727639067037604392, 3.267716535433071279, -1.614173228346451605 ) ) ;
#8862 = VERTEX_POINT ( 'NONE', #13948 ) ;
#8863 = PLANE ( 'NONE',  #28584 ) ;
#8864 = DIRECTION ( 'NONE',  ( -0.000000000000000000, 1.000000000000000000, -0.000000000000000000 ) ) ;
#8865 = VECTOR ( 'NONE', #36986, 39.37007874015748143 ) ;
#8866 = VECTOR ( 'NONE', #293, 39.37007874015748143 ) ;
#8867 = CARTESIAN_POINT ( 'NONE',  ( 2.923830774216937822, 1.666335789833975900, 0.4126137885002218453 ) ) ;
#8868 = CARTESIAN_POINT ( 'NONE',  ( 4.268512490100411402E-16, 0.000000000000000000, 1.259842519685033357 ) ) ;
#8869 = DIRECTION ( 'NONE',  ( -0.000000000000000000, 1.000000000000000000, -0.000000000000000000 ) ) ;
#8870 = ORIENTED_EDGE ( 'NONE', *, *, #3987, .T. ) ;
#8871 = LINE ( 'NONE', #27715, #37392 ) ;
#8872 = FACE_OUTER_BOUND ( 'NONE', #43122, .T. ) ;
#8873 = VERTEX_POINT ( 'NONE', #14194 ) ;
#8874 = PLANE ( 'NONE',  #28177 ) ;
#8875 = CARTESIAN_POINT ( 'NONE',  ( 0.1450362469327826365, 1.574803149606302854, -2.160491579385212191 ) ) ;
#8876 = DIRECTION ( 'NONE',  ( -0.000000000000000000, -1.000000000000000000, -0.000000000000000000 ) ) ;
#8877 = ORIENTED_EDGE ( 'NONE', *, *, #20324, .T. ) ;
#8878 = FACE_OUTER_BOUND ( 'NONE', #14737, .T. ) ;
#8879 = DIRECTION ( 'NONE',  ( 1.734723475976806848E-16, 0.000000000000000000, 1.000000000000000000 ) ) ;
#8880 = LINE ( 'NONE', #50917, #44028 ) ;
#8881 = ADVANCED_FACE ( 'NONE', ( #21952 ), #29692, .F. ) ;
#8882 = EDGE_CURVE ( 'NONE', #12300, #4494, #6455, .T. ) ;
#8883 = ORIENTED_EDGE ( 'NONE', *, *, #15012, .T. ) ;
#8884 = CARTESIAN_POINT ( 'NONE',  ( -0.8942052331142552601, 3.346456692913386100, -1.889763779527552146 ) ) ;
#8885 = CARTESIAN_POINT ( 'NONE',  ( -0.5455278134075214336, 3.267716535433071279, -0.1968503937007883287 ) ) ;
#8886 = ORIENTED_EDGE ( 'NONE', *, *, #37655, .F. ) ;
#8887 = AXIS2_PLACEMENT_3D ( 'NONE', #24937, #24430, #12549 ) ;
#8888 = DIRECTION ( 'NONE',  ( 1.734723475976806848E-16, -0.000000000000000000, 1.000000000000000000 ) ) ;
#8889 = EDGE_CURVE ( 'NONE', #37676, #36095, #6199, .T. ) ;
#8890 = DIRECTION ( 'NONE',  ( 0.000000000000000000, 1.000000000000000000, 0.000000000000000000 ) ) ;
#8891 = CARTESIAN_POINT ( 'NONE',  ( 1.833433833923351353, 3.346456692913386100, 0.3149606299212576177 ) ) ;
#8892 = CARTESIAN_POINT ( 'NONE',  ( 0.6284326417183513369, 0.02518258341035289893, 1.814510055229779040 ) ) ;
#8893 = EDGE_CURVE ( 'NONE', #25998, #48706, #43091, .T. ) ;
#8894 = EDGE_LOOP ( 'NONE', ( #3639, #18262, #34261, #18056 ) ) ;
#8895 = ORIENTED_EDGE ( 'NONE', *, *, #40283, .T. ) ;
#8896 = CARTESIAN_POINT ( 'NONE',  ( -0.3486774197067334935, 3.346456692913386100, 1.692913385826762873 ) ) ;
#8897 = CYLINDRICAL_SURFACE ( 'NONE', #16390, 2.952755905511811552 ) ;
#8898 = ORIENTED_EDGE ( 'NONE', *, *, #13737, .T. ) ;
#8899 = LINE ( 'NONE', #48100, #16808 ) ;
#8900 = FACE_OUTER_BOUND ( 'NONE', #33415, .T. ) ;
#8901 = PLANE ( 'NONE',  #42598 ) ;
#8902 = LINE ( 'NONE', #31902, #22383 ) ;
#8903 = ORIENTED_EDGE ( 'NONE', *, *, #37373, .T. ) ;
#8904 = EDGE_LOOP ( 'NONE', ( #12784, #37164, #36281, #40491 ) ) ;
#8905 = EDGE_CURVE ( 'NONE', #28960, #13304, #10073, .T. ) ;
#8906 = DIRECTION ( 'NONE',  ( 1.000000000000000000, 0.000000000000000000, -3.469446951953613696E-16 ) ) ;
#8907 = DIRECTION ( 'NONE',  ( 1.000000000000000000, 0.000000000000000000, 0.000000000000000000 ) ) ;
#8908 = VECTOR ( 'NONE', #43474, 39.37007874015748143 ) ;
#8909 = VECTOR ( 'NONE', #17523, 39.37007874015748143 ) ;
#8910 = DIRECTION ( 'NONE',  ( 1.734723475976806848E-16, -0.000000000000000000, 1.000000000000000000 ) ) ;
#8911 = VERTEX_POINT ( 'NONE', #2324 ) ;
#8912 = CARTESIAN_POINT ( 'NONE',  ( -0.4788131938641531637, 1.205361022782829114E-17, 2.914091152102186388 ) ) ;
#8913 = FACE_BOUND ( 'NONE', #722, .T. ) ;
#8914 = EDGE_LOOP ( 'NONE', ( #45865, #44511, #14367, #9220 ) ) ;
#8915 = EDGE_CURVE ( 'NONE', #25006, #24163, #33466, .T. ) ;
#8916 = CARTESIAN_POINT ( 'NONE',  ( 0.000000000000000000, 3.267716535433071279, 0.000000000000000000 ) ) ;
#8917 = EDGE_LOOP ( 'NONE', ( #30355, #13109, #1790, #22317 ) ) ;
#8919 = ORIENTED_EDGE ( 'NONE', *, *, #19065, .T. ) ;
#8918 = VECTOR ( 'NONE', #26366, 39.37007874015748143 ) ;
#8920 = CARTESIAN_POINT ( 'NONE',  ( -1.281152772984899491, 0.000000000000000000, -2.660341145381166506 ) ) ;
#8921 = VECTOR ( 'NONE', #22985, 39.37007874015748143 ) ;
#8922 = ORIENTED_EDGE ( 'NONE', *, *, #43509, .F. ) ;
#8923 = VERTEX_POINT ( 'NONE', #9819 ) ;
#8924 = DIRECTION ( 'NONE',  ( -1.000000000000000000, -0.000000000000000000, -0.000000000000000000 ) ) ;
#8925 = VECTOR ( 'NONE', #23703, 39.37007874015748143 ) ;
#8926 = ORIENTED_EDGE ( 'NONE', *, *, #42071, .T. ) ;
#8928 = DIRECTION ( 'NONE',  ( 1.000000000000000000, -0.000000000000000000, 0.000000000000000000 ) ) ;
#8927 = AXIS2_PLACEMENT_3D ( 'NONE', #17892, #49084, #17132 ) ;
#8929 = EDGE_CURVE ( 'NONE', #706, #12462, #33069, .T. ) ;
#8930 = DIRECTION ( 'NONE',  ( 1.000000000000000000, -0.000000000000000000, 0.000000000000000000 ) ) ;
#8931 = CARTESIAN_POINT ( 'NONE',  ( 2.073577001504950168, 0.9922959628731219395, 1.590677202529814593 ) ) ;
#8932 = DIRECTION ( 'NONE',  ( 0.3513748240813434620, 0.000000000000000000, -0.9362348706397368714 ) ) ;
#8933 = DIRECTION ( 'NONE',  ( 0.000000000000000000, 0.000000000000000000, -1.000000000000000000 ) ) ;
#8934 = DIRECTION ( 'NONE',  ( 1.734723475976806848E-16, -0.000000000000000000, 1.000000000000000000 ) ) ;
#8935 = ORIENTED_EDGE ( 'NONE', *, *, #27640, .F. ) ;
#8936 = CARTESIAN_POINT ( 'NONE',  ( 0.2727639067037609943, 3.346456692913386100, 0.9055118110236167750 ) ) ;
#8937 = LINE ( 'NONE', #43264, #28945 ) ;
#8938 = EDGE_LOOP ( 'NONE', ( #31193, #14617, #7266, #9470 ) ) ;
#8939 = CARTESIAN_POINT ( 'NONE',  ( 1.833433833923351353, 3.346456692913386100, -0.1968503937007886062 ) ) ;
#8940 = CARTESIAN_POINT ( 'NONE',  ( 1.131369771556057113, 1.631181450708906411, -2.235890070012082731 ) ) ;
#8941 = ORIENTED_EDGE ( 'NONE', *, *, #18487, .F. ) ;
#8942 = DIRECTION ( 'NONE',  ( -0.000000000000000000, 1.000000000000000000, -0.000000000000000000 ) ) ;
#8943 = VECTOR ( 'NONE', #18803, 39.37007874015748143 ) ;
#8944 = CARTESIAN_POINT ( 'NONE',  ( -1.181102362204724088, 0.4724409448818890911, 1.062992125984251413 ) ) ;
#8945 = CARTESIAN_POINT ( 'NONE',  ( 0.1155636338427008941, -0.5222242541845523167, 0.000000000000000000 ) ) ;
#8946 = ADVANCED_FACE ( 'NONE', ( #22455 ), #33832, .F. ) ;
#8947 = ORIENTED_EDGE ( 'NONE', *, *, #36408, .T. ) ;
#8948 = AXIS2_PLACEMENT_3D ( 'NONE', #43183, #19192, #3962 ) ;
#8949 = FACE_OUTER_BOUND ( 'NONE', #21200, .T. ) ;
#8950 = VERTEX_POINT ( 'NONE', #45658 ) ;
#8951 = FACE_BOUND ( 'NONE', #11720, .T. ) ;
#8952 = EDGE_CURVE ( 'NONE', #33042, #41687, #10325, .T. ) ;
#8953 = DIRECTION ( 'NONE',  ( 1.734723475976806848E-16, 0.000000000000000000, 1.000000000000000000 ) ) ;
#8954 = VECTOR ( 'NONE', #19998, 39.37007874015748143 ) ;
#8955 = VECTOR ( 'NONE', #30677, 39.37007874015748143 ) ;
#8956 = PLANE ( 'NONE',  #50602 ) ;
#8958 = EDGE_CURVE ( 'NONE', #36771, #3425, #48754, .T. ) ;
#8957 = PLANE ( 'NONE',  #48207 ) ;
#8959 = EDGE_CURVE ( 'NONE', #26189, #21459, #2576, .T. ) ;
#8960 = CONICAL_SURFACE ( 'NONE', #3164, 2.244934639244524632, 1.554780866114618743 ) ;
#8961 = ORIENTED_EDGE ( 'NONE', *, *, #40611, .T. ) ;
#8962 = VERTEX_POINT ( 'NONE', #29169 ) ;
#8963 = CARTESIAN_POINT ( 'NONE',  ( -0.2727639067037610499, 3.346456692913386100, -2.047244094488181343 ) ) ;
#8964 = ORIENTED_EDGE ( 'NONE', *, *, #43080, .T. ) ;
#8965 = VECTOR ( 'NONE', #2480, 39.37007874015748143 ) ;
#8966 = DIRECTION ( 'NONE',  ( -0.9998717552508122886, -0.01601477604151185785, 0.000000000000000000 ) ) ;
#8967 = VERTEX_POINT ( 'NONE', #34080 ) ;
#8968 = CARTESIAN_POINT ( 'NONE',  ( -1.985260859929297572, 3.346456692913386100, 0.6299212598425164567 ) ) ;
#8969 = AXIS2_PLACEMENT_3D ( 'NONE', #36366, #990, #47682 ) ;
#8970 = EDGE_CURVE ( 'NONE', #50620, #46022, #49765, .T. ) ;
#8971 = ORIENTED_EDGE ( 'NONE', *, *, #47467, .F. ) ;
#8972 = PLANE ( 'NONE',  #25752 ) ;
#8973 = ORIENTED_EDGE ( 'NONE', *, *, #22221, .F. ) ;
#8974 = EDGE_CURVE ( 'NONE', #44686, #36221, #29105, .T. ) ;
#8975 = CARTESIAN_POINT ( 'NONE',  ( -2.454875160333845674, 0.000000000000000000, 0.1574803149606286423 ) ) ;
#8976 = EDGE_LOOP ( 'NONE', ( #19644, #23737, #2438, #28678 ) ) ;
#8977 = CARTESIAN_POINT ( 'NONE',  ( 1.152895553066221268, 6.692913385826772199, -1.833672301139072758 ) ) ;
#8978 = VECTOR ( 'NONE', #12841, 39.37007874015748143 ) ;
#8979 = ADVANCED_FACE ( 'NONE', ( #10581 ), #6706, .T. ) ;
#8980 = ORIENTED_EDGE ( 'NONE', *, *, #27, .F. ) ;
#8981 = ORIENTED_EDGE ( 'NONE', *, *, #16332, .T. ) ;
#8982 = CARTESIAN_POINT ( 'NONE',  ( -0.5455278134075214336, 3.267716535433071279, -1.141732283464563791 ) ) ;
#8983 = ORIENTED_EDGE ( 'NONE', *, *, #4709, .F. ) ;
#8984 = CARTESIAN_POINT ( 'NONE',  ( 0.5455278134075212115, 0.000000000000000000, -0.9448818897637765168 ) ) ;
#8985 = EDGE_CURVE ( 'NONE', #7934, #45264, #37307, .T. ) ;
#8986 = ORIENTED_EDGE ( 'NONE', *, *, #20762, .F. ) ;
#8987 = DIRECTION ( 'NONE',  ( -0.000000000000000000, 1.000000000000000000, -0.000000000000000000 ) ) ;
#8988 = CARTESIAN_POINT ( 'NONE',  ( -0.6214413264104945434, 3.267716535433071279, -0.03937007874015895081 ) ) ;
#8989 = VECTOR ( 'NONE', #48799, 39.37007874015748143 ) ;
#8990 = CIRCLE ( 'NONE', #27140, 2.246510896728926010 ) ;
#8991 = B_SPLINE_CURVE_WITH_KNOTS ( 'NONE', 3,
 ( #38028, #10655, #6774, #37775 ),
 .UNSPECIFIED., .F., .F.,
 ( 4, 4 ),
 ( 0.001423630509341207613, 0.04645086268844192401 ),
 .UNSPECIFIED. ) ;
#8992 = LINE ( 'NONE', #476, #2511 ) ;
#8993 = PRESENTATION_LAYER_ASSIGNMENT (  '', '', ( #46045 ) ) ;
#8994 = VERTEX_POINT ( 'NONE', #41065 ) ;
#8995 = CARTESIAN_POINT ( 'NONE',  ( -0.2727639067037602727, 3.346456692913386100, 1.220472440944875281 ) ) ;
#8996 = CARTESIAN_POINT ( 'NONE',  ( 1.281152772984938126, 5.905511811023623991, -2.660341145381147854 ) ) ;
#8997 = CARTESIAN_POINT ( 'NONE',  ( 0.7423782071083087075, 0.000000000000000000, 0.6299212598425161236 ) ) ;
#8998 = PLANE ( 'NONE',  #49672 ) ;
#8999 = EDGE_CURVE ( 'NONE', #21605, #1831, #1923, .T. ) ;
#9000 = AXIS2_PLACEMENT_3D ( 'NONE', #31607, #15848, #43463 ) ;
#9001 = CARTESIAN_POINT ( 'NONE',  ( -0.6380732109764247761, 1.697682040615038801, -2.127022210610377773 ) ) ;
#9002 = ADVANCED_FACE ( 'NONE', ( #50269 ), #3330, .F. ) ;
#9003 = PLANE ( 'NONE',  #19834 ) ;
#9004 = LINE ( 'NONE', #24241, #19357 ) ;
#9005 = ORIENTED_EDGE ( 'NONE', *, *, #10519, .F. ) ;
#9006 = CARTESIAN_POINT ( 'NONE',  ( -0.3937007874015748254, 3.248031496062991685, -2.362204724409448620 ) ) ;
#9007 = DIRECTION ( 'NONE',  ( -0.000000000000000000, -1.000000000000000000, -0.000000000000000000 ) ) ;
#9008 = EDGE_LOOP ( 'NONE', ( #32200, #31912, #18041, #30567 ) ) ;
#9009 = FACE_BOUND ( 'NONE', #16333, .T. ) ;
#9010 = ORIENTED_EDGE ( 'NONE', *, *, #18749, .T. ) ;
#9011 = DIRECTION ( 'NONE',  ( -0.000000000000000000, 0.000000000000000000, 1.000000000000000000 ) ) ;
#9012 = ADVANCED_FACE ( 'NONE', ( #22705 ), #26675, .T. ) ;
#9013 = CARTESIAN_POINT ( 'NONE',  ( -1.700636463192204628, 0.000000000000000000, -0.4049693226113392219 ) ) ;
#9014 = CARTESIAN_POINT ( 'NONE',  ( 1.091055626815042423, 0.000000000000000000, -1.771653543307081691 ) ) ;
#9015 = DIRECTION ( 'NONE',  ( -1.000000000000000000, 0.000000000000000000, 1.734723475976806848E-16 ) ) ;
#9016 = FACE_OUTER_BOUND ( 'NONE', #21534, .T. ) ;
#9017 = AXIS2_PLACEMENT_3D ( 'NONE', #31312, #16325, #47261 ) ;
#9018 = EDGE_LOOP ( 'NONE', ( #4880, #37174, #273, #32861 ) ) ;
#9019 = ADVANCED_FACE ( 'NONE', ( #22956 ), #7458, .F. ) ;
#9020 = CARTESIAN_POINT ( 'NONE',  ( 1.461782879395302048, 1.205361022782829114E-17, -1.598346982901808211 ) ) ;
#9021 = DIRECTION ( 'NONE',  ( 0.3513748240813304724, 0.000000000000000000, 0.9362348706397417564 ) ) ;
#9022 = VERTEX_POINT ( 'NONE', #18584 ) ;
#9023 = CARTESIAN_POINT ( 'NONE',  ( -1.166969139818015533, 0.000000000000000000, 1.417322834645662777 ) ) ;
#9024 = ORIENTED_EDGE ( 'NONE', *, *, #28463, .T. ) ;
#9025 = VECTOR ( 'NONE', #49573, 39.37007874015748143 ) ;
#9026 = CARTESIAN_POINT ( 'NONE',  ( -1.195183497228115035E-16, 0.000000000000000000, -1.259842519685035134 ) ) ;
#9027 = DIRECTION ( 'NONE',  ( -1.000000000000000000, 0.000000000000000000, 1.734723475976806848E-16 ) ) ;
#9028 = VECTOR ( 'NONE', #18481, 39.37007874015748143 ) ;
#9029 = CARTESIAN_POINT ( 'NONE',  ( 1.636583440222563635, 3.346456692913386100, -1.259842519685035800 ) ) ;
#9030 = ORIENTED_EDGE ( 'NONE', *, *, #22981, .T. ) ;
#9031 = ORIENTED_EDGE ( 'NONE', *, *, #36870, .T. ) ;
#9032 = LINE ( 'NONE', #40530, #2095 ) ;
#9033 = CARTESIAN_POINT ( 'NONE',  ( -1.439733046521776361, 3.346456692913386100, 0.1181102362204704270 ) ) ;
#9034 = FACE_BOUND ( 'NONE', #47534, .T. ) ;
#9035 = AXIS2_PLACEMENT_3D ( 'NONE', #27915, #19904, #11917 ) ;
#9036 = CARTESIAN_POINT ( 'NONE',  ( 0.1067246931122726866, 0.02962905676920215767, 0.000000000000000000 ) ) ;
#9037 = CARTESIAN_POINT ( 'NONE',  ( -0.8182917201112814842, 0.000000000000000000, 1.417322834645662777 ) ) ;
#9038 = ADVANCED_FACE ( 'NONE', ( #23197 ), #33297, .F. ) ;
#9039 = ORIENTED_EDGE ( 'NONE', *, *, #14212, .F. ) ;
#9040 = CARTESIAN_POINT ( 'NONE',  ( -0.7874015748031495399, 0.000000000000000000, -1.220472440944881942 ) ) ;
#9041 = VERTEX_POINT ( 'NONE', #38709 ) ;
#9042 = ORIENTED_EDGE ( 'NONE', *, *, #20849, .T. ) ;
#9043 = EDGE_CURVE ( 'NONE', #36095, #24457, #39057, .T. ) ;
#9044 = ORIENTED_EDGE ( 'NONE', *, *, #49482, .F. ) ;
#9045 = CARTESIAN_POINT ( 'NONE',  ( 1.091055626815043311, 3.267716535433071279, 1.692913385826762873 ) ) ;
#9046 = DIRECTION ( 'NONE',  ( 0.000000000000000000, 0.000000000000000000, 1.000000000000000000 ) ) ;
#9047 = ADVANCED_FACE ( 'NONE', ( #34830 ), #30958, .F. ) ;
#9048 = CIRCLE ( 'NONE', #51031, 1.850107469027523432 ) ;
#9049 = EDGE_CURVE ( 'NONE', #16457, #22729, #13495, .T. ) ;
#9050 = DIRECTION ( 'NONE',  ( -3.469446951953613696E-16, 0.000000000000000000, -1.000000000000000000 ) ) ;
#9051 = CARTESIAN_POINT ( 'NONE',  ( 0.000000000000000000, 3.267716535433071279, -1.102362204724405714 ) ) ;
#9052 = ORIENTED_EDGE ( 'NONE', *, *, #17304, .T. ) ;
#9053 = ORIENTED_EDGE ( 'NONE', *, *, #22560, .T. ) ;
#9054 = B_SPLINE_CURVE_WITH_KNOTS ( 'NONE', 3,
 ( #3115, #2866, #14745, #46202 ),
 .UNSPECIFIED., .F., .F.,
 ( 4, 4 ),
 ( 2.272220830976737561E-07, 0.01613183417298772598 ),
 .UNSPECIFIED. ) ;
#9055 = CARTESIAN_POINT ( 'NONE',  ( 1.833433833923350909, 3.267716535433071279, 1.152076279655074087 ) ) ;
#9056 = DIRECTION ( 'NONE',  ( -3.469446951953613696E-16, 0.000000000000000000, -1.000000000000000000 ) ) ;
#9057 = CARTESIAN_POINT ( 'NONE',  ( 0.1968503937007873017, 0.000000000000000000, 0.6299212598425161236 ) ) ;
#9058 = CARTESIAN_POINT ( 'NONE',  ( 1.514466370292996800, 0.000000000000000000, 2.534789744887420149 ) ) ;
#9059 = LINE ( 'NONE', #1571, #47815 ) ;
#9060 = AXIS2_PLACEMENT_3D ( 'NONE', #8481, #11834, #24230 ) ;
#9061 = CARTESIAN_POINT ( 'NONE',  ( -2.307846990702095535, 2.755905511811027164, -0.8016101313716829102 ) ) ;
#9062 = EDGE_CURVE ( 'NONE', #5044, #49731, #21105, .T. ) ;
#9063 = LINE ( 'NONE', #21199, #40732 ) ;
#9064 = ORIENTED_EDGE ( 'NONE', *, *, #40711, .T. ) ;
#9065 = LINE ( 'NONE', #9578, #44841 ) ;
#9066 = DIRECTION ( 'NONE',  ( 1.734723475976806848E-16, -0.000000000000000000, 1.000000000000000000 ) ) ;
#9067 = AXIS2_PLACEMENT_3D ( 'NONE', #41662, #10419, #30547 ) ;
#9068 = ORIENTED_EDGE ( 'NONE', *, *, #39495, .T. ) ;
#9070 = ORIENTED_EDGE ( 'NONE', *, *, #2538, .F. ) ;
#9069 = EDGE_CURVE ( 'NONE', #35441, #16692, #14956, .T. ) ;
#9071 = CARTESIAN_POINT ( 'NONE',  ( 2.889674983507178219, 1.764288196056212454, -0.6090712660037608250 ) ) ;
#9072 = CARTESIAN_POINT ( 'NONE',  ( -0.8329809839909436686, 1.706281419137876565, -2.833254665166566877 ) ) ;
#9073 = ORIENTED_EDGE ( 'NONE', *, *, #27462, .T. ) ;
#9074 = EDGE_CURVE ( 'NONE', #37676, #13035, #27317, .T. ) ;
#9075 = ADVANCED_FACE ( 'NONE', ( #15461 ), #11583, .F. ) ;
#9076 = VERTEX_POINT ( 'NONE', #31463 ) ;
#9077 = CARTESIAN_POINT ( 'NONE',  ( 2.121469926805689354, 5.905511811023623991, -0.4337334748181388977 ) ) ;
#9078 = EDGE_LOOP ( 'NONE', ( #8755, #22675, #17088, #27288 ) ) ;
#9079 = ORIENTED_EDGE ( 'NONE', *, *, #13434, .T. ) ;
#9080 = CARTESIAN_POINT ( 'NONE',  ( 0.000000000000000000, 3.267716535433071279, 0.5905511811023582691 ) ) ;
#9081 = DIRECTION ( 'NONE',  ( 1.000000000000000000, 0.000000000000000000, -3.469446951953613696E-16 ) ) ;
#9082 = VERTEX_POINT ( 'NONE', #46666 ) ;
#9083 = VERTEX_POINT ( 'NONE', #11334 ) ;
#9084 = ORIENTED_EDGE ( 'NONE', *, *, #39592, .F. ) ;
#9085 = DIRECTION ( 'NONE',  ( -3.469446951953613696E-16, 0.000000000000000000, -1.000000000000000000 ) ) ;
#9086 = VERTEX_POINT ( 'NONE', #43062 ) ;
#9087 = ORIENTED_EDGE ( 'NONE', *, *, #13398, .T. ) ;
#9088 = LINE ( 'NONE', #36723, #44600 ) ;
#9089 = DIRECTION ( 'NONE',  ( -0.000000000000000000, 0.000000000000000000, 1.000000000000000000 ) ) ;
#9090 = DIRECTION ( 'NONE',  ( -0.000000000000000000, 0.000000000000000000, 1.000000000000000000 ) ) ;
#9091 = VECTOR ( 'NONE', #39463, 39.37007874015748143 ) ;
#9092 = ORIENTED_EDGE ( 'NONE', *, *, #1904, .F. ) ;
#9093 = VECTOR ( 'NONE', #12466, 39.37007874015748143 ) ;
#9094 = DIRECTION ( 'NONE',  ( 0.000000000000000000, 1.160734090543304660E-16, -1.000000000000000000 ) ) ;
#9095 = LINE ( 'NONE', #5478, #6072 ) ;
#9096 = PLANE ( 'NONE',  #11335 ) ;
#9097 = ORIENTED_EDGE ( 'NONE', *, *, #30234, .T. ) ;
#9098 = CARTESIAN_POINT ( 'NONE',  ( 0.08139965876239094178, 1.610780518492231694, 0.000000000000000000 ) ) ;
#9099 = FACE_OUTER_BOUND ( 'NONE', #48031, .T. ) ;
#9100 = CARTESIAN_POINT ( 'NONE',  ( 2.867773316779195447, 1.449472587384593725, -0.7050287376752005786 ) ) ;
#9101 = VERTEX_POINT ( 'NONE', #27067 ) ;
#9102 = ORIENTED_EDGE ( 'NONE', *, *, #40136, .T. ) ;
#9103 = VECTOR ( 'NONE', #10046, 39.37007874015748143 ) ;
#9104 = DIRECTION ( 'NONE',  ( -1.000000000000000000, 0.000000000000000000, -0.000000000000000000 ) ) ;
#9105 = CARTESIAN_POINT ( 'NONE',  ( 0.5455278134075208785, 0.000000000000000000, -1.574803149606293529 ) ) ;
#9106 = FACE_OUTER_BOUND ( 'NONE', #33349, .T. ) ;
#9107 = EDGE_CURVE ( 'NONE', #20582, #2274, #3586, .T. ) ;
#9108 = EDGE_CURVE ( 'NONE', #34031, #40030, #42314, .T. ) ;
#9109 = DIRECTION ( 'NONE',  ( -0.000000000000000000, 1.000000000000000000, -0.000000000000000000 ) ) ;
#9110 = DIRECTION ( 'NONE',  ( -0.000000000000000000, 1.000000000000000000, -0.000000000000000000 ) ) ;
#9111 = VERTEX_POINT ( 'NONE', #11833 ) ;
#9113 = EDGE_CURVE ( 'NONE', #36589, #8562, #51019, .T. ) ;
#9112 = ORIENTED_EDGE ( 'NONE', *, *, #142, .F. ) ;
#9114 = CARTESIAN_POINT ( 'NONE',  ( 2.793030215715258446, 1.664308485742666877, 0.9592557174602684977 ) ) ;
#9115 = ORIENTED_EDGE ( 'NONE', *, *, #5511, .F. ) ;
#9116 = LINE ( 'NONE', #17631, #38159 ) ;
#9117 = DIRECTION ( 'NONE',  ( 0.000000000000000000, 0.000000000000000000, -1.000000000000000000 ) ) ;
#9118 = ADVANCED_FACE ( 'NONE', ( #24740 ), #23965, .F. ) ;
#9119 = CARTESIAN_POINT ( 'NONE',  ( 0.000000000000000000, 3.313179664429866556, -2.422428857167389982 ) ) ;
#9121 = CARTESIAN_POINT ( 'NONE',  ( -0.7145799201509074328, 1.574803149606302854, 2.044048657746648789 ) ) ;
#9120 = APPLICATION_CONTEXT ( 'automotive_design' ) ;
#9122 = CARTESIAN_POINT ( 'NONE',  ( 2.061875708210571201, 1.740926663775191674, 1.053657044629532802 ) ) ;
#9123 = ORIENTED_EDGE ( 'NONE', *, *, #40195, .T. ) ;
#9124 = CARTESIAN_POINT ( 'NONE',  ( 0.7423782071083084855, 3.267716535433071279, -1.889763779527552812 ) ) ;
#9125 = EDGE_CURVE ( 'NONE', #48261, #11767, #36103, .T. ) ;
#9126 = DIRECTION ( 'NONE',  ( 0.000000000000000000, 1.160734090543304660E-16, -1.000000000000000000 ) ) ;
#9127 = VECTOR ( 'NONE', #26206, 39.37007874015748143 ) ;
#9128 = ORIENTED_EDGE ( 'NONE', *, *, #31110, .F. ) ;
#9129 = CARTESIAN_POINT ( 'NONE',  ( 0.8952071785065209841, 5.905511811023623991, 1.972340328593148007 ) ) ;
#9130 = EDGE_CURVE ( 'NONE', #29370, #45283, #213, .T. ) ;
#9131 = AXIS2_PLACEMENT_3D ( 'NONE', #47891, #8190, #44050 ) ;
#9132 = LINE ( 'NONE', #12240, #4702 ) ;
#9133 = CARTESIAN_POINT ( 'NONE',  ( 0.000000000000000000, 6.692913385826772199, 0.000000000000000000 ) ) ;
#9134 = ORIENTED_EDGE ( 'NONE', *, *, #13778, .T. ) ;
#9135 = CARTESIAN_POINT ( 'NONE',  ( -1.091055626815042645, 3.346456692913386100, -2.086614173228339641 ) ) ;
#9136 = EDGE_CURVE ( 'NONE', #46482, #30180, #28601, .T. ) ;
#9137 = CARTESIAN_POINT ( 'NONE',  ( 0.4696143004045483793, 3.267716535433071279, -1.629301903132388985E-16 ) ) ;
#9138 = EDGE_CURVE ( 'NONE', #36547, #12398, #28341, .T. ) ;
#9139 = EDGE_LOOP ( 'NONE', ( #3163, #248 ) ) ;
#9140 = CARTESIAN_POINT ( 'NONE',  ( 0.7423782071083082634, 3.267716535433071279, -1.771653543307081025 ) ) ;
#9141 = VECTOR ( 'NONE', #32736, 39.37007874015748143 ) ;
#9142 = DIRECTION ( 'NONE',  ( -1.000000000000000000, 0.000000000000000000, 0.000000000000000000 ) ) ;
#9143 = ORIENTED_EDGE ( 'NONE', *, *, #39612, .F. ) ;
#9144 = EDGE_CURVE ( 'NONE', #19095, #8962, #42334, .T. ) ;
#9145 = FACE_OUTER_BOUND ( 'NONE', #35424, .T. ) ;
#9146 = DIRECTION ( 'NONE',  ( -8.032339854997315857E-17, 1.000000000000000000, -1.007223559679407077E-16 ) ) ;
#9147 = CARTESIAN_POINT ( 'NONE',  ( -1.712496953225537633, 3.267716535433071279, -0.4724409448818884805 ) ) ;
#9148 = DIRECTION ( 'NONE',  ( 0.000000000000000000, 0.000000000000000000, 1.000000000000000000 ) ) ;
#9149 = DIRECTION ( 'NONE',  ( 0.000000000000000000, 0.000000000000000000, -1.000000000000000000 ) ) ;
#9150 = ORIENTED_EDGE ( 'NONE', *, *, #5384, .F. ) ;
#9151 = EDGE_LOOP ( 'NONE', ( #44943, #41085, #26564, #5646 ) ) ;
#9152 = CARTESIAN_POINT ( 'NONE',  ( 0.4696143004045479352, 3.346456692913386100, 0.7874015748031454320 ) ) ;
#9153 = B_SPLINE_CURVE_WITH_KNOTS ( 'NONE', 3,
 ( #49057, #1608, #13236, #20975 ),
 .UNSPECIFIED., .F., .F.,
 ( 4, 4 ),
 ( 2.895195689601480918E-07, 0.01652376043565199903 ),
 .UNSPECIFIED. ) ;
#9154 = LINE ( 'NONE', #13033, #9797 ) ;
#9155 = ORIENTED_EDGE ( 'NONE', *, *, #31235, .F. ) ;
#9156 = CARTESIAN_POINT ( 'NONE',  ( 0.8182917201112819283, 0.000000000000000000, -0.7874015748031473194 ) ) ;
#9157 = CARTESIAN_POINT ( 'NONE',  ( 1.363819533518803251, 0.000000000000000000, -0.7874015748031473194 ) ) ;
#9158 = DIRECTION ( 'NONE',  ( 1.000000000000000000, 0.000000000000000000, -3.469446951953613696E-16 ) ) ;
#9159 = DIRECTION ( 'NONE',  ( 0.000000000000000000, 0.000000000000000000, -1.000000000000000000 ) ) ;
#9160 = ORIENTED_EDGE ( 'NONE', *, *, #7676, .T. ) ;
#9161 = ORIENTED_EDGE ( 'NONE', *, *, #47787, .F. ) ;
#9162 = B_SPLINE_CURVE_WITH_KNOTS ( 'NONE', 3,
 ( #40103, #20473, #4731, #28464 ),
 .UNSPECIFIED., .F., .F.,
 ( 4, 4 ),
 ( 2.102951557409031314E-07, 0.002500239225155444656 ),
 .UNSPECIFIED. ) ;
#9163 = CARTESIAN_POINT ( 'NONE',  ( 0.000000000000000000, 0.07874015748031502893, 0.000000000000000000 ) ) ;
#9164 = DIRECTION ( 'NONE',  ( -1.000000000000000000, 0.000000000000000000, 0.000000000000000000 ) ) ;
#9165 = CARTESIAN_POINT ( 'NONE',  ( -2.454875160333845674, 3.232777166330581320, 0.1574803149606286423 ) ) ;
#9166 = ORIENTED_EDGE ( 'NONE', *, *, #8970, .T. ) ;
#9167 = DIRECTION ( 'NONE',  ( 1.000000000000000000, 0.000000000000000000, -3.469446951953613696E-16 ) ) ;
#9168 = FACE_BOUND ( 'NONE', #7533, .T. ) ;
#9169 = VERTEX_POINT ( 'NONE', #984 ) ;
#9170 = CARTESIAN_POINT ( 'NONE',  ( 0.1170985530868079300, 0.02979521312206013725, -1.850078377359382298 ) ) ;
#9171 = ORIENTED_EDGE ( 'NONE', *, *, #45402, .F. ) ;
#9172 = ORIENTED_EDGE ( 'NONE', *, *, #33648, .T. ) ;
#9173 = CARTESIAN_POINT ( 'NONE',  ( -2.101391096692225791, 1.575819129783617489, -0.5301069970517552354 ) ) ;
#9174 = VECTOR ( 'NONE', #14204, 39.37007874015748143 ) ;
#9175 = VECTOR ( 'NONE', #21225, 39.37007874015748143 ) ;
#9176 = ORIENTED_EDGE ( 'NONE', *, *, #40309, .F. ) ;
#9177 = CARTESIAN_POINT ( 'NONE',  ( 0.3129956986666029839, 1.049866565877818347, 2.000361441378088578 ) ) ;
#9178 = UNCERTAINTY_MEASURE_WITH_UNIT (LENGTH_MEASURE( 1.000000000000000082E-05 ), #50817, 'distance_accuracy_value', 'NONE');
#9179 = VERTEX_POINT ( 'NONE', #31720 ) ;
#9180 = EDGE_CURVE ( 'NONE', #31704, #10848, #12096, .T. ) ;
#9181 = EDGE_CURVE ( 'NONE', #30078, #14009, #8225, .T. ) ;
#9182 = B_SPLINE_CURVE_WITH_KNOTS ( 'NONE', 3,
 ( #50404, #42946, #22843, #7598 ),
 .UNSPECIFIED., .F., .F.,
 ( 4, 4 ),
 ( 0.01346820720327507846, 0.03074302814991078381 ),
 .UNSPECIFIED. ) ;
#9183 = DIRECTION ( 'NONE',  ( -0.9009688679024154823, 1.288287287306305283E-16, -0.4338837391175656699 ) ) ;
#9184 = CARTESIAN_POINT ( 'NONE',  ( 0.2727639067037604392, 3.346456692913386100, -0.6692913385826760875 ) ) ;
#9185 = ADVANCED_FACE ( 'NONE', ( #731 ), #47420, .F. ) ;
#9186 = DIRECTION ( 'NONE',  ( -3.469446951953613696E-16, 0.000000000000000000, -1.000000000000000000 ) ) ;
#9187 = VECTOR ( 'NONE', #38602, 39.37007874015748143 ) ;
#9188 = CARTESIAN_POINT ( 'NONE',  ( 4.268512490100411402E-16, 3.346456692913386100, 0.9448818897637749625 ) ) ;
#9189 = CARTESIAN_POINT ( 'NONE',  ( 1.062992125984251413, 0.000000000000000000, -1.181102362204724754 ) ) ;
#9190 = CARTESIAN_POINT ( 'NONE',  ( 0.04921259842519669359, 1.610264983814881479, 2.246280244424690320 ) ) ;
#9191 = ORIENTED_EDGE ( 'NONE', *, *, #32370, .F. ) ;
#9192 = CARTESIAN_POINT ( 'NONE',  ( 0.000000000000000000, 1.574803149606302854, 0.000000000000000000 ) ) ;
#9193 = DIRECTION ( 'NONE',  ( 1.000000000000000000, 0.000000000000000000, -3.469446951953613696E-16 ) ) ;
#9194 = ORIENTED_EDGE ( 'NONE', *, *, #30228, .T. ) ;
#9195 = CARTESIAN_POINT ( 'NONE',  ( -1.363819533518803029, 0.000000000000000000, 1.417322834645662777 ) ) ;
#9196 = ADVANCED_FACE ( 'NONE', ( #32236 ), #28084, .T. ) ;
#9197 = PLANE ( 'NONE',  #27763 ) ;
#9198 = ORIENTED_EDGE ( 'NONE', *, *, #44323, .T. ) ;
#9199 = CARTESIAN_POINT ( 'NONE',  ( -2.102985103392958077, 3.346456692913386100, 0.1181102362204704270 ) ) ;
#9200 = CARTESIAN_POINT ( 'NONE',  ( 1.636583440222563635, 3.267716535433071279, -2.839019714148966584E-16 ) ) ;
#9201 = DIRECTION ( 'NONE',  ( 0.9510565162951500895, 0.000000000000000000, 0.3090169943749582204 ) ) ;
#9202 = ADVANCED_FACE ( 'NONE', ( #16484 ), #8480, .F. ) ;
#9203 = EDGE_CURVE ( 'NONE', #43398, #17597, #40234, .T. ) ;
#9204 = ORIENTED_EDGE ( 'NONE', *, *, #18050, .T. ) ;
#9205 = DIRECTION ( 'NONE',  ( 0.000000000000000000, 1.000000000000000000, 0.000000000000000000 ) ) ;
#9206 = ORIENTED_EDGE ( 'NONE', *, *, #36351, .T. ) ;
#9207 = FACE_BOUND ( 'NONE', #17094, .T. ) ;
#9208 = FACE_OUTER_BOUND ( 'NONE', #24919, .T. ) ;
#9209 = AXIS2_PLACEMENT_3D ( 'NONE', #14848, #33971, #2974 ) ;
#9210 = VECTOR ( 'NONE', #40421, 39.37007874015748143 ) ;
#9211 = CARTESIAN_POINT ( 'NONE',  ( 1.672606463373375485, 0.000000000000000000, 0.4917175957957914401 ) ) ;
#9212 = LINE ( 'NONE', #17467, #23465 ) ;
#9213 = AXIS2_PLACEMENT_3D ( 'NONE', #18988, #34742, #11249 ) ;
#9214 = VERTEX_POINT ( 'NONE', #8988 ) ;
#9215 = ORIENTED_EDGE ( 'NONE', *, *, #37477, .T. ) ;
#9216 = FACE_OUTER_BOUND ( 'NONE', #41309, .T. ) ;
#9217 = ORIENTED_EDGE ( 'NONE', *, *, #30917, .T. ) ;
#9218 = VECTOR ( 'NONE', #25796, 39.37007874015748143 ) ;
#9219 = DIRECTION ( 'NONE',  ( 1.734723475976806848E-16, -0.000000000000000000, 1.000000000000000000 ) ) ;
#9220 = ORIENTED_EDGE ( 'NONE', *, *, #36311, .F. ) ;
#9221 = LINE ( 'NONE', #16721, #42121 ) ;
#9222 = VERTEX_POINT ( 'NONE', #15961 ) ;
#9223 = PLANE ( 'NONE',  #4339 ) ;
#9224 = B_SPLINE_CURVE_WITH_KNOTS ( 'NONE', 3,
 ( #10665, #6787, #10910, #50591 ),
 .UNSPECIFIED., .F., .F.,
 ( 4, 4 ),
 ( 2.397469164285932143E-07, 0.01629908605468858088 ),
 .UNSPECIFIED. ) ;
#9225 = DIRECTION ( 'NONE',  ( 0.000000000000000000, 0.000000000000000000, -1.000000000000000000 ) ) ;
#9226 = ORIENTED_EDGE ( 'NONE', *, *, #4174, .T. ) ;
#9227 = LINE ( 'NONE', #28844, #43837 ) ;
#9228 = ORIENTED_EDGE ( 'NONE', *, *, #45974, .F. ) ;
#9229 = EDGE_LOOP ( 'NONE', ( #46804, #46714, #33245, #1498 ) ) ;
#9230 = VERTEX_POINT ( 'NONE', #12604 ) ;
#9231 = ORIENTED_EDGE ( 'NONE', *, *, #38783, .T. ) ;
#9232 = DIRECTION ( 'NONE',  ( 0.000000000000000000, 0.000000000000000000, 1.000000000000000000 ) ) ;
#9233 = CARTESIAN_POINT ( 'NONE',  ( -1.091055626815042645, 3.346456692913386100, -1.771653543307081025 ) ) ;
#9234 = ADVANCED_FACE ( 'NONE', ( #40488 ), #44799, .T. ) ;
#9235 = EDGE_CURVE ( 'NONE', #30696, #1746, #39373, .T. ) ;
#9236 = ORIENTED_EDGE ( 'NONE', *, *, #37064, .T. ) ;
#9237 = B_SPLINE_CURVE_WITH_KNOTS ( 'NONE', 3,
 ( #42564, #3323, #15199, #30950 ),
 .UNSPECIFIED., .F., .F.,
 ( 4, 4 ),
 ( 0.1211775127643062860, 0.1625894504277921315 ),
 .UNSPECIFIED. ) ;
#9238 = DIRECTION ( 'NONE',  ( -3.469446951953613696E-16, 0.000000000000000000, -1.000000000000000000 ) ) ;
#9239 = EDGE_LOOP ( 'NONE', ( #11923, #27867, #34400, #18915 ) ) ;
#9240 = CARTESIAN_POINT ( 'NONE',  ( -1.536664496436148184E-16, 3.267716535433071279, 0.4330708661417287386 ) ) ;
#9241 = EDGE_CURVE ( 'NONE', #40528, #12432, #27234, .T. ) ;
#9242 = VECTOR ( 'NONE', #36222, 39.37007874015748143 ) ;
#9243 = EDGE_CURVE ( 'NONE', #21615, #5817, #8133, .T. ) ;
#9244 = EDGE_CURVE ( 'NONE', #46444, #33470, #15379, .T. ) ;
#9245 = CARTESIAN_POINT ( 'NONE',  ( -1.363819533518803029, 3.267716535433071279, 0.4724409448818871482 ) ) ;
#9246 = EDGE_LOOP ( 'NONE', ( #13296, #11006, #43603, #4301 ) ) ;
#9247 = AXIS2_PLACEMENT_3D ( 'NONE', #35066, #14936, #3063 ) ;
#9248 = DIRECTION ( 'NONE',  ( -0.000000000000000000, 1.000000000000000000, -0.000000000000000000 ) ) ;
#9249 = DIRECTION ( 'NONE',  ( -1.000000000000000000, 0.000000000000000000, 1.734723475976806848E-16 ) ) ;
#9250 = LINE ( 'NONE', #36881, #30736 ) ;
#9251 = PLANE ( 'NONE',  #26639 ) ;
#9252 = VECTOR ( 'NONE', #50944, 39.37007874015748143 ) ;
#9253 = CARTESIAN_POINT ( 'NONE',  ( -2.097080421798980687, 3.346456692913386100, -0.1968503937007880511 ) ) ;
#9254 = CARTESIAN_POINT ( 'NONE',  ( -1.091055626815042645, 3.267716535433071279, -1.771653543307081025 ) ) ;
#9255 = AXIS2_PLACEMENT_3D ( 'NONE', #46375, #11039, #50472 ) ;
#9256 = DIRECTION ( 'NONE',  ( 0.8805955318567391110, 0.000000000000000000, -0.4738686624729965269 ) ) ;
#9257 = EDGE_CURVE ( 'NONE', #30941, #16203, #48895, .T. ) ;
#9258 = ORIENTED_EDGE ( 'NONE', *, *, #10466, .T. ) ;
#9259 = DIRECTION ( 'NONE',  ( -0.01601477604151182663, 0.9998717552508123996, -0.000000000000000000 ) ) ;
#9260 = CARTESIAN_POINT ( 'NONE',  ( 2.793030215715258446, 1.762782749918499814, 0.9592557174602684977 ) ) ;
#9261 = ORIENTED_EDGE ( 'NONE', *, *, #48062, .F. ) ;
#9262 = CARTESIAN_POINT ( 'NONE',  ( 0.000000000000000000, 3.267716535433071279, 0.1181102362204704270 ) ) ;
#9263 = EDGE_CURVE ( 'NONE', #24903, #10800, #35744, .T. ) ;
#9264 = EDGE_LOOP ( 'NONE', ( #25332, #4092, #13393, #38139 ) ) ;
#9265 = CARTESIAN_POINT ( 'NONE',  ( 0.000000000000000000, 3.267716535433071279, 0.000000000000000000 ) ) ;
#9266 = CARTESIAN_POINT ( 'NONE',  ( -2.867773316779185677, 1.674559808355669199, -0.7050287376752426560 ) ) ;
#9267 = LINE ( 'NONE', #25774, #48438 ) ;
#9268 = FACE_OUTER_BOUND ( 'NONE', #14176, .T. ) ;
#9269 = DIRECTION ( 'NONE',  ( -3.469446951953613696E-16, 0.000000000000000000, -1.000000000000000000 ) ) ;
#9270 = ORIENTED_EDGE ( 'NONE', *, *, #38742, .F. ) ;
#9271 = EDGE_CURVE ( 'NONE', #43549, #7899, #7377, .T. ) ;
#9272 = CARTESIAN_POINT ( 'NONE',  ( 0.1067246931122726866, 0.02962905676920215767, 0.000000000000000000 ) ) ;
#9273 = FACE_BOUND ( 'NONE', #43750, .T. ) ;
#9274 = ORIENTED_EDGE ( 'NONE', *, *, #46181, .T. ) ;
#9275 = DIRECTION ( 'NONE',  ( -0.000000000000000000, 0.000000000000000000, 1.000000000000000000 ) ) ;
#9276 = EDGE_CURVE ( 'NONE', #19355, #41467, #7127, .T. ) ;
#9277 = ORIENTED_EDGE ( 'NONE', *, *, #46965, .F. ) ;
#9278 = CARTESIAN_POINT ( 'NONE',  ( 2.074049943651431693, 1.574803149606302854, 0.6221544894624233546 ) ) ;
#9279 = CARTESIAN_POINT ( 'NONE',  ( 1.181102362204724532, 0.4724409448818893686, 1.062992125984251413 ) ) ;
#9280 = AXIS2_PLACEMENT_3D ( 'NONE', #3132, #50560, #34629 ) ;
#9281 = CARTESIAN_POINT ( 'NONE',  ( -2.182111253630085290, 0.000000000000000000, -0.1968503937007880511 ) ) ;
#9282 = AXIS2_PLACEMENT_3D ( 'NONE', #17989, #40986, #41739 ) ;
#9283 = CARTESIAN_POINT ( 'NONE',  ( -2.150703319933163993, 1.607838006543269804, -0.2514661222534355645 ) ) ;
#9284 = ORIENTED_EDGE ( 'NONE', *, *, #33519, .T. ) ;
#9285 = VERTEX_POINT ( 'NONE', #50676 ) ;
#9286 = CARTESIAN_POINT ( 'NONE',  ( 0.1968503937007873017, 0.000000000000000000, 0.3149606299212576177 ) ) ;
#9288 = PLANE ( 'NONE',  #47940 ) ;
#9287 = CIRCLE ( 'NONE', #15076, 1.850107469027523432 ) ;
#9289 = FACE_BOUND ( 'NONE', #47875, .T. ) ;
#9290 = EDGE_LOOP ( 'NONE', ( #21613, #26165, #21048, #33127 ) ) ;
#9291 = VECTOR ( 'NONE', #20613, 39.37007874015748143 ) ;
#9292 = VECTOR ( 'NONE', #25147, 39.37007874015748143 ) ;
#9293 = LINE ( 'NONE', #48740, #5600 ) ;
#9294 = CARTESIAN_POINT ( 'NONE',  ( -1.636583440222564301, 3.346456692913386100, 1.417869535855831753 ) ) ;
#9295 = ORIENTED_EDGE ( 'NONE', *, *, #1171, .T. ) ;
#9296 = B_SPLINE_CURVE_WITH_KNOTS ( 'NONE', 3,
 ( #26288, #18036, #13656, #6162 ),
 .UNSPECIFIED., .F., .F.,
 ( 4, 4 ),
 ( 0.01171354017532363727, 0.03073678216732763507 ),
 .UNSPECIFIED. ) ;
#9297 = CARTESIAN_POINT ( 'NONE',  ( 0.000000000000000000, 3.267716535433071279, -1.102362204724405714 ) ) ;
#9298 = DIRECTION ( 'NONE',  ( 1.000000000000000000, 0.000000000000000000, -3.469446951953613696E-16 ) ) ;
#9299 = ORIENTED_EDGE ( 'NONE', *, *, #41798, .F. ) ;
#9300 = ORIENTED_EDGE ( 'NONE', *, *, #35855, .F. ) ;
#9301 = ORIENTED_EDGE ( 'NONE', *, *, #14211, .F. ) ;
#9302 = LINE ( 'NONE', #16796, #29263 ) ;
#9303 = EDGE_CURVE ( 'NONE', #42740, #10110, #38620, .T. ) ;
#9304 = CARTESIAN_POINT ( 'NONE',  ( -0.07591351300297333182, 3.346456692913386100, -1.102362204724405714 ) ) ;
#9305 = DIRECTION ( 'NONE',  ( -0.01601477604151182663, 0.9998717552508123996, -0.000000000000000000 ) ) ;
#9306 = EDGE_CURVE ( 'NONE', #26179, #23113, #11251, .T. ) ;
#9307 = DIRECTION ( 'NONE',  ( -3.469446951953613696E-16, 0.000000000000000000, -1.000000000000000000 ) ) ;
#9308 = EDGE_LOOP ( 'NONE', ( #35749, #2639, #25547, #19417 ) ) ;
#9309 = ORIENTED_EDGE ( 'NONE', *, *, #34036, .F. ) ;
#9310 = CARTESIAN_POINT ( 'NONE',  ( 0.000000000000000000, 6.692913385826772199, 0.000000000000000000 ) ) ;
#9311 = CARTESIAN_POINT ( 'NONE',  ( -0.8942052331142549271, 3.267716535433071279, 3.102397620449222481E-16 ) ) ;
#9312 = LINE ( 'NONE', #16287, #44724 ) ;
#9313 = CARTESIAN_POINT ( 'NONE',  ( 0.000000000000000000, 0.000000000000000000, 0.000000000000000000 ) ) ;
#9314 = CARTESIAN_POINT ( 'NONE',  ( 1.363819533518803695, 3.346456692913386100, 1.681890501046755748 ) ) ;
#9315 = DIRECTION ( 'NONE',  ( -1.000000000000000000, -0.000000000000000000, -0.000000000000000000 ) ) ;
#9316 = B_SPLINE_CURVE_WITH_KNOTS ( 'NONE', 3,
 ( #1543, #13417, #13170, #1793 ),
 .UNSPECIFIED., .F., .F.,
 ( 4, 4 ),
 ( 4.217863529357209716E-07, 0.04981117579911063797 ),
 .UNSPECIFIED. ) ;
#9317 = FACE_OUTER_BOUND ( 'NONE', #6957, .T. ) ;
#9318 = CIRCLE ( 'NONE', #1055, 2.165354330708661568 ) ;
#9319 = VERTEX_POINT ( 'NONE', #39628 ) ;
#9320 = DIRECTION ( 'NONE',  ( 0.9998717552508121775, 0.01601477604151182663, 0.000000000000000000 ) ) ;
#9321 = CARTESIAN_POINT ( 'NONE',  ( -0.5455278134075214336, 0.000000000000000000, -0.5118110236220467790 ) ) ;
#9322 = VERTEX_POINT ( 'NONE', #30873 ) ;
#9323 = VECTOR ( 'NONE', #32041, 39.37007874015748143 ) ;
#9324 = ORIENTED_EDGE ( 'NONE', *, *, #31040, .F. ) ;
#9325 = VECTOR ( 'NONE', #49523, 39.37007874015748143 ) ;
#9326 = DIRECTION ( 'NONE',  ( -0.9998717552508122886, -0.01601477604151180928, 0.000000000000000000 ) ) ;
#9327 = CARTESIAN_POINT ( 'NONE',  ( 0.7423782071083087075, 3.346456692913386100, 0.9448818897637746295 ) ) ;
#9328 = ORIENTED_EDGE ( 'NONE', *, *, #74, .F. ) ;
#9329 = EDGE_CURVE ( 'NONE', #17641, #13815, #42483, .T. ) ;
#9330 = VECTOR ( 'NONE', #5574, 39.37007874015748143 ) ;
#9331 = VERTEX_POINT ( 'NONE', #23117 ) ;
#9332 = CARTESIAN_POINT ( 'NONE',  ( 0.7423782071083092626, 3.346456692913386100, 1.889763779527550369 ) ) ;
#9333 = ADVANCED_FACE ( 'NONE', ( #34744 ), #43485, .F. ) ;
#9334 = ORIENTED_EDGE ( 'NONE', *, *, #24265, .F. ) ;
#9335 = LINE ( 'NONE', #29465, #21086 ) ;
#9336 = CARTESIAN_POINT ( 'NONE',  ( -1.744243240276441398, 5.905511811023623991, 1.328042291889479420 ) ) ;
#9337 = EDGE_CURVE ( 'NONE', #6293, #24410, #50184, .T. ) ;
#9338 = ORIENTED_EDGE ( 'NONE', *, *, #39340, .F. ) ;
#9339 = VERTEX_POINT ( 'NONE', #14872 ) ;
#9340 = ORIENTED_EDGE ( 'NONE', *, *, #26647, .T. ) ;
#9341 = LINE ( 'NONE', #1338, #32096 ) ;
#9342 = ORIENTED_EDGE ( 'NONE', *, *, #46744, .F. ) ;
#9343 = ORIENTED_EDGE ( 'NONE', *, *, #21324, .T. ) ;
#9344 = EDGE_CURVE ( 'NONE', #20959, #28842, #30615, .T. ) ;
#9345 = LINE ( 'NONE', #41857, #16581 ) ;
#9346 = CARTESIAN_POINT ( 'NONE',  ( -1.712496953225537188, 3.267716535433071279, 0.7874015748031456541 ) ) ;
#9347 = CARTESIAN_POINT ( 'NONE',  ( 0.002207914879453961969, 6.692913385826772199, 0.04916304461325451958 ) ) ;
#9348 = EDGE_CURVE ( 'NONE', #46386, #7678, #39118, .T. ) ;
#9349 = VERTEX_POINT ( 'NONE', #19489 ) ;
#9350 = CARTESIAN_POINT ( 'NONE',  ( 0.04921259842519667277, 1.720031199985617265, 2.952755905511811108 ) ) ;
#9351 = CARTESIAN_POINT ( 'NONE',  ( 0.4696143004045479352, 3.346456692913386100, -0.4724409448818886470 ) ) ;
#9352 = B_SPLINE_CURVE_WITH_KNOTS ( 'NONE', 3,
 ( #9071, #24820, #20945, #36699 ),
 .UNSPECIFIED., .F., .F.,
 ( 4, 4 ),
 ( 2.052460249050213172E-07, 0.01602278383226833289 ),
 .UNSPECIFIED. ) ;
#9353 = LINE ( 'NONE', #32871, #8008 ) ;
#9354 = EDGE_LOOP ( 'NONE', ( #34514, #19954, #32951, #4161 ) ) ;
#9355 = LINE ( 'NONE', #28965, #9242 ) ;
#9356 = AXIS2_PLACEMENT_3D ( 'NONE', #11379, #38997, #31003 ) ;
#9357 = DIRECTION ( 'NONE',  ( 1.000000000000000000, 0.000000000000000000, -3.469446951953613696E-16 ) ) ;
#9358 = CARTESIAN_POINT ( 'NONE',  ( -0.1450934409768900590, 0.000000000000000000, 2.161127057262024032 ) ) ;
#9359 = ORIENTED_EDGE ( 'NONE', *, *, #28762, .F. ) ;
#9360 = AXIS2_PLACEMENT_3D ( 'NONE', #37025, #18854, #21519 ) ;
#9361 = EDGE_LOOP ( 'NONE', ( #19339, #13414, #24756, #26000 ) ) ;
#9362 = VECTOR ( 'NONE', #39716, 39.37007874015748143 ) ;
#9363 = ADVANCED_FACE ( 'NONE', ( #50930 ), #31378, .F. ) ;
#9364 = AXIS2_PLACEMENT_3D ( 'NONE', #41138, #44981, #25375 ) ;
#9365 = DIRECTION ( 'NONE',  ( 1.000000000000000000, 0.000000000000000000, 0.000000000000000000 ) ) ;
#9366 = PLANE ( 'NONE',  #23651 ) ;
#9367 = ADVANCED_FACE ( 'NONE', ( #23623 ), #35503, .F. ) ;
#9368 = DIRECTION ( 'NONE',  ( -1.000000000000000000, 0.000000000000000000, 0.000000000000000000 ) ) ;
#9369 = VERTEX_POINT ( 'NONE', #31631 ) ;
#9370 = VERTEX_POINT ( 'NONE', #5027 ) ;
#9371 = CIRCLE ( 'NONE', #16780, 2.165354330708661568 ) ;
#9372 = EDGE_CURVE ( 'NONE', #38240, #43935, #45661, .T. ) ;
#9373 = LINE ( 'NONE', #5753, #7761 ) ;
#9374 = ORIENTED_EDGE ( 'NONE', *, *, #2503, .F. ) ;
#9375 = LINE ( 'NONE', #9633, #48008 ) ;
#9376 = DIRECTION ( 'NONE',  ( 0.000000000000000000, 0.000000000000000000, 1.000000000000000000 ) ) ;
#9377 = PLANE ( 'NONE',  #11820 ) ;
#9378 = CARTESIAN_POINT ( 'NONE',  ( 0.4696143004045479352, 3.346456692913386100, -1.417322834645664331 ) ) ;
#9379 = CARTESIAN_POINT ( 'NONE',  ( -1.909347346926324462, 3.346456692913386100, 1.021348170950612255 ) ) ;
#9380 = ORIENTED_EDGE ( 'NONE', *, *, #4250, .T. ) ;
#9381 = DIRECTION ( 'NONE',  ( 0.000000000000000000, 0.7071067811865466846, -0.7071067811865483499 ) ) ;
#9382 = CARTESIAN_POINT ( 'NONE',  ( -2.156388021673881994, 3.267716535433071279, -0.1968503937007880511 ) ) ;
#9383 = EDGE_LOOP ( 'NONE', ( #453, #3562, #48651, #21350 ) ) ;
#9384 = DIRECTION ( 'NONE',  ( 1.000000000000000000, 0.000000000000000000, -3.469446951953613696E-16 ) ) ;
#9385 = DIRECTION ( 'NONE',  ( -1.858431260983764056E-16, 0.7660444431189770143, 0.6427876096865403621 ) ) ;
#9386 = CARTESIAN_POINT ( 'NONE',  ( -0.2727639067037602727, 3.346456692913386100, 0.5905511811023582691 ) ) ;
#9387 = VERTEX_POINT ( 'NONE', #16909 ) ;
#9388 = EDGE_CURVE ( 'NONE', #31953, #25971, #20772, .T. ) ;
#9389 = CARTESIAN_POINT ( 'NONE',  ( 1.236813753895251722, 1.205361022782829114E-17, -2.681693691597563767 ) ) ;
#9390 = FACE_OUTER_BOUND ( 'NONE', #10165, .T. ) ;
#9391 = VECTOR ( 'NONE', #5299, 39.37007874015748143 ) ;
#9392 = AXIS2_PLACEMENT_3D ( 'NONE', #28662, #4920, #9050 ) ;
#9393 = B_SPLINE_CURVE_WITH_KNOTS ( 'NONE', 3,
 ( #43633, #27890, #4404, #8021 ),
 .UNSPECIFIED., .F., .F.,
 ( 4, 4 ),
 ( 0.1211873102087489551, 0.1625992483279400380 ),
 .UNSPECIFIED. ) ;
#9394 = EDGE_LOOP ( 'NONE', ( #11823, #40480, #1, #26241 ) ) ;
#9395 = AXIS2_PLACEMENT_3D ( 'NONE', #36382, #17522, #36641 ) ;
#9396 = CARTESIAN_POINT ( 'NONE',  ( 1.365808055127285092, 0.01624875952099000959, 1.488494957536232510 ) ) ;
#9397 = CARTESIAN_POINT ( 'NONE',  ( 0.1968503937007869686, 3.267716535433071279, -2.086614173228339641 ) ) ;
#9398 = EDGE_LOOP ( 'NONE', ( #30659, #17226, #30583, #18401 ) ) ;
#9399 = PLANE ( 'NONE',  #48405 ) ;
#9400 = AXIS2_PLACEMENT_3D ( 'NONE', #41920, #45765, #45260 ) ;
#9401 = AXIS2_PLACEMENT_3D ( 'NONE', #10341, #50283, #37972 ) ;
#9402 = LINE ( 'NONE', #48598, #2068 ) ;
#9403 = LINE ( 'NONE', #21529, #2454 ) ;
#9404 = CARTESIAN_POINT ( 'NONE',  ( -0.8851347855165027090, 0.009234599073057599486, 1.577415923295598876 ) ) ;
#9405 = EDGE_CURVE ( 'NONE', #26688, #16323, #9415, .T. ) ;
#9406 = EDGE_CURVE ( 'NONE', #49431, #49218, #8644, .T. ) ;
#9407 = EDGE_CURVE ( 'NONE', #30647, #8095, #644, .T. ) ;
#9408 = DIRECTION ( 'NONE',  ( 1.734723475976806848E-16, -0.000000000000000000, 1.000000000000000000 ) ) ;
#9409 = VERTEX_POINT ( 'NONE', #4774 ) ;
#9410 = ORIENTED_EDGE ( 'NONE', *, *, #46387, .F. ) ;
#9411 = LINE ( 'NONE', #40907, #40540 ) ;
#9412 = VECTOR ( 'NONE', #44423, 39.37007874015748143 ) ;
#9413 = PLANE ( 'NONE',  #24647 ) ;
#9414 = ORIENTED_EDGE ( 'NONE', *, *, #39709, .F. ) ;
#9415 = LINE ( 'NONE', #40655, #50533 ) ;
#9416 = CARTESIAN_POINT ( 'NONE',  ( 2.083268748869757658, 3.267716535433071279, 0.5905511811023582691 ) ) ;
#9417 = DIRECTION ( 'NONE',  ( 1.734723475976806848E-16, -0.000000000000000000, 1.000000000000000000 ) ) ;
#9418 = CARTESIAN_POINT ( 'NONE',  ( 0.1968503937007873017, 0.000000000000000000, -1.259842519685035134 ) ) ;
#9419 = VERTEX_POINT ( 'NONE', #28000 ) ;
#9420 = ORIENTED_EDGE ( 'NONE', *, *, #23986, .F. ) ;
#9421 = DIRECTION ( 'NONE',  ( -0.000000000000000000, 1.000000000000000000, -0.000000000000000000 ) ) ;
#9422 = LINE ( 'NONE', #6813, #32401 ) ;
#9423 = LINE ( 'NONE', #17421, #9903 ) ;
#9424 = ORIENTED_EDGE ( 'NONE', *, *, #4878, .T. ) ;
#9425 = LINE ( 'NONE', #17174, #38081 ) ;
#9426 = FACE_BOUND ( 'NONE', #28835, .T. ) ;
#9427 = ORIENTED_EDGE ( 'NONE', *, *, #443, .F. ) ;
#9428 = DIRECTION ( 'NONE',  ( 0.000000000000000000, 0.000000000000000000, 1.000000000000000000 ) ) ;
#9429 = VERTEX_POINT ( 'NONE', #16396 ) ;
#9430 = ORIENTED_EDGE ( 'NONE', *, *, #25037, .T. ) ;
#9431 = ADVANCED_FACE ( 'NONE', ( #20521 ), #32927, .F. ) ;
#9432 = FACE_OUTER_BOUND ( 'NONE', #36316, .T. ) ;
#9433 = EDGE_CURVE ( 'NONE', #43799, #30581, #48089, .T. ) ;
#9434 = ORIENTED_EDGE ( 'NONE', *, *, #42071, .F. ) ;
#9435 = CARTESIAN_POINT ( 'NONE',  ( -1.363819533518803029, 3.346456692913386100, 0.7874015748031456541 ) ) ;
#9436 = EDGE_CURVE ( 'NONE', #8029, #5151, #8899, .T. ) ;
#9437 = LINE ( 'NONE', #19819, #21269 ) ;
#9438 = ORIENTED_EDGE ( 'NONE', *, *, #15241, .F. ) ;
#9439 = VECTOR ( 'NONE', #7594, 39.37007874015748143 ) ;
#9440 = ADVANCED_FACE ( 'NONE', ( #16655 ), #36530, .F. ) ;
#9441 = ADVANCED_FACE ( 'NONE', ( #1409 ), #1153, .F. ) ;
#9442 = VECTOR ( 'NONE', #49172, 39.37007874015748143 ) ;
#9443 = LINE ( 'NONE', #10203, #34354 ) ;
#9444 = DIRECTION ( 'NONE',  ( 0.000000000000000000, 0.000000000000000000, 1.000000000000000000 ) ) ;
#9445 = VECTOR ( 'NONE', #32464, 39.37007874015748143 ) ;
#9446 = VECTOR ( 'NONE', #10274, 39.37007874015748143 ) ;
#9447 = DIRECTION ( 'NONE',  ( 5.779879058772725700E-18, 1.000000000000000000, -1.286990067732317241E-16 ) ) ;
#9448 = CARTESIAN_POINT ( 'NONE',  ( -0.5455278134075214336, 3.267716535433071279, 0.3149606299212577287 ) ) ;
#9449 = CARTESIAN_POINT ( 'NONE',  ( -2.122900408447768505, 1.587732724264993900, -2.052396256617323278 ) ) ;
#9450 = AXIS2_PLACEMENT_3D ( 'NONE', #21907, #43212, #7861 ) ;
#9451 = EDGE_LOOP ( 'NONE', ( #42379, #21475, #14888, #33997 ) ) ;
#9452 = DIRECTION ( 'NONE',  ( -0.000000000000000000, 0.000000000000000000, 1.000000000000000000 ) ) ;
#9453 = LINE ( 'NONE', #32966, #16618 ) ;
#9454 = ORIENTED_EDGE ( 'NONE', *, *, #18983, .T. ) ;
#9455 = CARTESIAN_POINT ( 'NONE',  ( 2.136142994004097684, 1.647101463257393705, -1.351088264443995213 ) ) ;
#9456 = CARTESIAN_POINT ( 'NONE',  ( 0.000000000000000000, 3.346456692913386100, 0.000000000000000000 ) ) ;
#9457 = ORIENTED_EDGE ( 'NONE', *, *, #38300, .T. ) ;
#9458 = CARTESIAN_POINT ( 'NONE',  ( 0.000000000000000000, 3.267716535433071279, -1.141732283464563569 ) ) ;
#9459 = CARTESIAN_POINT ( 'NONE',  ( -2.182111253630085290, 3.346456692913386100, 0.6299212598425164567 ) ) ;
#9460 = DIRECTION ( 'NONE',  ( -3.469446951953613696E-16, 0.000000000000000000, -1.000000000000000000 ) ) ;
#9461 = ORIENTED_EDGE ( 'NONE', *, *, #46921, .T. ) ;
#9462 = FACE_OUTER_BOUND ( 'NONE', #40465, .T. ) ;
#9463 = ORIENTED_EDGE ( 'NONE', *, *, #5458, .T. ) ;
#9464 = FACE_BOUND ( 'NONE', #30535, .T. ) ;
#9465 = FACE_OUTER_BOUND ( 'NONE', #42317, .T. ) ;
#9466 = DIRECTION ( 'NONE',  ( -1.000000000000000000, 0.000000000000000000, -0.000000000000000000 ) ) ;
#9467 = DIRECTION ( 'NONE',  ( 1.000000000000000000, 0.000000000000000000, 2.775557561562891351E-16 ) ) ;
#9468 = EDGE_CURVE ( 'NONE', #42898, #10781, #12514, .T. ) ;
#9469 = EDGE_CURVE ( 'NONE', #39301, #44322, #44260, .T. ) ;
#9470 = ORIENTED_EDGE ( 'NONE', *, *, #49012, .F. ) ;
#9471 = VERTEX_POINT ( 'NONE', #17162 ) ;
#9472 = VECTOR ( 'NONE', #6967, 39.37007874015748143 ) ;
#9473 = EDGE_CURVE ( 'NONE', #11679, #18573, #44512, .T. ) ;
#9474 = DIRECTION ( 'NONE',  ( 0.000000000000000000, 0.000000000000000000, -1.000000000000000000 ) ) ;
#9475 = ORIENTED_EDGE ( 'NONE', *, *, #6459, .F. ) ;
#9476 = AXIS2_PLACEMENT_3D ( 'NONE', #1823, #6214, #10595 ) ;
#9477 = DIRECTION ( 'NONE',  ( -3.469446951953613696E-16, 0.000000000000000000, -1.000000000000000000 ) ) ;
#9478 = ORIENTED_EDGE ( 'NONE', *, *, #22072, .T. ) ;
#9479 = EDGE_CURVE ( 'NONE', #14608, #36153, #27205, .T. ) ;
#9480 = CIRCLE ( 'NONE', #46549, 2.443628662382284489 ) ;
#9481 = LINE ( 'NONE', #17478, #34719 ) ;
#9482 = VERTEX_POINT ( 'NONE', #47586 ) ;
#9483 = CARTESIAN_POINT ( 'NONE',  ( -1.195183497228115035E-16, 3.346456692913386100, -0.6299212598425177889 ) ) ;
#9484 = CARTESIAN_POINT ( 'NONE',  ( 0.5455278134075212115, 3.346456692913386100, -0.3149606299212593941 ) ) ;
#9485 = VECTOR ( 'NONE', #3806, 39.37007874015748143 ) ;
#9486 = EDGE_LOOP ( 'NONE', ( #26994, #31080, #26940, #50442 ) ) ;
#9487 = PLANE ( 'NONE',  #26525 ) ;
#9488 = VERTEX_POINT ( 'NONE', #12264 ) ;
#9489 = VERTEX_POINT ( 'NONE', #43739 ) ;
#9490 = ADVANCED_FACE ( 'NONE', ( #8390 ), #24137, .F. ) ;
#9491 = EDGE_CURVE ( 'NONE', #6407, #24742, #10430, .T. ) ;
#9492 = ORIENTED_EDGE ( 'NONE', *, *, #30003, .T. ) ;
#9493 = ORIENTED_EDGE ( 'NONE', *, *, #10354, .F. ) ;
#9494 = DIRECTION ( 'NONE',  ( -0.01601477604151182663, 0.9998717552508123996, -0.000000000000000000 ) ) ;
#9495 = ADVANCED_FACE ( 'NONE', ( #37299 ), #25664, .F. ) ;
#9496 = ORIENTED_EDGE ( 'NONE', *, *, #24447, .T. ) ;
#9497 = CARTESIAN_POINT ( 'NONE',  ( -2.867773316779185677, 1.674559808355669199, -0.7050287376752426560 ) ) ;
#9498 = ORIENTED_EDGE ( 'NONE', *, *, #40164, .T. ) ;
#9499 = CARTESIAN_POINT ( 'NONE',  ( -1.363819533518803473, 3.267716535433071279, 1.605145679676863057 ) ) ;
#9500 = CARTESIAN_POINT ( 'NONE',  ( 0.000000000000000000, 3.267716535433071279, -4.780733988912460139E-16 ) ) ;
#9501 = ORIENTED_EDGE ( 'NONE', *, *, #17975, .F. ) ;
#9502 = DIRECTION ( 'NONE',  ( 1.000000000000000000, -0.000000000000000000, 0.000000000000000000 ) ) ;
#9503 = LINE ( 'NONE', #21129, #42632 ) ;
#9504 = VECTOR ( 'NONE', #41327, 39.37007874015748143 ) ;
#9505 = ORIENTED_EDGE ( 'NONE', *, *, #33760, .F. ) ;
#9506 = CARTESIAN_POINT ( 'NONE',  ( -2.082617625631827174, 3.267716535433071279, 0.3149606299212578953 ) ) ;
#9507 = LINE ( 'NONE', #6140, #42337 ) ;
#9508 = AXIS2_PLACEMENT_3D ( 'NONE', #37996, #14749, #2618 ) ;
#9509 = CARTESIAN_POINT ( 'NONE',  ( 2.919426793319799707, 5.118110236220475784, 0.4451252810446826302 ) ) ;
#9510 = VECTOR ( 'NONE', #33102, 39.37007874015748143 ) ;
#9511 = LINE ( 'NONE', #25505, #42109 ) ;
#9512 = B_SPLINE_CURVE_WITH_KNOTS ( 'NONE', 3,
 ( #9753, #29628, #41497, #2518 ),
 .UNSPECIFIED., .F., .F.,
 ( 4, 4 ),
 ( 0.001413063469367606406, 0.003913248153456502960 ),
 .UNSPECIFIED. ) ;
#9513 = DIRECTION ( 'NONE',  ( -0.01601477604151182663, 0.9998717552508123996, -0.000000000000000000 ) ) ;
#9514 = EDGE_LOOP ( 'NONE', ( #38908, #29346, #28515, #19624 ) ) ;
#9515 = LINE ( 'NONE', #47234, #47616 ) ;
#9516 = CARTESIAN_POINT ( 'NONE',  ( -0.8182917201112819283, 3.346456692913386100, -0.03937007874015895081 ) ) ;
#9517 = VECTOR ( 'NONE', #4249, 39.37007874015748143 ) ;
#9518 = ORIENTED_EDGE ( 'NONE', *, *, #29852, .T. ) ;
#9519 = CARTESIAN_POINT ( 'NONE',  ( -2.308557526972532692, 5.905511811023623991, 1.841013194464760305 ) ) ;
#9520 = ORIENTED_EDGE ( 'NONE', *, *, #47845, .F. ) ;
#9521 = CARTESIAN_POINT ( 'NONE',  ( 0.4696143004045479352, 3.346456692913386100, -1.102362204724405714 ) ) ;
#9522 = CARTESIAN_POINT ( 'NONE',  ( -0.07591351300297359550, 3.267716535433071279, -2.047244094488181343 ) ) ;
#9523 = LINE ( 'NONE', #37410, #11367 ) ;
#9524 = FACE_OUTER_BOUND ( 'NONE', #8242, .T. ) ;
#9525 = DIRECTION ( 'NONE',  ( -0.000000000000000000, 1.000000000000000000, -0.000000000000000000 ) ) ;
#9526 = ORIENTED_EDGE ( 'NONE', *, *, #4411, .T. ) ;
#9527 = LINE ( 'NONE', #5397, #48005 ) ;
#9528 = EDGE_CURVE ( 'NONE', #26747, #19657, #29544, .T. ) ;
#9529 = FACE_BOUND ( 'NONE', #50221, .T. ) ;
#9530 = ADVANCED_FACE ( 'NONE', ( #21289 ), #1919, .F. ) ;
#9531 = ORIENTED_EDGE ( 'NONE', *, *, #7315, .T. ) ;
#9532 = CARTESIAN_POINT ( 'NONE',  ( 0.8182917201112819283, 3.346456692913386100, 0.7874015748031454320 ) ) ;
#9533 = ORIENTED_EDGE ( 'NONE', *, *, #19592, .F. ) ;
#9534 = EDGE_CURVE ( 'NONE', #47091, #33606, #6306, .T. ) ;
#9535 = DIRECTION ( 'NONE',  ( -3.469446951953613696E-16, 0.000000000000000000, -1.000000000000000000 ) ) ;
#9536 = PLANE ( 'NONE',  #20636 ) ;
#9537 = CARTESIAN_POINT ( 'NONE',  ( -1.439733046521776139, 3.346456692913386100, 0.3149606299212578953 ) ) ;
#9538 = EDGE_CURVE ( 'NONE', #17338, #27824, #29282, .T. ) ;
#9539 = DIRECTION ( 'NONE',  ( -0.000000000000000000, 1.000000000000000000, -0.000000000000000000 ) ) ;
#9540 = AXIS2_PLACEMENT_3D ( 'NONE', #36624, #25504, #36370 ) ;
#9541 = ORIENTED_EDGE ( 'NONE', *, *, #27302, .T. ) ;
#9542 = ORIENTED_EDGE ( 'NONE', *, *, #11293, .F. ) ;
#9543 = AXIS2_PLACEMENT_3D ( 'NONE', #22205, #6198, #49268 ) ;
#9544 = CARTESIAN_POINT ( 'NONE',  ( 0.5905511811023627100, 0.000000000000000000, 2.165354330708661568 ) ) ;
#9545 = DIRECTION ( 'NONE',  ( 1.734723475976806848E-16, -0.000000000000000000, 1.000000000000000000 ) ) ;
#9546 = FACE_BOUND ( 'NONE', #32531, .T. ) ;
#9547 = ORIENTED_EDGE ( 'NONE', *, *, #24686, .F. ) ;
#9548 = VECTOR ( 'NONE', #2741, 39.37007874015748143 ) ;
#9549 = FACE_OUTER_BOUND ( 'NONE', #30064, .T. ) ;
#9550 = EDGE_CURVE ( 'NONE', #21218, #42295, #6921, .T. ) ;
#9551 = DIRECTION ( 'NONE',  ( -1.000000000000000000, 0.000000000000000000, 1.734723475976806848E-16 ) ) ;
#9552 = CIRCLE ( 'NONE', #18616, 2.106299212598425008 ) ;
#9553 = B_SPLINE_CURVE_WITH_KNOTS ( 'NONE', 3,
 ( #47369, #15913, #4558, #20030 ),
 .UNSPECIFIED., .F., .F.,
 ( 4, 4 ),
 ( 0.001036764039224162678, 0.004836410851953563440 ),
 .UNSPECIFIED. ) ;
#9554 = ORIENTED_EDGE ( 'NONE', *, *, #41962, .F. ) ;
#9555 = CARTESIAN_POINT ( 'NONE',  ( -1.387661672111457412, 1.205361022782829114E-17, -1.663104731517942136 ) ) ;
#9556 = AXIS2_PLACEMENT_3D ( 'NONE', #49996, #41794, #42545 ) ;
#9557 = PLANE ( 'NONE',  #36940 ) ;
#9558 = EDGE_CURVE ( 'NONE', #13466, #24951, #30304, .T. ) ;
#9559 = ORIENTED_EDGE ( 'NONE', *, *, #42708, .T. ) ;
#9560 = ORIENTED_EDGE ( 'NONE', *, *, #1789, .F. ) ;
#9561 = ORIENTED_EDGE ( 'NONE', *, *, #4337, .F. ) ;
#9562 = LINE ( 'NONE', #13692, #2132 ) ;
#9563 = DIRECTION ( 'NONE',  ( 0.000000000000000000, 0.000000000000000000, -1.000000000000000000 ) ) ;
#9564 = DIRECTION ( 'NONE',  ( 0.000000000000000000, 1.000000000000000000, 0.000000000000000000 ) ) ;
#9565 = CARTESIAN_POINT ( 'NONE',  ( 0.000000000000000000, 3.267716535433071279, -0.1968503937007883287 ) ) ;
#9566 = VERTEX_POINT ( 'NONE', #9671 ) ;
#9567 = VERTEX_POINT ( 'NONE', #49119 ) ;
#9568 = CARTESIAN_POINT ( 'NONE',  ( 0.000000000000000000, 0.000000000000000000, 0.000000000000000000 ) ) ;
#9569 = FACE_OUTER_BOUND ( 'NONE', #26308, .T. ) ;
#9570 = ADVANCED_FACE ( 'NONE', ( #2433 ), #49869, .F. ) ;
#9571 = LINE ( 'NONE', #21700, #1246 ) ;
#9572 = CARTESIAN_POINT ( 'NONE',  ( 1.015142113812069091, 3.239993870794025010, -2.236998478663746237 ) ) ;
#9573 = CARTESIAN_POINT ( 'NONE',  ( 2.378961647330872342, 3.230577599468342775, 0.6299212598425161236 ) ) ;
#9574 = AXIS2_PLACEMENT_3D ( 'NONE', #550, #43133, #16297 ) ;
#9575 = PLANE ( 'NONE',  #29185 ) ;
#9576 = ORIENTED_EDGE ( 'NONE', *, *, #40523, .T. ) ;
#9577 = VECTOR ( 'NONE', #38033, 39.37007874015748143 ) ;
#9578 = CARTESIAN_POINT ( 'NONE',  ( -1.363819533518803251, 3.267716535433071279, 2.365849761790805487E-16 ) ) ;
#9579 = LINE ( 'NONE', #25322, #35148 ) ;
#9580 = VECTOR ( 'NONE', #45854, 39.37007874015748143 ) ;
#9581 = EDGE_LOOP ( 'NONE', ( #36830, #7291, #2971, #24938 ) ) ;
#9582 = ORIENTED_EDGE ( 'NONE', *, *, #43445, .F. ) ;
#9583 = LINE ( 'NONE', #13718, #33999 ) ;
#9584 = LINE ( 'NONE', #21975, #5594 ) ;
#9585 = AXIS2_PLACEMENT_3D ( 'NONE', #48045, #28451, #16859 ) ;
#9586 = VERTEX_POINT ( 'NONE', #26422 ) ;
#9587 = VECTOR ( 'NONE', #19238, 39.37007874015748143 ) ;
#9588 = EDGE_CURVE ( 'NONE', #25851, #3960, #14047, .T. ) ;
#9589 = ORIENTED_EDGE ( 'NONE', *, *, #36399, .F. ) ;
#9590 = CARTESIAN_POINT ( 'NONE',  ( 2.164658444855302122, 5.905511811023623991, -0.04795272066889885720 ) ) ;
#9591 = VERTEX_POINT ( 'NONE', #37809 ) ;
#9592 = EDGE_CURVE ( 'NONE', #42497, #15363, #29795, .T. ) ;
#9593 = CARTESIAN_POINT ( 'NONE',  ( -0.8182917201112814842, 0.000000000000000000, 0.4724409448818872592 ) ) ;
#9594 = PLANE ( 'NONE',  #34648 ) ;
#9595 = EDGE_CURVE ( 'NONE', #39853, #24587, #41416, .T. ) ;
#9596 = EDGE_CURVE ( 'NONE', #33624, #11338, #21801, .T. ) ;
#9597 = ORIENTED_EDGE ( 'NONE', *, *, #25347, .F. ) ;
#9598 = ORIENTED_EDGE ( 'NONE', *, *, #38493, .T. ) ;
#9599 = ORIENTED_EDGE ( 'NONE', *, *, #48812, .T. ) ;
#9600 = B_SPLINE_CURVE_WITH_KNOTS ( 'NONE', 3,
 ( #18303, #13928, #37429, #48989 ),
 .UNSPECIFIED., .F., .F.,
 ( 4, 4 ),
 ( 2.136435014586510233E-07, 0.002500479660419988558 ),
 .UNSPECIFIED. ) ;
#9601 = CARTESIAN_POINT ( 'NONE',  ( 0.9766252528120925591, 0.01428436922565947537, 1.730545172518233699 ) ) ;
#9602 = ORIENTED_EDGE ( 'NONE', *, *, #44732, .T. ) ;
#9603 = ORIENTED_EDGE ( 'NONE', *, *, #17639, .F. ) ;
#9604 = CARTESIAN_POINT ( 'NONE',  ( -0.2727639067037605503, 3.267716535433071279, 4.731699523581609741E-17 ) ) ;
#9605 = FACE_OUTER_BOUND ( 'NONE', #21955, .T. ) ;
#9606 = LINE ( 'NONE', #21478, #32754 ) ;
#9607 = B_SPLINE_CURVE_WITH_KNOTS ( 'NONE', 3,
 ( #2071, #2574, #14192, #5938 ),
 .UNSPECIFIED., .F., .F.,
 ( 4, 4 ),
 ( 0.1211775127643062444, 0.1625894504277921315 ),
 .UNSPECIFIED. ) ;
#9608 = ORIENTED_EDGE ( 'NONE', *, *, #28638, .F. ) ;
#9609 = CARTESIAN_POINT ( 'NONE',  ( -0.8004649005966125719, 0.000000000000000000, -1.548759025234861753 ) ) ;
#9610 = ADVANCED_FACE ( 'NONE', ( #2678 ), #49618, .F. ) ;
#9611 = LINE ( 'NONE', #1347, #46428 ) ;
#9612 = CARTESIAN_POINT ( 'NONE',  ( 1.723687301221656476, 1.205361022782829114E-17, -1.311649477509800876 ) ) ;
#9613 = VECTOR ( 'NONE', #49719, 39.37007874015748143 ) ;
#9614 = EDGE_LOOP ( 'NONE', ( #40749, #45921, #12646, #10329 ) ) ;
#9615 = CARTESIAN_POINT ( 'NONE',  ( -1.712496953225537411, 3.267716535433071279, 5.941417334598190051E-16 ) ) ;
#9616 = DIRECTION ( 'NONE',  ( -9.390536051998764103E-17, -1.000000000000000000, -6.822623802544789917E-17 ) ) ;
#9617 = VECTOR ( 'NONE', #42329, 39.37007874015748143 ) ;
#9618 = CIRCLE ( 'NONE', #24471, 2.165354330708661568 ) ;
#9619 = DIRECTION ( 'NONE',  ( -0.000000000000000000, 0.000000000000000000, 1.000000000000000000 ) ) ;
#9620 = EDGE_CURVE ( 'NONE', #12025, #44687, #1662, .T. ) ;
#9621 = ORIENTED_EDGE ( 'NONE', *, *, #41930, .F. ) ;
#9622 = EDGE_LOOP ( 'NONE', ( #20950, #19500, #50234, #3543 ) ) ;
#9623 = DIRECTION ( 'NONE',  ( 1.734723475976806848E-16, 0.000000000000000000, 1.000000000000000000 ) ) ;
#9624 = VECTOR ( 'NONE', #42189, 39.37007874015748143 ) ;
#9625 = ADVANCED_FACE ( 'NONE', ( #38062 ), #33176, .F. ) ;
#9626 = CARTESIAN_POINT ( 'NONE',  ( 1.693438507483599809, 1.640086946997390216, 1.863498184031233684 ) ) ;
#9627 = CARTESIAN_POINT ( 'NONE',  ( 2.651794250122221246E-16, 3.346456692913386100, 2.165354330708661568 ) ) ;
#9628 = ORIENTED_EDGE ( 'NONE', *, *, #19122, .T. ) ;
#9629 = ORIENTED_EDGE ( 'NONE', *, *, #46169, .F. ) ;
#9630 = VECTOR ( 'NONE', #35956, 39.37007874015748143 ) ;
#9631 = LINE ( 'NONE', #36237, #28362 ) ;
#9632 = ORIENTED_EDGE ( 'NONE', *, *, #29883, .T. ) ;
#9633 = CARTESIAN_POINT ( 'NONE',  ( -0.7145799201509080989, 6.692913385826772199, 2.044048657746648789 ) ) ;
#9634 = EDGE_CURVE ( 'NONE', #17559, #46164, #17659, .T. ) ;
#9635 = CARTESIAN_POINT ( 'NONE',  ( 0.2727639067037609943, 3.267716535433071279, 1.850393700787392293 ) ) ;
#9636 = CARTESIAN_POINT ( 'NONE',  ( -0.2727639067037607723, 0.000000000000000000, -1.732283464566922726 ) ) ;
#9637 = DIRECTION ( 'NONE',  ( -0.000000000000000000, 1.000000000000000000, -0.000000000000000000 ) ) ;
#9638 = LINE ( 'NONE', #9893, #44366 ) ;
#9639 = VERTEX_POINT ( 'NONE', #15611 ) ;
#9640 = CARTESIAN_POINT ( 'NONE',  ( -2.074656761898998170, 6.692913385826772199, -0.6223516566630905578 ) ) ;
#9641 = DIRECTION ( 'NONE',  ( -1.000000000000000000, -0.000000000000000000, -0.000000000000000000 ) ) ;
#9642 = EDGE_CURVE ( 'NONE', #10831, #5151, #47058, .T. ) ;
#9643 = CARTESIAN_POINT ( 'NONE',  ( 0.2810212965233879201, 1.723635030826397685, -2.939398504915932797 ) ) ;
#9644 = EDGE_CURVE ( 'NONE', #24556, #795, #24377, .T. ) ;
#9645 = ORIENTED_EDGE ( 'NONE', *, *, #6413, .T. ) ;
#9646 = PLANE ( 'NONE',  #41358 ) ;
#9647 = DIRECTION ( 'NONE',  ( 0.9909497617679331460, 0.000000000000000000, 0.1342332658176667026 ) ) ;
#9648 = DIRECTION ( 'NONE',  ( -0.6579387259397027066, 0.000000000000000000, -0.7530714660036196273 ) ) ;
#9649 = ORIENTED_EDGE ( 'NONE', *, *, #30566, .F. ) ;
#9650 = VECTOR ( 'NONE', #48900, 39.37007874015748143 ) ;
#9651 = CARTESIAN_POINT ( 'NONE',  ( 0.7376647802434432855, 1.010125197387645057, -2.487884157410633179 ) ) ;
#9652 = CARTESIAN_POINT ( 'NONE',  ( 1.951523201471517588, 0.05917688107560774985, -0.1369052102211298083 ) ) ;
#9653 = ORIENTED_EDGE ( 'NONE', *, *, #1373, .T. ) ;
#9654 = CARTESIAN_POINT ( 'NONE',  ( 1.363819533518804139, 3.346456692913386100, 1.605145679676863057 ) ) ;
#9655 = DIRECTION ( 'NONE',  ( -0.1785568947986370392, 0.000000000000000000, 0.9839295885986295565 ) ) ;
#9656 = ORIENTED_EDGE ( 'NONE', *, *, #38114, .F. ) ;
#9657 = DIRECTION ( 'NONE',  ( -1.000000000000000000, 0.000000000000000000, -0.000000000000000000 ) ) ;
#9658 = ADVANCED_FACE ( 'NONE', ( #11730 ), #881, .F. ) ;
#9659 = CARTESIAN_POINT ( 'NONE',  ( 2.182111253630085290, 3.346456692913386100, -1.161035397307311917E-15 ) ) ;
#9660 = PLANE ( 'NONE',  #51014 ) ;
#9661 = DIRECTION ( 'NONE',  ( -0.000000000000000000, 1.000000000000000000, -0.000000000000000000 ) ) ;
#9662 = VECTOR ( 'NONE', #26627, 39.37007874015748143 ) ;
#9663 = EDGE_CURVE ( 'NONE', #16084, #19545, #39105, .T. ) ;
#9664 = EDGE_CURVE ( 'NONE', #6110, #13500, #19727, .T. ) ;
#9665 = CARTESIAN_POINT ( 'NONE',  ( 0.7148041136150545816, 0.000000000000000000, -2.044646019095610168 ) ) ;
#9666 = VERTEX_POINT ( 'NONE', #35488 ) ;
#9667 = ORIENTED_EDGE ( 'NONE', *, *, #9550, .F. ) ;
#9668 = DIRECTION ( 'NONE',  ( 1.000000000000000000, -0.000000000000000000, 0.000000000000000000 ) ) ;
#9669 = CARTESIAN_POINT ( 'NONE',  ( 0.2727639067037609943, 0.000000000000000000, 1.220472440944875281 ) ) ;
#9670 = ORIENTED_EDGE ( 'NONE', *, *, #49110, .T. ) ;
#9671 = CARTESIAN_POINT ( 'NONE',  ( 0.7423782071083092626, 3.346456692913386100, 2.034117492951036166 ) ) ;
#9672 = DIRECTION ( 'NONE',  ( 0.000000000000000000, 0.000000000000000000, 1.000000000000000000 ) ) ;
#9673 = CARTESIAN_POINT ( 'NONE',  ( -0.5455278134075214336, 3.346456692913386100, -8.878505979408855953E-16 ) ) ;
#9674 = EDGE_LOOP ( 'NONE', ( #27930, #38105, #11908, #41490 ) ) ;
#9675 = ORIENTED_EDGE ( 'NONE', *, *, #29122, .T. ) ;
#9676 = CARTESIAN_POINT ( 'NONE',  ( -1.743145509346910149, 0.000000000000000000, -0.04249111949972883551 ) ) ;
#9677 = FACE_OUTER_BOUND ( 'NONE', #23019, .T. ) ;
#9678 = LINE ( 'NONE', #9934, #34626 ) ;
#9679 = VERTEX_POINT ( 'NONE', #43214 ) ;
#9680 = CARTESIAN_POINT ( 'NONE',  ( -2.139026224642868623, 1.640833132300933972, 0.3394128413014118606 ) ) ;
#9681 = FACE_BOUND ( 'NONE', #26677, .T. ) ;
#9682 = ORIENTED_EDGE ( 'NONE', *, *, #11264, .T. ) ;
#9683 = CARTESIAN_POINT ( 'NONE',  ( 0.000000000000000000, 3.267716535433071279, -0.9448818897637762948 ) ) ;
#9684 = VERTEX_POINT ( 'NONE', #36001 ) ;
#9685 = ORIENTED_EDGE ( 'NONE', *, *, #23762, .T. ) ;
#9686 = CARTESIAN_POINT ( 'NONE',  ( -1.263630850544466666, 0.000000000000000000, -1.276241334172347530 ) ) ;
#9687 = VECTOR ( 'NONE', #42923, 39.37007874015748143 ) ;
#9688 = VECTOR ( 'NONE', #4943, 39.37007874015748143 ) ;
#9690 = ORIENTED_EDGE ( 'NONE', *, *, #11607, .T. ) ;
#9689 = EDGE_CURVE ( 'NONE', #49800, #45211, #32134, .T. ) ;
#9691 = CARTESIAN_POINT ( 'NONE',  ( 2.106333035502527373, 3.267716535433071279, -0.006892066987323136953 ) ) ;
#9692 = UNCERTAINTY_MEASURE_WITH_UNIT (LENGTH_MEASURE( 1.000000000000000082E-05 ), #40606, 'distance_accuracy_value', 'NONE');
#9693 = DIRECTION ( 'NONE',  ( -0.4738686624730094055, 0.000000000000000000, 0.8805955318567321166 ) ) ;
#9694 = ORIENTED_EDGE ( 'NONE', *, *, #37789, .F. ) ;
#9695 = AXIS2_PLACEMENT_3D ( 'NONE', #12548, #8933, #1188 ) ;
#9696 = CARTESIAN_POINT ( 'NONE',  ( 1.363819533518803251, 3.267716535433071279, -2.365849761790805487E-16 ) ) ;
#9697 = CARTESIAN_POINT ( 'NONE',  ( -0.07591351300297359550, 0.000000000000000000, -2.047244094488181343 ) ) ;
#9698 = EDGE_CURVE ( 'NONE', #4856, #129, #43467, .T. ) ;
#9699 = FACE_OUTER_BOUND ( 'NONE', #30684, .T. ) ;
#9700 = EDGE_CURVE ( 'NONE', #5044, #22970, #5268, .T. ) ;
#9701 =( BOUNDED_CURVE ( )  B_SPLINE_CURVE ( 3, ( #22245, #33875, #26112, #34873 ),
 .UNSPECIFIED., .F., .F. ) 
 B_SPLINE_CURVE_WITH_KNOTS ( ( 4, 4 ),
 ( 2.506443096395472470, 2.557263767594603721 ),
 .UNSPECIFIED. ) 
 CURVE ( )  GEOMETRIC_REPRESENTATION_ITEM ( )  RATIONAL_B_SPLINE_CURVE ( ( 1.000000000000000000, 0.9997847831954709275, 0.9997847831954709275, 1.000000000000000000 ) ) 
 REPRESENTATION_ITEM ( '' )  );
#9702 = EDGE_CURVE ( 'NONE', #31964, #7588, #40112, .T. ) ;
#9703 = LINE ( 'NONE', #29577, #17355 ) ;
#9704 = LINE ( 'NONE', #49151, #36895 ) ;
#9705 = DIRECTION ( 'NONE',  ( -0.000000000000000000, 1.000000000000000000, -0.000000000000000000 ) ) ;
#9706 = VERTEX_POINT ( 'NONE', #47315 ) ;
#9707 = DIRECTION ( 'NONE',  ( -0.01601477604151182663, 0.9998717552508123996, -0.000000000000000000 ) ) ;
#9708 = VECTOR ( 'NONE', #44034, 39.37007874015748143 ) ;
#9709 = DIRECTION ( 'NONE',  ( -0.000000000000000000, 1.000000000000000000, -0.000000000000000000 ) ) ;
#9710 = ORIENTED_EDGE ( 'NONE', *, *, #10282, .F. ) ;
#9711 = LINE ( 'NONE', #25704, #18249 ) ;
#9712 = DIRECTION ( 'NONE',  ( -0.000000000000000000, 1.000000000000000000, -0.000000000000000000 ) ) ;
#9713 = EDGE_LOOP ( 'NONE', ( #42348, #47257, #47704, #23063 ) ) ;
#9714 = CARTESIAN_POINT ( 'NONE',  ( -1.636583440222563635, 0.000000000000000000, -4.780733988912460139E-16 ) ) ;
#9715 = ADVANCED_FACE ( 'NONE', ( #35236 ), #16118, .T. ) ;
#9717 = B_SPLINE_CURVE_WITH_KNOTS ( 'NONE', 3,
 ( #989, #12874, #24994, #20353 ),
 .UNSPECIFIED., .F., .F.,
 ( 4, 4 ),
 ( 0.1211873102087489551, 0.1625992483279400380 ),
 .UNSPECIFIED. ) ;
#9716 = CARTESIAN_POINT ( 'NONE',  ( -2.576863348864732117, 1.568913320674888201, 1.442554885838411849 ) ) ;
#9718 = PLANE ( 'NONE',  #7078 ) ;
#9719 = EDGE_LOOP ( 'NONE', ( #44400, #39810, #3637, #48353 ) ) ;
#9720 = CARTESIAN_POINT ( 'NONE',  ( 0.4696143004045484903, 3.346456692913386100, 1.732283464566921172 ) ) ;
#9721 = ORIENTED_EDGE ( 'NONE', *, *, #43640, .T. ) ;
#9722 = FACE_BOUND ( 'NONE', #7058, .T. ) ;
#9723 = CYLINDRICAL_SURFACE ( 'NONE', #34973, 2.165354330708661568 ) ;
#9724 = EDGE_CURVE ( 'NONE', #26498, #17294, #39556, .T. ) ;
#9725 = CARTESIAN_POINT ( 'NONE',  ( -0.5455278134075217666, 3.226699998040866824, -2.401574803149598036 ) ) ;
#9726 = PLANE ( 'NONE',  #50688 ) ;
#9727 = VECTOR ( 'NONE', #21400, 39.37007874015748143 ) ;
#9728 = EDGE_CURVE ( 'NONE', #37378, #681, #40127, .T. ) ;
#9729 = EDGE_CURVE ( 'NONE', #42663, #41559, #37111, .T. ) ;
#9730 = ORIENTED_EDGE ( 'NONE', *, *, #31062, .F. ) ;
#9731 = ORIENTED_EDGE ( 'NONE', *, *, #39061, .F. ) ;
#9732 = CARTESIAN_POINT ( 'NONE',  ( -1.088097428176262760, 1.690474079180120492, 1.917118167796188821 ) ) ;
#9733 = ADVANCED_FACE ( 'NONE', ( #4241 ), #20969, .T. ) ;
#9734 = VERTEX_POINT ( 'NONE', #20503 ) ;
#9735 = VECTOR ( 'NONE', #31002, 39.37007874015748143 ) ;
#9736 = LINE ( 'NONE', #5601, #12908 ) ;
#9737 = VERTEX_POINT ( 'NONE', #12497 ) ;
#9738 = DIRECTION ( 'NONE',  ( 0.000000000000000000, -1.000000000000000000, 0.000000000000000000 ) ) ;
#9739 = ORIENTED_EDGE ( 'NONE', *, *, #9144, .T. ) ;
#9740 = DIRECTION ( 'NONE',  ( 0.000000000000000000, 0.000000000000000000, -1.000000000000000000 ) ) ;
#9741 = VECTOR ( 'NONE', #28079, 39.37007874015748143 ) ;
#9742 = CARTESIAN_POINT ( 'NONE',  ( -1.481515513156636876, 0.000000000000000000, -0.9189724476880739568 ) ) ;
#9743 = ORIENTED_EDGE ( 'NONE', *, *, #37633, .F. ) ;
#9744 = DIRECTION ( 'NONE',  ( -0.6089060283534990514, 0.7932423643721808748, 0.000000000000000000 ) ) ;
#9745 = ORIENTED_EDGE ( 'NONE', *, *, #37514, .T. ) ;
#9746 = VERTEX_POINT ( 'NONE', #28493 ) ;
#9747 = VECTOR ( 'NONE', #11975, 39.37007874015748143 ) ;
#9748 = VERTEX_POINT ( 'NONE', #28235 ) ;
#9749 = ORIENTED_EDGE ( 'NONE', *, *, #8010, .T. ) ;
#9750 = CARTESIAN_POINT ( 'NONE',  ( -1.712496953225537188, 3.267716535433071279, 0.9055118110236167750 ) ) ;
#9751 = VERTEX_POINT ( 'NONE', #44242 ) ;
#9752 = CARTESIAN_POINT ( 'NONE',  ( 0.2727639067037608278, 3.267716535433071279, -4.731699523581614055E-17 ) ) ;
#9753 = CARTESIAN_POINT ( 'NONE',  ( 1.306991306359274629, 1.630410611703223545, -1.882644677548868550 ) ) ;
#9754 = EDGE_CURVE ( 'NONE', #47970, #3256, #8880, .T. ) ;
#9755 = AXIS2_PLACEMENT_3D ( 'NONE', #15437, #46388, #6677 ) ;
#9756 = DIRECTION ( 'NONE',  ( -1.000000000000000000, -0.000000000000000000, -0.000000000000000000 ) ) ;
#9757 = EDGE_LOOP ( 'NONE', ( #28431, #34052, #29580, #15465 ) ) ;
#9758 = EDGE_CURVE ( 'NONE', #26688, #18090, #45243, .T. ) ;
#9759 = CARTESIAN_POINT ( 'NONE',  ( -2.600183657057300035, 5.905511811023623991, 1.399218491554124144 ) ) ;
#9760 = DIRECTION ( 'NONE',  ( -1.000000000000000000, -0.000000000000000000, -0.000000000000000000 ) ) ;
#9761 = VERTEX_POINT ( 'NONE', #49097 ) ;
#9762 = CARTESIAN_POINT ( 'NONE',  ( 1.128560816269277955, 1.725977917706353670, 1.984842472008916170 ) ) ;
#9763 = DIRECTION ( 'NONE',  ( 0.000000000000000000, -1.000000000000000000, 0.000000000000000000 ) ) ;
#9764 = VECTOR ( 'NONE', #39962, 39.37007874015748143 ) ;
#9765 = CARTESIAN_POINT ( 'NONE',  ( 2.052631463899902364, 3.346456692913386100, 0.4724409448818868706 ) ) ;
#9766 = CARTESIAN_POINT ( 'NONE',  ( 1.838947341486932396, 0.05737377265108637575, 0.6492553997849701553 ) ) ;
#9767 = CIRCLE ( 'NONE', #50935, 2.246510896728926010 ) ;
#9768 = VECTOR ( 'NONE', #1587, 39.37007874015748143 ) ;
#9769 = LINE ( 'NONE', #10270, #50322 ) ;
#9770 = CARTESIAN_POINT ( 'NONE',  ( 0.000000000000000000, 0.07874015748031502893, 0.000000000000000000 ) ) ;
#9771 = ORIENTED_EDGE ( 'NONE', *, *, #21668, .T. ) ;
#9772 = CARTESIAN_POINT ( 'NONE',  ( -2.867773316779185677, 0.000000000000000000, -0.7050287376752425450 ) ) ;
#9773 = LINE ( 'NONE', #38166, #29221 ) ;
#9774 = VECTOR ( 'NONE', #8928, 39.37007874015748143 ) ;
#9775 = ORIENTED_EDGE ( 'NONE', *, *, #25050, .T. ) ;
#9776 = PLANE ( 'NONE',  #12723 ) ;
#9777 = EDGE_CURVE ( 'NONE', #22951, #42620, #29262, .T. ) ;
#9778 = VECTOR ( 'NONE', #26277, 39.37007874015748143 ) ;
#9779 = VERTEX_POINT ( 'NONE', #33667 ) ;
#9780 = CARTESIAN_POINT ( 'NONE',  ( -2.164823134740036181, 1.673228346456695492, 0.000000000000000000 ) ) ;
#9781 = CARTESIAN_POINT ( 'NONE',  ( 0.000000000000000000, 3.267716535433071279, 1.574803149606291974 ) ) ;
#9782 = DIRECTION ( 'NONE',  ( 1.000000000000000000, 0.000000000000000000, 0.000000000000000000 ) ) ;
#9783 = EDGE_CURVE ( 'NONE', #6941, #22597, #44396, .T. ) ;
#9784 = CARTESIAN_POINT ( 'NONE',  ( -1.909347346926324462, 3.346456692913386100, 0.7874015748031456541 ) ) ;
#9785 = CARTESIAN_POINT ( 'NONE',  ( 1.636583440222563635, 3.267716535433071279, -1.417869535855832419 ) ) ;
#9786 = ORIENTED_EDGE ( 'NONE', *, *, #3074, .T. ) ;
#9787 = EDGE_CURVE ( 'NONE', #37703, #15500, #6123, .T. ) ;
#9788 = DIRECTION ( 'NONE',  ( 0.000000000000000000, 0.000000000000000000, -1.000000000000000000 ) ) ;
#9789 = ORIENTED_EDGE ( 'NONE', *, *, #44271, .T. ) ;
#9790 = CARTESIAN_POINT ( 'NONE',  ( -2.576863348864732117, 1.580667355030889620, 1.442554885838411849 ) ) ;
#9791 = EDGE_CURVE ( 'NONE', #21262, #34643, #40636, .T. ) ;
#9792 = EDGE_LOOP ( 'NONE', ( #10253, #43810, #42418, #50671 ) ) ;
#9793 = LINE ( 'NONE', #28375, #8140 ) ;
#9794 = CARTESIAN_POINT ( 'NONE',  ( -1.556712866041156662, 1.548291375251236834, 2.509548638715847435 ) ) ;
#9795 = ORIENTED_EDGE ( 'NONE', *, *, #25084, .F. ) ;
#9796 = DIRECTION ( 'NONE',  ( 0.000000000000000000, 1.160734090543304660E-16, -1.000000000000000000 ) ) ;
#9797 = VECTOR ( 'NONE', #44509, 39.37007874015748143 ) ;
#9798 = DIRECTION ( 'NONE',  ( -0.08963930890344089242, -1.156025585781303350E-16, 0.9959742939952384022 ) ) ;
#9799 = DIRECTION ( 'NONE',  ( -3.469446951953613696E-16, 0.000000000000000000, -1.000000000000000000 ) ) ;
#9800 = ORIENTED_EDGE ( 'NONE', *, *, #43317, .T. ) ;
#9801 = EDGE_LOOP ( 'NONE', ( #35003, #3961, #35492, #34361, #9560 ) ) ;
#9802 = CARTESIAN_POINT ( 'NONE',  ( 1.025452293874513421, 0.5070346321433218950, 0.9794755770252094873 ) ) ;
#9803 = FACE_BOUND ( 'NONE', #5396, .T. ) ;
#9804 = VERTEX_POINT ( 'NONE', #41154 ) ;
#9805 = VECTOR ( 'NONE', #10116, 39.37007874015748143 ) ;
#9806 = CIRCLE ( 'NONE', #22988, 2.165354330708661568 ) ;
#9807 = LINE ( 'NONE', #48488, #7258 ) ;
#9808 = CARTESIAN_POINT ( 'NONE',  ( -2.592413363271652393, 1.568516221823312629, 1.413658116983555812 ) ) ;
#9809 = ORIENTED_EDGE ( 'NONE', *, *, #20404, .F. ) ;
#9810 = VERTEX_POINT ( 'NONE', #24636 ) ;
#9811 = AXIS2_PLACEMENT_3D ( 'NONE', #10645, #48883, #5566 ) ;
#9812 = PLANE ( 'NONE',  #1868 ) ;
#9813 = DIRECTION ( 'NONE',  ( -0.000000000000000000, 0.000000000000000000, 1.000000000000000000 ) ) ;
#9814 = EDGE_LOOP ( 'NONE', ( #8389, #27039, #10738, #6057 ) ) ;
#9815 = ORIENTED_EDGE ( 'NONE', *, *, #46915, .T. ) ;
#9816 = VECTOR ( 'NONE', #44490, 39.37007874015748143 ) ;
#9817 = ORIENTED_EDGE ( 'NONE', *, *, #46169, .T. ) ;
#9818 = CARTESIAN_POINT ( 'NONE',  ( -1.712496953225537633, 3.346456692913386100, -0.7874015748031470974 ) ) ;
#9819 = CARTESIAN_POINT ( 'NONE',  ( -2.182111253630085290, 3.346456692913386100, -6.146657985744592735E-16 ) ) ;
#9820 = DIRECTION ( 'NONE',  ( -3.986037398843765983E-20, -1.000000000000000000, -1.160734090543304660E-16 ) ) ;
#9821 = FACE_OUTER_BOUND ( 'NONE', #44459, .T. ) ;
#9822 = VERTEX_POINT ( 'NONE', #49355 ) ;
#9823 = VERTEX_POINT ( 'NONE', #17649 ) ;
#9824 = EDGE_CURVE ( 'NONE', #31188, #34410, #37537, .T. ) ;
#9825 = CARTESIAN_POINT ( 'NONE',  ( -1.166969139818015977, 3.346456692913386100, -1.732283464566922726 ) ) ;
#9826 = CARTESIAN_POINT ( 'NONE',  ( -2.182111253630085290, 3.346456692913386100, 0.4330708661417290162 ) ) ;
#9827 = ADVANCED_FACE ( 'NONE', ( #9390 ), #25142, .F. ) ;
#9828 = CARTESIAN_POINT ( 'NONE',  ( -0.07591351300297333182, 3.346456692913386100, -0.4724409448818883694 ) ) ;
#9829 = CARTESIAN_POINT ( 'NONE',  ( -1.091055626815042645, 0.000000000000000000, -1.889763779527552146 ) ) ;
#9830 = EDGE_CURVE ( 'NONE', #40779, #20338, #9906, .T. ) ;
#9831 = DIRECTION ( 'NONE',  ( 7.237058681235204266E-17, -1.000000000000000000, 9.074984547606538936E-17 ) ) ;
#9832 = PLANE ( 'NONE',  #25984 ) ;
#9833 = VECTOR ( 'NONE', #17348, 39.37007874015748143 ) ;
#9834 = CARTESIAN_POINT ( 'NONE',  ( -0.6214413264104945434, 0.000000000000000000, -1.732283464566922726 ) ) ;
#9835 = ORIENTED_EDGE ( 'NONE', *, *, #23285, .F. ) ;
#9836 = CARTESIAN_POINT ( 'NONE',  ( 1.091055626815042645, 0.000000000000000000, -8.878505979408855953E-16 ) ) ;
#9837 = CARTESIAN_POINT ( 'NONE',  ( 1.363819533518803251, 0.000000000000000000, -0.4724409448818889246 ) ) ;
#9838 = ORIENTED_EDGE ( 'NONE', *, *, #13783, .T. ) ;
#9839 = ORIENTED_EDGE ( 'NONE', *, *, #24793, .T. ) ;
#9841 = PLANE ( 'NONE',  #50432 ) ;
#9840 = VECTOR ( 'NONE', #342, 39.37007874015748143 ) ;
#9842 = CARTESIAN_POINT ( 'NONE',  ( 0.000000000000000000, 3.267716535433071279, 0.4724409448818871482 ) ) ;
#9843 = EDGE_CURVE ( 'NONE', #26214, #9586, #44494, .T. ) ;
#9844 = VERTEX_POINT ( 'NONE', #45494 ) ;
#9845 = CIRCLE ( 'NONE', #23025, 2.106299212598425008 ) ;
#9846 = ADVANCED_FACE ( 'NONE', ( #5259 ), #2156, .F. ) ;
#9847 = ORIENTED_EDGE ( 'NONE', *, *, #964, .T. ) ;
#9848 = DIRECTION ( 'NONE',  ( -1.000000000000000000, -0.000000000000000000, -0.000000000000000000 ) ) ;
#9849 = AXIS2_PLACEMENT_3D ( 'NONE', #50235, #4508, #31890 ) ;
#9850 = EDGE_LOOP ( 'NONE', ( #45217, #6436, #17883, #15294 ) ) ;
#9851 = LINE ( 'NONE', #9080, #37574 ) ;
#9852 = CARTESIAN_POINT ( 'NONE',  ( -0.2727639067037602727, 0.000000000000000000, 1.535433070866133898 ) ) ;
#9853 = ORIENTED_EDGE ( 'NONE', *, *, #34224, .T. ) ;
#9854 = ORIENTED_EDGE ( 'NONE', *, *, #40719, .T. ) ;
#9855 = DIRECTION ( 'NONE',  ( -1.000000000000000000, 0.000000000000000000, -0.000000000000000000 ) ) ;
#9856 = ORIENTED_EDGE ( 'NONE', *, *, #31750, .F. ) ;
#9857 = ORIENTED_EDGE ( 'NONE', *, *, #25337, .F. ) ;
#9858 = DIRECTION ( 'NONE',  ( -1.000000000000000000, 0.000000000000000000, 1.734723475976806848E-16 ) ) ;
#9859 = DIRECTION ( 'NONE',  ( -1.000000000000000000, 0.000000000000000000, 1.734723475976806848E-16 ) ) ;
#9860 = FACE_OUTER_BOUND ( 'NONE', #35124, .T. ) ;
#9861 = EDGE_CURVE ( 'NONE', #1626, #13831, #21520, .T. ) ;
#9862 = ORIENTED_EDGE ( 'NONE', *, *, #79, .F. ) ;
#9863 = DIRECTION ( 'NONE',  ( -3.469446951953613696E-16, 0.000000000000000000, -1.000000000000000000 ) ) ;
#9864 = DIRECTION ( 'NONE',  ( -1.000000000000000000, -0.000000000000000000, -0.000000000000000000 ) ) ;
#9865 = CONICAL_SURFACE ( 'NONE', #32992, 2.165354330708661568, 0.2617993877991570129 ) ;
#9866 = PLANE ( 'NONE',  #15462 ) ;
#9867 = VERTEX_POINT ( 'NONE', #1128 ) ;
#9868 = B_SPLINE_CURVE_WITH_KNOTS ( 'NONE', 3,
 ( #39641, #7891, #31388, #43239 ),
 .UNSPECIFIED., .F., .F.,
 ( 4, 4 ),
 ( 2.176057671437937673E-07, 0.01613016441388016517 ),
 .UNSPECIFIED. ) ;
#9869 = CARTESIAN_POINT ( 'NONE',  ( 0.4521076751547876138, 1.616718085813380945, 2.215705648545971407 ) ) ;
#9870 = DIRECTION ( 'NONE',  ( 1.734723475976806848E-16, -0.000000000000000000, 1.000000000000000000 ) ) ;
#9871 = CARTESIAN_POINT ( 'NONE',  ( 1.287906020515830141, 0.000000000000000000, -0.9448818897637765168 ) ) ;
#9872 = ORIENTED_EDGE ( 'NONE', *, *, #42440, .F. ) ;
#9873 = ORIENTED_EDGE ( 'NONE', *, *, #21265, .F. ) ;
#9874 =( CONVERSION_BASED_UNIT ( 'INCH', #14248 ) LENGTH_UNIT ( ) NAMED_UNIT ( #15895 ) );
#9875 = VECTOR ( 'NONE', #32299, 39.37007874015748143 ) ;
#9876 = LINE ( 'NONE', #43116, #34900 ) ;
#9877 = DIRECTION ( 'NONE',  ( -3.469446951953613696E-16, 0.000000000000000000, -1.000000000000000000 ) ) ;
#9878 = LINE ( 'NONE', #9627, #2395 ) ;
#9879 = EDGE_LOOP ( 'NONE', ( #36880, #5554, #18760, #38670 ) ) ;
#9880 = VERTEX_POINT ( 'NONE', #21015 ) ;
#9881 = EDGE_CURVE ( 'NONE', #50385, #41856, #46200, .T. ) ;
#9882 = CARTESIAN_POINT ( 'NONE',  ( 2.121469926805689354, 5.118110236220475784, -0.4337334748181388422 ) ) ;
#9883 = AXIS2_PLACEMENT_3D ( 'NONE', #36712, #9081, #13468 ) ;
#9884 = B_SPLINE_CURVE_WITH_KNOTS ( 'NONE', 3,
 ( #45580, #49189, #10244, #29616 ),
 .UNSPECIFIED., .F., .F.,
 ( 4, 4 ),
 ( 2.272220335726248535E-07, 0.01624913354395895668 ),
 .UNSPECIFIED. ) ;
#9885 = ORIENTED_EDGE ( 'NONE', *, *, #730, .F. ) ;
#9886 = DIRECTION ( 'NONE',  ( -0.01601477604151182663, 0.9998717552508123996, -0.000000000000000000 ) ) ;
#9887 = PLANE ( 'NONE',  #7795 ) ;
#9888 = ADVANCED_FACE ( 'NONE', ( #36767 ), #48130, .T. ) ;
#9889 = EDGE_CURVE ( 'NONE', #11672, #12924, #20349, .T. ) ;
#9890 = EDGE_CURVE ( 'NONE', #31232, #31458, #1642, .T. ) ;
#9891 = LINE ( 'NONE', #9119, #1959 ) ;
#9892 = CARTESIAN_POINT ( 'NONE',  ( 0.000000000000000000, 3.267716535433071279, -0.1574803149606301411 ) ) ;
#9893 = CARTESIAN_POINT ( 'NONE',  ( -1.712496953225537633, 3.346456692913386100, -0.4724409448818884805 ) ) ;
#9894 = ORIENTED_EDGE ( 'NONE', *, *, #26757, .T. ) ;
#9895 = LINE ( 'NONE', #5509, #11826 ) ;
#9896 = CARTESIAN_POINT ( 'NONE',  ( 0.002207914879453961535, -5.712274067634378313E-18, 0.04916304461325374242 ) ) ;
#9897 = DIRECTION ( 'NONE',  ( -3.469446951953613696E-16, 0.000000000000000000, -1.000000000000000000 ) ) ;
#9898 = ORIENTED_EDGE ( 'NONE', *, *, #3523, .T. ) ;
#9899 = DIRECTION ( 'NONE',  ( 1.000000000000000000, -0.000000000000000000, 0.000000000000000000 ) ) ;
#9900 = CARTESIAN_POINT ( 'NONE',  ( 1.748846139897575647, 1.475252794177884352, -2.379195924602942380 ) ) ;
#9901 = EDGE_CURVE ( 'NONE', #3787, #38012, #33158, .T. ) ;
#9902 = CARTESIAN_POINT ( 'NONE',  ( -1.636583440222564301, 3.346456692913386100, -1.141732283464563791 ) ) ;
#9903 = VECTOR ( 'NONE', #32680, 39.37007874015748143 ) ;
#9904 = EDGE_LOOP ( 'NONE', ( #42997, #45037, #37994, #22120 ) ) ;
#9905 = PLANE ( 'NONE',  #24213 ) ;
#9906 = LINE ( 'NONE', #1389, #12714 ) ;
#9907 = ADVANCED_FACE ( 'NONE', ( #10914 ), #6547, .F. ) ;
#9908 = ORIENTED_EDGE ( 'NONE', *, *, #49462, .T. ) ;
#9909 = CARTESIAN_POINT ( 'NONE',  ( 1.398572223930554026, 1.205361022782829114E-17, 1.525996566212370231 ) ) ;
#9910 = CARTESIAN_POINT ( 'NONE',  ( 0.000000000000000000, 3.267716535433071279, 1.417322834645662777 ) ) ;
#9911 = ORIENTED_EDGE ( 'NONE', *, *, #27262, .T. ) ;
#9912 = DIRECTION ( 'NONE',  ( -0.000000000000000000, 1.000000000000000000, -0.000000000000000000 ) ) ;
#9913 = VECTOR ( 'NONE', #41004, 39.37007874015748854 ) ;
#9914 = DIRECTION ( 'NONE',  ( 0.000000000000000000, 0.000000000000000000, -1.000000000000000000 ) ) ;
#9915 = DIRECTION ( 'NONE',  ( -0.000000000000000000, -1.000000000000000000, -0.000000000000000000 ) ) ;
#9916 = CARTESIAN_POINT ( 'NONE',  ( -1.171281348708517633, 1.623524940395525640, 1.864444939713191474 ) ) ;
#9917 = AXIS2_PLACEMENT_3D ( 'NONE', #32617, #28207, #48310 ) ;
#9918 = ADVANCED_FACE ( 'NONE', ( #7298 ), #46007, .F. ) ;
#9919 = CARTESIAN_POINT ( 'NONE',  ( -1.363819533518803473, 3.346456692913386100, 1.732283464566920950 ) ) ;
#9920 = VERTEX_POINT ( 'NONE', #46253 ) ;
#9921 = ORIENTED_EDGE ( 'NONE', *, *, #38311, .F. ) ;
#9922 = LINE ( 'NONE', #48605, #1803 ) ;
#9923 = CARTESIAN_POINT ( 'NONE',  ( 2.378961647330872786, 0.000000000000000000, 0.6299212598425161236 ) ) ;
#9924 = ORIENTED_EDGE ( 'NONE', *, *, #8744, .F. ) ;
#9925 = CARTESIAN_POINT ( 'NONE',  ( -1.166969139818015977, 3.346456692913386100, -1.102362204724405270 ) ) ;
#9926 = CARTESIAN_POINT ( 'NONE',  ( 1.287906020515830141, 3.346456692913386100, -0.8267716535433055070 ) ) ;
#9927 = VECTOR ( 'NONE', #15494, 39.37007874015748143 ) ;
#9928 = DIRECTION ( 'NONE',  ( -0.000000000000000000, 1.000000000000000000, -0.000000000000000000 ) ) ;
#9929 = EDGE_CURVE ( 'NONE', #12101, #20050, #4352, .T. ) ;
#9930 = ORIENTED_EDGE ( 'NONE', *, *, #7355, .F. ) ;
#9931 = VERTEX_POINT ( 'NONE', #2664 ) ;
#9932 = DIRECTION ( 'NONE',  ( 1.734723475976806848E-16, -0.000000000000000000, 1.000000000000000000 ) ) ;
#9933 = CARTESIAN_POINT ( 'NONE',  ( -1.091055626815042201, 3.267716535433071279, 0.6299212598425164567 ) ) ;
#9934 = CARTESIAN_POINT ( 'NONE',  ( -0.07591351300297333182, 3.346456692913386100, -1.732283464566922726 ) ) ;
#9935 = EDGE_LOOP ( 'NONE', ( #13690, #21229, #42137, #10843 ) ) ;
#9936 = CARTESIAN_POINT ( 'NONE',  ( 1.598711713508005117, 6.692913385826772199, -1.460438370699377764 ) ) ;
#9937 = CARTESIAN_POINT ( 'NONE',  ( 1.761123562704338452, 3.267716535433071279, 1.259842519685033135 ) ) ;
#9938 = ORIENTED_EDGE ( 'NONE', *, *, #12396, .F. ) ;
#9939 = ADVANCED_FACE ( 'NONE', ( #10669 ), #23039, .F. ) ;
#9940 = LINE ( 'NONE', #29809, #24922 ) ;
#9941 = ORIENTED_EDGE ( 'NONE', *, *, #30725, .T. ) ;
#9942 = ORIENTED_EDGE ( 'NONE', *, *, #50847, .F. ) ;
#9943 = PLANE ( 'NONE',  #32848 ) ;
#9944 = CARTESIAN_POINT ( 'NONE',  ( -1.636583440222563635, 3.267716535433071279, 0.4330708661417290162 ) ) ;
#9945 = ORIENTED_EDGE ( 'NONE', *, *, #29104, .F. ) ;
#9946 = PLANE ( 'NONE',  #49164 ) ;
#9947 = LINE ( 'NONE', #14584, #45263 ) ;
#9948 = VERTEX_POINT ( 'NONE', #232 ) ;
#9949 = PLANE ( 'NONE',  #6344 ) ;
#9950 = CARTESIAN_POINT ( 'NONE',  ( 0.5455278134075212115, 3.346456692913386100, -0.6299212598425181220 ) ) ;
#9951 = EDGE_CURVE ( 'NONE', #50754, #380, #27103, .T. ) ;
#9952 = VECTOR ( 'NONE', #7154, 39.37007874015748143 ) ;
#9953 = VECTOR ( 'NONE', #5390, 39.37007874015748143 ) ;
#9954 = PLANE ( 'NONE',  #19801 ) ;
#9955 = EDGE_CURVE ( 'NONE', #4281, #37443, #11170, .T. ) ;
#9956 = PLANE ( 'NONE',  #11305 ) ;
#9957 = PLANE ( 'NONE',  #10553 ) ;
#9958 = ORIENTED_EDGE ( 'NONE', *, *, #1312, .F. ) ;
#9959 = PLANE ( 'NONE',  #38206 ) ;
#9960 = CIRCLE ( 'NONE', #25649, 2.106299212598425008 ) ;
#9961 = CARTESIAN_POINT ( 'NONE',  ( 1.363819533518803251, 3.346456692913386100, 1.102362204724403938 ) ) ;
#9962 = ORIENTED_EDGE ( 'NONE', *, *, #31139, .T. ) ;
#9963 = CARTESIAN_POINT ( 'NONE',  ( 0.1968503937007873017, 3.346456692913386100, -0.6299212598425177889 ) ) ;
#9964 = DIRECTION ( 'NONE',  ( -0.000000000000000000, 1.000000000000000000, -0.000000000000000000 ) ) ;
#9965 = ORIENTED_EDGE ( 'NONE', *, *, #30428, .T. ) ;
#9966 = DIRECTION ( 'NONE',  ( 1.000000000000000000, 0.000000000000000000, 0.000000000000000000 ) ) ;
#9967 = CARTESIAN_POINT ( 'NONE',  ( 0.000000000000000000, 3.267716535433071279, -0.6692913385826758654 ) ) ;
#9968 = LINE ( 'NONE', #14095, #26842 ) ;
#9969 = ORIENTED_EDGE ( 'NONE', *, *, #14418, .F. ) ;
#9970 = DIRECTION ( 'NONE',  ( -0.000000000000000000, 0.000000000000000000, 1.000000000000000000 ) ) ;
#9971 = VERTEX_POINT ( 'NONE', #41652 ) ;
#9972 = FACE_BOUND ( 'NONE', #49839, .T. ) ;
#9973 = CARTESIAN_POINT ( 'NONE',  ( 0.07982360342473591996, 1.709180471932028711, 0.000000000000000000 ) ) ;
#9974 = FACE_OUTER_BOUND ( 'NONE', #23580, .T. ) ;
#9975 = DIRECTION ( 'NONE',  ( 1.734723475976806848E-16, 0.000000000000000000, 1.000000000000000000 ) ) ;
#9976 = EDGE_CURVE ( 'NONE', #16878, #16143, #38544, .T. ) ;
#9977 = ORIENTED_EDGE ( 'NONE', *, *, #521, .T. ) ;
#9978 = ORIENTED_EDGE ( 'NONE', *, *, #9138, .T. ) ;
#9979 = CARTESIAN_POINT ( 'NONE',  ( 1.636583440222563857, 3.346456692913386100, -0.1968503937007886062 ) ) ;
#9980 = ORIENTED_EDGE ( 'NONE', *, *, #5203, .T. ) ;
#9981 = CARTESIAN_POINT ( 'NONE',  ( 2.164658444855302122, 5.905511811023623991, -0.04795272066889885720 ) ) ;
#9982 = EDGE_LOOP ( 'NONE', ( #48726, #8217, #16459, #33175 ) ) ;
#9983 = ADVANCED_FACE ( 'NONE', ( #45747 ), #34166, .F. ) ;
#9984 = AXIS2_PLACEMENT_3D ( 'NONE', #49215, #25760, #29642 ) ;
#9985 = CARTESIAN_POINT ( 'NONE',  ( 0.4696143004045484903, 3.346456692913386100, 1.417322834645662777 ) ) ;
#9986 = CIRCLE ( 'NONE', #40499, 2.246510896728926010 ) ;
#9987 = ADVANCED_FACE ( 'NONE', ( #6790 ), #22535, .F. ) ;
#9988 = ORIENTED_EDGE ( 'NONE', *, *, #42428, .T. ) ;
#9989 = LINE ( 'NONE', #25735, #6818 ) ;
#9990 = ADVANCED_FACE ( 'NONE', ( #30789 ), #38297, .F. ) ;
#9991 = CARTESIAN_POINT ( 'NONE',  ( 0.000000000000000000, 3.267716535433071279, 0.000000000000000000 ) ) ;
#9992 = VERTEX_POINT ( 'NONE', #7045 ) ;
#9993 = EDGE_CURVE ( 'NONE', #4443, #26808, #22791, .T. ) ;
#9994 = PLANE ( 'NONE',  #20790 ) ;
#9995 = ORIENTED_EDGE ( 'NONE', *, *, #26322, .T. ) ;
#9996 = AXIS2_PLACEMENT_3D ( 'NONE', #23751, #43102, #7502 ) ;
#9997 = EDGE_LOOP ( 'NONE', ( #43906, #30824, #5090, #29205 ) ) ;
#9998 = EDGE_CURVE ( 'NONE', #23774, #34452, #34667, .T. ) ;
#9999 = VECTOR ( 'NONE', #11031, 39.37007874015748854 ) ;
#10000 =( BOUNDED_CURVE ( )  B_SPLINE_CURVE ( 3, ( #34778, #46617, #42259, #34281 ),
 .UNSPECIFIED., .F., .F. ) 
 B_SPLINE_CURVE_WITH_KNOTS ( ( 4, 4 ),
 ( 0.7124684239378302752, 0.7632890951369610821 ),
 .UNSPECIFIED. ) 
 CURVE ( )  GEOMETRIC_REPRESENTATION_ITEM ( )  RATIONAL_B_SPLINE_CURVE ( ( 1.000000000000000000, 0.9997847831954709275, 0.9997847831954709275, 1.000000000000000000 ) ) 
 REPRESENTATION_ITEM ( '' )  );
#10001 = VERTEX_POINT ( 'NONE', #15042 ) ;
#10002 = ORIENTED_EDGE ( 'NONE', *, *, #26537, .T. ) ;
#10003 = CARTESIAN_POINT ( 'NONE',  ( -0.2493563821447185302, 1.638291256590492129, -2.221569428308970195 ) ) ;
#10004 = ORIENTED_EDGE ( 'NONE', *, *, #11552, .F. ) ;
#10005 = FACE_OUTER_BOUND ( 'NONE', #45838, .T. ) ;
#10006 = DIRECTION ( 'NONE',  ( -0.9998717552508121775, -0.01601477604151182663, 0.000000000000000000 ) ) ;
#10007 = EDGE_CURVE ( 'NONE', #4959, #50129, #26901, .T. ) ;
#10008 = CARTESIAN_POINT ( 'NONE',  ( 2.277873973731426638, 1.463603380278871713, 1.879489153247667632 ) ) ;
#10009 = ADVANCED_FACE ( 'NONE', ( #3419 ), #27585, .T. ) ;
#10010 = ORIENTED_EDGE ( 'NONE', *, *, #37245, .F. ) ;
#10011 = FACE_OUTER_BOUND ( 'NONE', #19107, .T. ) ;
#10012 = LINE ( 'NONE', #2521, #49202 ) ;
#10013 = EDGE_CURVE ( 'NONE', #9169, #47474, #1523, .T. ) ;
#10014 = VERTEX_POINT ( 'NONE', #43595 ) ;
#10015 = DIRECTION ( 'NONE',  ( 1.734723475976806848E-16, 0.000000000000000000, 1.000000000000000000 ) ) ;
#10016 = LINE ( 'NONE', #25757, #8546 ) ;
#10017 = CARTESIAN_POINT ( 'NONE',  ( -0.3486774197067340486, 3.267716535433071279, -0.8267716535433049518 ) ) ;
#10018 = PLANE ( 'NONE',  #41313 ) ;
#10019 = AXIS2_PLACEMENT_3D ( 'NONE', #43524, #4049, #36056 ) ;
#10020 = CIRCLE ( 'NONE', #11661, 2.165354330708661568 ) ;
#10021 = LINE ( 'NONE', #18022, #47871 ) ;
#10022 = DIRECTION ( 'NONE',  ( 0.000000000000000000, 1.000000000000000000, 0.000000000000000000 ) ) ;
#10023 = ORIENTED_EDGE ( 'NONE', *, *, #14789, .T. ) ;
#10024 = LINE ( 'NONE', #22406, #30414 ) ;
#10025 = DIRECTION ( 'NONE',  ( 1.000000000000000000, 0.000000000000000000, 0.000000000000000000 ) ) ;
#10026 = AXIS2_PLACEMENT_3D ( 'NONE', #48978, #13659, #45125 ) ;
#10027 = ORIENTED_EDGE ( 'NONE', *, *, #37872, .F. ) ;
#10028 = DIRECTION ( 'NONE',  ( 1.000000000000000000, 0.000000000000000000, 0.000000000000000000 ) ) ;
#10029 = VECTOR ( 'NONE', #39756, 39.37007874015748143 ) ;
#10030 = VERTEX_POINT ( 'NONE', #43851 ) ;
#10031 = CARTESIAN_POINT ( 'NONE',  ( 0.2239970000120027616, 0.000000000000000000, -1.939803615689571048 ) ) ;
#10032 = DIRECTION ( 'NONE',  ( 5.782411586589357392E-17, -0.000000000000000000, 1.000000000000000000 ) ) ;
#10033 = VECTOR ( 'NONE', #42461, 39.37007874015748143 ) ;
#10034 = FACE_OUTER_BOUND ( 'NONE', #20653, .T. ) ;
#10035 = CARTESIAN_POINT ( 'NONE',  ( 0.4696143004045476577, 3.267716535433071279, -2.053280005709960054 ) ) ;
#10036 = DIRECTION ( 'NONE',  ( 1.734723475976806848E-16, -0.000000000000000000, 1.000000000000000000 ) ) ;
#10037 = EDGE_LOOP ( 'NONE', ( #33180, #26613, #39451, #7785 ) ) ;
#10038 = DIRECTION ( 'NONE',  ( 0.9998717552508121775, 0.01601477604151182663, 0.000000000000000000 ) ) ;
#10039 = ORIENTED_EDGE ( 'NONE', *, *, #16570, .T. ) ;
#10040 = EDGE_LOOP ( 'NONE', ( #22797, #44448, #23767, #31087 ) ) ;
#10041 = DIRECTION ( 'NONE',  ( -3.469446951953613696E-16, 0.000000000000000000, -1.000000000000000000 ) ) ;
#10042 = ORIENTED_EDGE ( 'NONE', *, *, #1789, .T. ) ;
#10043 = LINE ( 'NONE', #41793, #26271 ) ;
#10044 = CARTESIAN_POINT ( 'NONE',  ( -1.057143431661240696, 3.267716535433071279, 1.889763779527550147 ) ) ;
#10045 = ORIENTED_EDGE ( 'NONE', *, *, #11461, .T. ) ;
#10046 = DIRECTION ( 'NONE',  ( 1.734723475976806848E-16, -0.000000000000000000, 1.000000000000000000 ) ) ;
#10047 = EDGE_CURVE ( 'NONE', #16283, #19691, #47441, .T. ) ;
#10048 = LINE ( 'NONE', #45135, #26561 ) ;
#10049 = EDGE_CURVE ( 'NONE', #31344, #10330, #22632, .T. ) ;
#10050 = EDGE_CURVE ( 'NONE', #14916, #329, #4371, .T. ) ;
#10051 = CARTESIAN_POINT ( 'NONE',  ( -1.743516651958532115, 0.0004834999639498255872, 0.04168935124556687882 ) ) ;
#10052 = ORIENTED_EDGE ( 'NONE', *, *, #38861, .T. ) ;
#10053 = VERTEX_POINT ( 'NONE', #16510 ) ;
#10054 = CARTESIAN_POINT ( 'NONE',  ( 1.636583440222563857, 3.346456692913386100, 0.6299212598425164567 ) ) ;
#10055 = FACE_BOUND ( 'NONE', #11787, .T. ) ;
#10056 = ORIENTED_EDGE ( 'NONE', *, *, #7393, .F. ) ;
#10057 = AXIS2_PLACEMENT_3D ( 'NONE', #618, #20493, #47304 ) ;
#10058 = VECTOR ( 'NONE', #17109, 39.37007874015748143 ) ;
#10059 = CARTESIAN_POINT ( 'NONE',  ( -2.437180031585919782, 1.566133505135788750, -1.667735833703134274 ) ) ;
#10060 = LINE ( 'NONE', #28647, #15941 ) ;
#10061 = ORIENTED_EDGE ( 'NONE', *, *, #3521, .F. ) ;
#10062 = ORIENTED_EDGE ( 'NONE', *, *, #25973, .T. ) ;
#10063 = LINE ( 'NONE', #33316, #16693 ) ;
#10064 = AXIS2_PLACEMENT_3D ( 'NONE', #34809, #50742, #11064 ) ;
#10065 = CARTESIAN_POINT ( 'NONE',  ( -1.195183497228115035E-16, 0.000000000000000000, -0.6299212598425177889 ) ) ;
#10066 = VERTEX_POINT ( 'NONE', #20371 ) ;
#10067 = ORIENTED_EDGE ( 'NONE', *, *, #5639, .T. ) ;
#10068 = VECTOR ( 'NONE', #18567, 39.37007874015748143 ) ;
#10069 = EDGE_CURVE ( 'NONE', #24123, #50554, #28626, .T. ) ;
#10070 = ORIENTED_EDGE ( 'NONE', *, *, #9596, .T. ) ;
#10071 = LINE ( 'NONE', #37704, #2948 ) ;
#10072 = AXIS2_PLACEMENT_3D ( 'NONE', #28049, #39421, #32721 ) ;
#10073 = LINE ( 'NONE', #41314, #36533 ) ;
#10074 = EDGE_CURVE ( 'NONE', #4308, #27306, #16248, .T. ) ;
#10075 = DIRECTION ( 'NONE',  ( -0.000000000000000000, 1.000000000000000000, -0.000000000000000000 ) ) ;
#10076 = FACE_OUTER_BOUND ( 'NONE', #43788, .T. ) ;
#10077 = EDGE_CURVE ( 'NONE', #7418, #10769, #1266, .T. ) ;
#10078 = ORIENTED_EDGE ( 'NONE', *, *, #3910, .T. ) ;
#10079 = ORIENTED_EDGE ( 'NONE', *, *, #36924, .F. ) ;
#10080 = DIRECTION ( 'NONE',  ( -0.000000000000000000, 0.000000000000000000, 1.000000000000000000 ) ) ;
#10081 = LINE ( 'NONE', #45924, #17222 ) ;
#10082 = ADVANCED_FACE ( 'NONE', ( #28368 ), #32782, .F. ) ;
#10083 = LINE ( 'NONE', #34344, #41499 ) ;
#10084 = DIRECTION ( 'NONE',  ( 0.000000000000000000, -1.000000000000000000, 0.000000000000000000 ) ) ;
#10085 = LINE ( 'NONE', #18086, #2575 ) ;
#10086 = DIRECTION ( 'NONE',  ( -3.986037398843765983E-20, -1.000000000000000000, -1.160734090543304660E-16 ) ) ;
#10087 = LINE ( 'NONE', #33597, #31661 ) ;
#10088 = EDGE_LOOP ( 'NONE', ( #32910, #45559, #37090, #6569 ) ) ;
#10089 = CARTESIAN_POINT ( 'NONE',  ( 0.002207914879453961969, 6.692913385826772199, 0.04916304461325451958 ) ) ;
#10090 = DIRECTION ( 'NONE',  ( -0.000000000000000000, 0.000000000000000000, 1.000000000000000000 ) ) ;
#10091 = ORIENTED_EDGE ( 'NONE', *, *, #14181, .F. ) ;
#10092 = ORIENTED_EDGE ( 'NONE', *, *, #6185, .T. ) ;
#10093 = CONICAL_SURFACE ( 'NONE', #34815, 2.165354330708661568, 0.2617993877991570129 ) ;
#10094 = CARTESIAN_POINT ( 'NONE',  ( -0.5455278134075214336, 3.346456692913386100, -0.5118110236220467790 ) ) ;
#10095 = ORIENTED_EDGE ( 'NONE', *, *, #42637, .T. ) ;
#10096 = VECTOR ( 'NONE', #40723, 39.37007874015748143 ) ;
#10097 = ORIENTED_EDGE ( 'NONE', *, *, #30886, .F. ) ;
#10098 = CARTESIAN_POINT ( 'NONE',  ( 1.669153017917641924, 1.205361022782829114E-17, 1.268159837793114031 ) ) ;
#10099 = VECTOR ( 'NONE', #42240, 39.37007874015748143 ) ;
#10100 = ORIENTED_EDGE ( 'NONE', *, *, #8314, .F. ) ;
#10101 = AXIS2_PLACEMENT_3D ( 'NONE', #27987, #23867, #39617 ) ;
#10102 = CARTESIAN_POINT ( 'NONE',  ( 0.6363476328836782381, 3.267716535433071279, 2.007874015748021268 ) ) ;
#10103 = LINE ( 'NONE', #47452, #33852 ) ;
#10104 = ORIENTED_EDGE ( 'NONE', *, *, #11801, .F. ) ;
#10105 = EDGE_CURVE ( 'NONE', #13306, #39823, #12628, .T. ) ;
#10106 = ORIENTED_EDGE ( 'NONE', *, *, #40205, .F. ) ;
#10107 = CARTESIAN_POINT ( 'NONE',  ( 1.909347346926324462, 0.000000000000000000, -1.299212598425194320 ) ) ;
#10108 = ADVANCED_FACE ( 'NONE', ( #27854 ), #24254, .F. ) ;
#10109 = ORIENTED_EDGE ( 'NONE', *, *, #11920, .T. ) ;
#10110 = VERTEX_POINT ( 'NONE', #8248 ) ;
#10111 = CARTESIAN_POINT ( 'NONE',  ( 0.000000000000000000, 3.267716535433071279, 1.417322834645662777 ) ) ;
#10112 = CARTESIAN_POINT ( 'NONE',  ( 2.100403847690402337, 3.346456692913386100, -0.1574803149606304187 ) ) ;
#10113 = LINE ( 'NONE', #17604, #1289 ) ;
#10114 = ADVANCED_FACE ( 'NONE', ( #9268 ), #39997, .F. ) ;
#10115 = ORIENTED_EDGE ( 'NONE', *, *, #34026, .T. ) ;
#10116 = DIRECTION ( 'NONE',  ( -3.469446951953613696E-16, 0.000000000000000000, -1.000000000000000000 ) ) ;
#10117 = FACE_OUTER_BOUND ( 'NONE', #34341, .T. ) ;
#10118 = CARTESIAN_POINT ( 'NONE',  ( 0.7423782071083087075, 0.000000000000000000, -1.259842519685035134 ) ) ;
#10119 = ORIENTED_EDGE ( 'NONE', *, *, #23423, .T. ) ;
#10120 = CARTESIAN_POINT ( 'NONE',  ( 0.000000000000000000, 3.267716535433071279, 0.7874015748031456541 ) ) ;
#10121 = LINE ( 'NONE', #21745, #44174 ) ;
#10122 = PLANE ( 'NONE',  #41465 ) ;
#10123 = ORIENTED_EDGE ( 'NONE', *, *, #51035, .F. ) ;
#10124 = ORIENTED_EDGE ( 'NONE', *, *, #19843, .T. ) ;
#10125 = LINE ( 'NONE', #26377, #39020 ) ;
#10126 = EDGE_CURVE ( 'NONE', #38943, #49919, #25013, .T. ) ;
#10127 = DIRECTION ( 'NONE',  ( 0.000000000000000000, 0.000000000000000000, -1.000000000000000000 ) ) ;
#10128 = DIRECTION ( 'NONE',  ( -0.000000000000000000, 1.000000000000000000, -0.000000000000000000 ) ) ;
#10129 = ORIENTED_EDGE ( 'NONE', *, *, #47918, .F. ) ;
#10130 = ORIENTED_EDGE ( 'NONE', *, *, #32925, .T. ) ;
#10131 = AXIS2_PLACEMENT_3D ( 'NONE', #34943, #30816, #7326 ) ;
#10132 = ADVANCED_FACE ( 'NONE', ( #20105 ), #5137, .T. ) ;
#10133 = CARTESIAN_POINT ( 'NONE',  ( 1.636583440222563635, 3.346456692913386100, -1.456692913385823296 ) ) ;
#10134 = AXIS2_PLACEMENT_3D ( 'NONE', #47792, #21236, #48558 ) ;
#10135 = ORIENTED_EDGE ( 'NONE', *, *, #35992, .T. ) ;
#10136 = DIRECTION ( 'NONE',  ( 9.769962616701375978E-15, 0.000000000000000000, 1.000000000000000000 ) ) ;
#10137 = CARTESIAN_POINT ( 'NONE',  ( -0.2727639067037608278, 0.000000000000000000, 0.2755905511810995412 ) ) ;
#10138 = AXIS2_PLACEMENT_3D ( 'NONE', #32242, #42880, #24997 ) ;
#10139 = AXIS2_PLACEMENT_3D ( 'NONE', #16551, #10834, #26331 ) ;
#10140 = CYLINDRICAL_SURFACE ( 'NONE', #10177, 2.164630168518208109 ) ;
#10141 = DIRECTION ( 'NONE',  ( 1.000000000000000000, 0.000000000000000000, 0.000000000000000000 ) ) ;
#10142 = LINE ( 'NONE', #44983, #25396 ) ;
#10143 = AXIS2_PLACEMENT_3D ( 'NONE', #9192, #19774, #35794 ) ;
#10144 = ORIENTED_EDGE ( 'NONE', *, *, #41203, .T. ) ;
#10145 = CARTESIAN_POINT ( 'NONE',  ( 0.5455278134075212115, 3.346456692913386100, -0.3149606299212593941 ) ) ;
#10146 = CARTESIAN_POINT ( 'NONE',  ( 4.268512490100411402E-16, 0.000000000000000000, 2.204724409448808764 ) ) ;
#10147 = CARTESIAN_POINT ( 'NONE',  ( -0.5455278134075216556, 3.346456692913386100, -2.401574803149598036 ) ) ;
#10148 = ORIENTED_EDGE ( 'NONE', *, *, #5198, .T. ) ;
#10149 = FACE_OUTER_BOUND ( 'NONE', #28883, .T. ) ;
#10150 = PLANE ( 'NONE',  #12110 ) ;
#10151 = PLANE ( 'NONE',  #19707 ) ;
#10152 = ORIENTED_EDGE ( 'NONE', *, *, #46168, .T. ) ;
#10153 = CARTESIAN_POINT ( 'NONE',  ( 1.636583440222563635, 0.000000000000000000, -1.259842519685035800 ) ) ;
#10154 = ORIENTED_EDGE ( 'NONE', *, *, #25636, .F. ) ;
#10155 = CARTESIAN_POINT ( 'NONE',  ( -2.182111253630085290, 0.000000000000000000, -0.3149606299212589500 ) ) ;
#10156 = CARTESIAN_POINT ( 'NONE',  ( 4.268512490100411402E-16, 0.000000000000000000, 2.204724409448808764 ) ) ;
#10157 = ORIENTED_EDGE ( 'NONE', *, *, #34871, .T. ) ;
#10158 = CARTESIAN_POINT ( 'NONE',  ( -0.8182917201112819283, 3.346456692913386100, 1.850393700787391849 ) ) ;
#10159 = DIRECTION ( 'NONE',  ( -0.000000000000000000, 1.000000000000000000, -0.000000000000000000 ) ) ;
#10160 = CARTESIAN_POINT ( 'NONE',  ( 0.8182917201112819283, 0.000000000000000000, -0.4724409448818889246 ) ) ;
#10161 = CARTESIAN_POINT ( 'NONE',  ( -1.636583440222564301, 0.000000000000000000, -0.8267716535433052849 ) ) ;
#10162 = CARTESIAN_POINT ( 'NONE',  ( 1.294674717756378213, 1.049866565877817681, 1.556672598441452227 ) ) ;
#10163 = CONICAL_SURFACE ( 'NONE', #41493, 3.483074324928249421, 1.244861948955335196 ) ;
#10164 = ADVANCED_FACE ( 'NONE', ( #4885 ), #28881, .F. ) ;
#10165 = EDGE_LOOP ( 'NONE', ( #49448, #22974, #36214, #49549 ) ) ;
#10166 = ORIENTED_EDGE ( 'NONE', *, *, #38524, .F. ) ;
#10167 = DIRECTION ( 'NONE',  ( -0.8345732537213079727, 0.000000000000000000, 0.5508969814520945363 ) ) ;
#10168 = DIRECTION ( 'NONE',  ( -0.01601477604151182663, 0.9998717552508123996, -0.000000000000000000 ) ) ;
#10169 = EDGE_CURVE ( 'NONE', #34201, #41731, #5394, .T. ) ;
#10170 = VERTEX_POINT ( 'NONE', #497 ) ;
#10171 = VECTOR ( 'NONE', #41716, 39.37007874015748143 ) ;
#10172 = CARTESIAN_POINT ( 'NONE',  ( 0.8182917201112819283, 0.000000000000000000, -0.1574803149606301411 ) ) ;
#10173 = CARTESIAN_POINT ( 'NONE',  ( -1.557927422371237158, 0.000000000000000000, 0.7824709080581183640 ) ) ;
#10174 = FACE_OUTER_BOUND ( 'NONE', #8613, .T. ) ;
#10175 = EDGE_CURVE ( 'NONE', #10682, #20840, #32005, .T. ) ;
#10176 = AXIS2_PLACEMENT_3D ( 'NONE', #30258, #10639, #10384 ) ;
#10177 = AXIS2_PLACEMENT_3D ( 'NONE', #2646, #7284, #42134 ) ;
#10178 = VERTEX_POINT ( 'NONE', #37157 ) ;
#10179 = VERTEX_POINT ( 'NONE', #29395 ) ;
#10180 = DIRECTION ( 'NONE',  ( -1.000000000000000000, 0.000000000000000000, 0.000000000000000000 ) ) ;
#10181 = CARTESIAN_POINT ( 'NONE',  ( 0.000000000000000000, 3.267716535433071279, -1.614173228346451605 ) ) ;
#10182 = DIRECTION ( 'NONE',  ( -1.000000000000000000, 0.000000000000000000, 0.000000000000000000 ) ) ;
#10183 = EDGE_CURVE ( 'NONE', #29009, #37485, #37919, .T. ) ;
#10184 = EDGE_LOOP ( 'NONE', ( #48542, #42289, #17095, #31179 ) ) ;
#10185 = LINE ( 'NONE', #17680, #48739 ) ;
#10186 = DIRECTION ( 'NONE',  ( 1.000000000000000000, 0.000000000000000000, 0.000000000000000000 ) ) ;
#10187 = VECTOR ( 'NONE', #5248, 39.37007874015748143 ) ;
#10188 = EDGE_LOOP ( 'NONE', ( #5015, #4255, #4809, #22685 ) ) ;
#10189 = CARTESIAN_POINT ( 'NONE',  ( 0.000000000000000000, 3.267716535433071279, -1.732283464566923614 ) ) ;
#10190 = ORIENTED_EDGE ( 'NONE', *, *, #23870, .T. ) ;
#10191 = EDGE_LOOP ( 'NONE', ( #9143, #30870, #26928, #16374, #39999, #14481, #27489, #29481, #44114, #33503, #94, #28203, #24306 ) ) ;
#10192 = FACE_OUTER_BOUND ( 'NONE', #6192, .T. ) ;
#10193 = DIRECTION ( 'NONE',  ( 1.734723475976806848E-16, -0.000000000000000000, 1.000000000000000000 ) ) ;
#10194 = DIRECTION ( 'NONE',  ( 0.8345732537212999791, 0.000000000000000000, 0.5508969814521065267 ) ) ;
#10195 = ADVANCED_FACE ( 'NONE', ( #48974 ), #5655, .F. ) ;
#10196 = ORIENTED_EDGE ( 'NONE', *, *, #20916, .F. ) ;
#10197 = CARTESIAN_POINT ( 'NONE',  ( 0.8182917201112819283, 0.000000000000000000, 0.4724409448818868706 ) ) ;
#10198 = UNCERTAINTY_MEASURE_WITH_UNIT (LENGTH_MEASURE( 1.000000000000000082E-05 ), #43383, 'distance_accuracy_value', 'NONE');
#10199 = CARTESIAN_POINT ( 'NONE',  ( -0.3486774197067336045, 3.267716535433071279, 1.209717811016577845E-16 ) ) ;
#10200 = ORIENTED_EDGE ( 'NONE', *, *, #29464, .F. ) ;
#10201 = EDGE_CURVE ( 'NONE', #47505, #2009, #9296, .T. ) ;
#10202 = ORIENTED_EDGE ( 'NONE', *, *, #30384, .F. ) ;
#10203 = CARTESIAN_POINT ( 'NONE',  ( 0.4696143004045484903, 3.346456692913386100, 2.362204724409437961 ) ) ;
#10204 = CARTESIAN_POINT ( 'NONE',  ( -0.3486774197067339376, 0.000000000000000000, -0.9448818897637762948 ) ) ;
#10205 = CARTESIAN_POINT ( 'NONE',  ( 0.000000000000000000, 0.07874015748031495954, 0.000000000000000000 ) ) ;
#10206 = AXIS2_PLACEMENT_3D ( 'NONE', #30447, #29933, #26056 ) ;
#10207 = DIRECTION ( 'NONE',  ( -0.000000000000000000, 1.000000000000000000, -0.000000000000000000 ) ) ;
#10208 = DIRECTION ( 'NONE',  ( -0.000000000000000000, 1.000000000000000000, -0.000000000000000000 ) ) ;
#10209 = EDGE_LOOP ( 'NONE', ( #23126, #30022, #42685 ) ) ;
#10210 = DIRECTION ( 'NONE',  ( 0.000000000000000000, -0.000000000000000000, 1.000000000000000000 ) ) ;
#10211 = AXIS2_PLACEMENT_3D ( 'NONE', #27027, #19282, #23932 ) ;
#10212 = EDGE_CURVE ( 'NONE', #13102, #19845, #21912, .T. ) ;
#10213 = CARTESIAN_POINT ( 'NONE',  ( 1.015142113812069313, 3.346456692913386100, 1.102362204724403938 ) ) ;
#10214 = AXIS2_PLACEMENT_3D ( 'NONE', #20605, #19824, #35591 ) ;
#10215 = VECTOR ( 'NONE', #19018, 39.37007874015748143 ) ;
#10216 = EDGE_LOOP ( 'NONE', ( #3297, #19434, #5687, #14168, #15419, #14399, #6493, #19048, #13097, #30800, #36500 ) ) ;
#10217 = CARTESIAN_POINT ( 'NONE',  ( 0.000000000000000000, 3.346456692913386100, 0.000000000000000000 ) ) ;
#10218 = CARTESIAN_POINT ( 'NONE',  ( 1.091055626815042645, 3.267716535433071279, -0.9448818897637765168 ) ) ;
#10219 = EDGE_LOOP ( 'NONE', ( #43289, #48736, #18251, #23921 ) ) ;
#10220 = CARTESIAN_POINT ( 'NONE',  ( 1.833433833923351353, 0.000000000000000000, -0.6299212598425181220 ) ) ;
#10221 = DIRECTION ( 'NONE',  ( -3.469446951953613696E-16, 0.000000000000000000, -1.000000000000000000 ) ) ;
#10222 = CARTESIAN_POINT ( 'NONE',  ( -0.06966273521059174190, 0.000000000000000000, 0.3674709282358790130 ) ) ;
#10223 = VECTOR ( 'NONE', #23984, 39.37007874015748143 ) ;
#10224 = VERTEX_POINT ( 'NONE', #37668 ) ;
#10225 = CARTESIAN_POINT ( 'NONE',  ( 1.091055626815043311, 0.000000000000000000, 1.692913385826762873 ) ) ;
#10226 = ORIENTED_EDGE ( 'NONE', *, *, #43148, .T. ) ;
#10227 = LINE ( 'NONE', #49669, #47609 ) ;
#10228 = DIRECTION ( 'NONE',  ( 0.01601477604151182663, -0.9998717552508123996, 0.000000000000000000 ) ) ;
#10229 = CARTESIAN_POINT ( 'NONE',  ( 1.560669927219590525, 3.346456692913386100, 1.220472440944875281 ) ) ;
#10230 = LINE ( 'NONE', #46080, #11171 ) ;
#10231 = B_SPLINE_CURVE_WITH_KNOTS ( 'NONE', 3,
 ( #39608, #8623, #48333, #32129 ),
 .UNSPECIFIED., .F., .F.,
 ( 4, 4 ),
 ( 2.019292001486067082E-07, 0.01600527235543932475 ),
 .UNSPECIFIED. ) ;
#10232 = ORIENTED_EDGE ( 'NONE', *, *, #16413, .T. ) ;
#10233 = EDGE_LOOP ( 'NONE', ( #10393, #40763, #21471, #18060, #19632, #1852 ) ) ;
#10234 = DIRECTION ( 'NONE',  ( 1.734723475976806848E-16, -0.000000000000000000, 1.000000000000000000 ) ) ;
#10235 = B_SPLINE_CURVE_WITH_KNOTS ( 'NONE', 3,
 ( #19554, #46207, #10864, #30242 ),
 .UNSPECIFIED., .F., .F.,
 ( 4, 4 ),
 ( 0.0002843467791849443676, 0.0004991820216076624152 ),
 .UNSPECIFIED. ) ;
#10236 = CARTESIAN_POINT ( 'NONE',  ( -2.519917724921192370, 1.050329523583607205, 0.3910081006951147686 ) ) ;
#10237 = ORIENTED_EDGE ( 'NONE', *, *, #32088, .F. ) ;
#10238 = EDGE_CURVE ( 'NONE', #42166, #44618, #6669, .T. ) ;
#10239 = LINE ( 'NONE', #41480, #8326 ) ;
#10240 = ADVANCED_FACE ( 'NONE', ( #9524 ), #29657, .F. ) ;
#10241 = ORIENTED_EDGE ( 'NONE', *, *, #25741, .F. ) ;
#10242 = CARTESIAN_POINT ( 'NONE',  ( 0.1968503937007877735, 0.000000000000000000, 2.007874015748021268 ) ) ;
#10243 = EDGE_CURVE ( 'NONE', #19430, #49786, #45122, .T. ) ;
#10244 = CARTESIAN_POINT ( 'NONE',  ( 2.201476786394565011, 1.746575479641379491, 1.240550762682156805 ) ) ;
#10245 = AXIS2_PLACEMENT_3D ( 'NONE', #1182, #28283, #8674 ) ;
#10246 = VERTEX_POINT ( 'NONE', #5902 ) ;
#10247 = DIRECTION ( 'NONE',  ( -3.469446951953613696E-16, 0.000000000000000000, -1.000000000000000000 ) ) ;
#10248 = ORIENTED_EDGE ( 'NONE', *, *, #30175, .T. ) ;
#10249 = ORIENTED_EDGE ( 'NONE', *, *, #34309, .T. ) ;
#10250 = VECTOR ( 'NONE', #37555, 39.37007874015748143 ) ;
#10251 = VECTOR ( 'NONE', #46427, 39.37007874015748143 ) ;
#10252 = ORIENTED_EDGE ( 'NONE', *, *, #30848, .F. ) ;
#10253 = ORIENTED_EDGE ( 'NONE', *, *, #1473, .T. ) ;
#10254 = LINE ( 'NONE', #17745, #14554 ) ;
#10255 = VECTOR ( 'NONE', #20622, 39.37007874015748143 ) ;
#10256 = ORIENTED_EDGE ( 'NONE', *, *, #16427, .T. ) ;
#10257 = CARTESIAN_POINT ( 'NONE',  ( -1.091055626815042645, 0.000000000000000000, 1.889763779527550147 ) ) ;
#10258 = CARTESIAN_POINT ( 'NONE',  ( -1.872964171688006996, 0.5249316497054298258, 0.2040481837739120674 ) ) ;
#10259 = ADVANCED_FACE ( 'NONE', ( #42033 ), #25522, .F. ) ;
#10260 = DIRECTION ( 'NONE',  ( 1.000000000000000000, -0.000000000000000000, 0.000000000000000000 ) ) ;
#10261 = CARTESIAN_POINT ( 'NONE',  ( 0.8182917201112817063, 3.346456692913386100, -2.244094488188969283 ) ) ;
#10262 = DIRECTION ( 'NONE',  ( -1.000000000000000000, -0.000000000000000000, -0.000000000000000000 ) ) ;
#10263 = ORIENTED_EDGE ( 'NONE', *, *, #10433, .F. ) ;
#10264 = PLANE ( 'NONE',  #19194 ) ;
#10265 = LINE ( 'NONE', #14137, #32485 ) ;
#10266 = DIRECTION ( 'NONE',  ( 0.000000000000000000, 0.000000000000000000, -1.000000000000000000 ) ) ;
#10267 = EDGE_CURVE ( 'NONE', #575, #49569, #18287, .T. ) ;
#10268 = LINE ( 'NONE', #13892, #27284 ) ;
#10269 = VERTEX_POINT ( 'NONE', #13912 ) ;
#10270 = CARTESIAN_POINT ( 'NONE',  ( 1.015142113812069979, 3.346456692913386100, 1.912654141836395372 ) ) ;
#10271 = CARTESIAN_POINT ( 'NONE',  ( 2.171725698152134676, 1.651127248238214218, 1.668948176259438254 ) ) ;
#10272 = ORIENTED_EDGE ( 'NONE', *, *, #31159, .F. ) ;
#10273 = DIRECTION ( 'NONE',  ( -1.000000000000000000, -0.000000000000000000, -0.000000000000000000 ) ) ;
#10274 = DIRECTION ( 'NONE',  ( -1.000000000000000000, 0.000000000000000000, 0.000000000000000000 ) ) ;
#10275 = ORIENTED_EDGE ( 'NONE', *, *, #40978, .T. ) ;
#10276 = CIRCLE ( 'NONE', #49802, 2.165354330708661568 ) ;
#10277 = ADVANCED_FACE ( 'NONE', ( #49229 ), #45878, .T. ) ;
#10278 = VECTOR ( 'NONE', #30011, 39.37007874015748143 ) ;
#10279 = VERTEX_POINT ( 'NONE', #10035 ) ;
#10280 = LINE ( 'NONE', #18541, #39647 ) ;
#10281 = VECTOR ( 'NONE', #35870, 39.37007874015748143 ) ;
#10282 = EDGE_CURVE ( 'NONE', #36917, #47149, #25271, .T. ) ;
#10284 = VECTOR ( 'NONE', #19029, 39.37007874015748143 ) ;
#10283 = DIRECTION ( 'NONE',  ( -1.000000000000000000, -0.000000000000000000, -0.000000000000000000 ) ) ;
#10285 = PLANE ( 'NONE',  #32845 ) ;
#10286 = DIRECTION ( 'NONE',  ( -3.469446951953613696E-16, 0.000000000000000000, -1.000000000000000000 ) ) ;
#10287 = CARTESIAN_POINT ( 'NONE',  ( 1.688048600224988149, 0.000000000000000000, -0.4357642695449466252 ) ) ;
#10288 = ORIENTED_EDGE ( 'NONE', *, *, #23615, .T. ) ;
#10289 = CARTESIAN_POINT ( 'NONE',  ( 0.5455278134075216556, 0.000000000000000000, 1.062992125984246083 ) ) ;
#10290 = CONICAL_SURFACE ( 'NONE', #42455, 2.244934639244524632, 1.554780866114618743 ) ;
#10291 = ORIENTED_EDGE ( 'NONE', *, *, #41028, .T. ) ;
#10292 = ORIENTED_EDGE ( 'NONE', *, *, #8555, .T. ) ;
#10293 = DIRECTION ( 'NONE',  ( -1.000000000000000000, -0.000000000000000000, -0.000000000000000000 ) ) ;
#10294 = ORIENTED_EDGE ( 'NONE', *, *, #1975, .F. ) ;
#10295 = LINE ( 'NONE', #2551, #7339 ) ;
#10296 = FACE_OUTER_BOUND ( 'NONE', #38923, .T. ) ;
#10297 = VERTEX_POINT ( 'NONE', #30161 ) ;
#10298 = EDGE_CURVE ( 'NONE', #15130, #35692, #32728, .T. ) ;
#10299 = LINE ( 'NONE', #21664, #30558 ) ;
#10300 =( BOUNDED_CURVE ( )  B_SPLINE_CURVE ( 3, ( #37152, #13147, #9013, #40511 ),
 .UNSPECIFIED., .F., .F. ) 
 B_SPLINE_CURVE_WITH_KNOTS ( ( 4, 4 ),
 ( 3.318026082093744389, 3.368777294715108894 ),
 .UNSPECIFIED. ) 
 CURVE ( )  GEOMETRIC_REPRESENTATION_ITEM ( )  RATIONAL_B_SPLINE_CURVE ( ( 1.000000000000000000, 0.9997853710521733550, 0.9997853710521733550, 1.000000000000000000 ) ) 
 REPRESENTATION_ITEM ( '' )  );
#10301 = LINE ( 'NONE', #50001, #39751 ) ;
#10302 = EDGE_CURVE ( 'NONE', #26738, #11672, #10541, .T. ) ;
#10303 = EDGE_CURVE ( 'NONE', #35318, #42095, #41781, .T. ) ;
#10304 = DIRECTION ( 'NONE',  ( 1.000000000000000000, 0.000000000000000000, 0.000000000000000000 ) ) ;
#10305 = EDGE_LOOP ( 'NONE', ( #40695, #17540, #12078, #28830 ) ) ;
#10306 = ORIENTED_EDGE ( 'NONE', *, *, #50314, .F. ) ;
#10307 = DIRECTION ( 'NONE',  ( -0.1342332658176667026, 0.000000000000000000, 0.9909497617679331460 ) ) ;
#10308 = FACE_BOUND ( 'NONE', #23809, .T. ) ;
#10309 = ORIENTED_EDGE ( 'NONE', *, *, #42340, .T. ) ;
#10310 = LINE ( 'NONE', #49253, #27840 ) ;
#10311 = CARTESIAN_POINT ( 'NONE',  ( -1.909347346926324906, 0.000000000000000000, 1.220472440944875059 ) ) ;
#10312 = ORIENTED_EDGE ( 'NONE', *, *, #28531, .T. ) ;
#10313 = VERTEX_POINT ( 'NONE', #34045 ) ;
#10314 = ADVANCED_FACE ( 'NONE', ( #49729 ), #14415, .F. ) ;
#10315 = CARTESIAN_POINT ( 'NONE',  ( -1.909347346926324462, 3.346456692913386100, 1.102362204724404160 ) ) ;
#10316 = VECTOR ( 'NONE', #11903, 39.37007874015748143 ) ;
#10317 = CARTESIAN_POINT ( 'NONE',  ( -1.597940118745532434, 0.5246043514710795330, -1.459700650569985214 ) ) ;
#10318 = VECTOR ( 'NONE', #18625, 39.37007874015748143 ) ;
#10319 = ORIENTED_EDGE ( 'NONE', *, *, #7310, .F. ) ;
#10320 = VECTOR ( 'NONE', #42826, 39.37007874015748143 ) ;
#10321 = VERTEX_POINT ( 'NONE', #31427 ) ;
#10322 = VECTOR ( 'NONE', #16900, 39.37007874015748143 ) ;
#10323 = ORIENTED_EDGE ( 'NONE', *, *, #5703, .T. ) ;
#10324 = CARTESIAN_POINT ( 'NONE',  ( -1.166969139818015533, 0.000000000000000000, 1.102362204724404160 ) ) ;
#10325 = LINE ( 'NONE', #26069, #46403 ) ;
#10326 = CARTESIAN_POINT ( 'NONE',  ( 0.5455278134075211005, 3.267716535433071279, 0.1181102362204701633 ) ) ;
#10327 = EDGE_CURVE ( 'NONE', #33404, #44569, #11045, .T. ) ;
#10328 = DIRECTION ( 'NONE',  ( 1.000000000000000000, 0.000000000000000000, 0.000000000000000000 ) ) ;
#10329 = ORIENTED_EDGE ( 'NONE', *, *, #47676, .F. ) ;
#10330 = VERTEX_POINT ( 'NONE', #10789 ) ;
#10331 = VECTOR ( 'NONE', #4767, 39.37007874015748143 ) ;
#10332 = DIRECTION ( 'NONE',  ( 1.000000000000000000, 0.000000000000000000, 0.000000000000000000 ) ) ;
#10333 = CARTESIAN_POINT ( 'NONE',  ( 1.287906020515830585, 3.346456692913386100, 1.377952755905504256 ) ) ;
#10334 = B_SPLINE_CURVE_WITH_KNOTS ( 'NONE', 3,
 ( #12859, #39453, #28594, #35583 ),
 .UNSPECIFIED., .F., .F.,
 ( 4, 4 ),
 ( 2.103352892585149584E-07, 0.002500280059082746632 ),
 .UNSPECIFIED. ) ;
#10335 = DIRECTION ( 'NONE',  ( -0.7227948638273978821, 0.000000000000000000, 0.6910626489868580968 ) ) ;
#10336 = ADVANCED_FACE ( 'NONE', ( #11549 ), #26784, .F. ) ;
#10337 = CARTESIAN_POINT ( 'NONE',  ( -1.471105834599418127, 0.000000000000000000, -0.9906718873397587499 ) ) ;
#10338 = EDGE_CURVE ( 'NONE', #19488, #35545, #42278, .T. ) ;
#10339 = LINE ( 'NONE', #21704, #32549 ) ;
#10340 = ADVANCED_FACE ( 'NONE', ( #18545 ), #46134, .T. ) ;
#10341 = CARTESIAN_POINT ( 'NONE',  ( 0.07982360342473591996, 1.709180471932028711, 0.000000000000000000 ) ) ;
#10342 = VERTEX_POINT ( 'NONE', #38421 ) ;
#10343 = PLANE ( 'NONE',  #11065 ) ;
#10344 = DIRECTION ( 'NONE',  ( -0.9998717552508122886, -0.01601477604151182316, 0.000000000000000000 ) ) ;
#10345 = ORIENTED_EDGE ( 'NONE', *, *, #32395, .T. ) ;
#10346 = ORIENTED_EDGE ( 'NONE', *, *, #7781, .T. ) ;
#10347 = DIRECTION ( 'NONE',  ( 0.6427876096865403621, 0.7660444431189770143, 1.858431260983764056E-16 ) ) ;
#10348 = ORIENTED_EDGE ( 'NONE', *, *, #44650, .F. ) ;
#10349 = EDGE_CURVE ( 'NONE', #18986, #26807, #7427, .T. ) ;
#10350 = VECTOR ( 'NONE', #29119, 39.37007874015748143 ) ;
#10351 = AXIS2_PLACEMENT_3D ( 'NONE', #27533, #28048, #43532 ) ;
#10352 = ORIENTED_EDGE ( 'NONE', *, *, #29430, .T. ) ;
#10353 = CARTESIAN_POINT ( 'NONE',  ( -0.8182917201112818173, 3.267716535433071279, 1.419509857074483292E-16 ) ) ;
#10354 = EDGE_CURVE ( 'NONE', #26402, #50880, #42536, .T. ) ;
#10355 = AXIS2_PLACEMENT_3D ( 'NONE', #30487, #6736, #18865 ) ;
#10356 = ORIENTED_EDGE ( 'NONE', *, *, #24977, .T. ) ;
#10357 = PLANE ( 'NONE',  #4572 ) ;
#10358 = DIRECTION ( 'NONE',  ( 1.734723475976806848E-16, -0.000000000000000000, 1.000000000000000000 ) ) ;
#10359 = VECTOR ( 'NONE', #21991, 39.37007874015748143 ) ;
#10360 = ADVANCED_FACE ( 'NONE', ( #23412 ), #22918, .T. ) ;
#10361 = EDGE_CURVE ( 'NONE', #16311, #4534, #34548, .T. ) ;
#10362 = ORIENTED_EDGE ( 'NONE', *, *, #29537, .F. ) ;
#10363 = ORIENTED_EDGE ( 'NONE', *, *, #24096, .F. ) ;
#10364 = VECTOR ( 'NONE', #50, 39.37007874015748143 ) ;
#10365 = CARTESIAN_POINT ( 'NONE',  ( -0.5455278134075216556, 0.000000000000000000, -2.204724409448810540 ) ) ;
#10367 = ORIENTED_EDGE ( 'NONE', *, *, #36639, .T. ) ;
#10366 = EDGE_CURVE ( 'NONE', #47863, #20926, #6918, .T. ) ;
#10368 = ORIENTED_EDGE ( 'NONE', *, *, #1995, .F. ) ;
#10369 = DIRECTION ( 'NONE',  ( -3.469446951953613696E-16, 0.000000000000000000, -1.000000000000000000 ) ) ;
#10370 = DIRECTION ( 'NONE',  ( 0.1785568947986229116, -1.142151789626729957E-16, 0.9839295885986321100 ) ) ;
#10371 = CARTESIAN_POINT ( 'NONE',  ( 1.363819533518803251, 3.346456692913386100, 0.7874015748031454320 ) ) ;
#10372 = CARTESIAN_POINT ( 'NONE',  ( 2.600183657057280051, 0.000000000000000000, 1.399218491554161892 ) ) ;
#10373 = ORIENTED_EDGE ( 'NONE', *, *, #3000, .F. ) ;
#10374 = CARTESIAN_POINT ( 'NONE',  ( 0.000000000000000000, 1.574803149606302854, 0.000000000000000000 ) ) ;
#10375 = PLANE ( 'NONE',  #26665 ) ;
#10376 = CARTESIAN_POINT ( 'NONE',  ( 0.8182917201112819283, 0.000000000000000000, -0.03937007874015881204 ) ) ;
#10377 = VERTEX_POINT ( 'NONE', #30925 ) ;
#10378 = DIRECTION ( 'NONE',  ( 0.000000000000000000, -1.000000000000000000, 0.000000000000000000 ) ) ;
#10379 = CARTESIAN_POINT ( 'NONE',  ( -0.5455278134075214336, 3.346456692913386100, -0.9448818897637762948 ) ) ;
#10380 = CARTESIAN_POINT ( 'NONE',  ( -0.3486774197067339376, 3.346456692913386100, -1.889763779527552146 ) ) ;
#10381 = VERTEX_POINT ( 'NONE', #11797 ) ;
#10382 = ORIENTED_EDGE ( 'NONE', *, *, #30272, .T. ) ;
#10383 = SHAPE_REPRESENTATION_RELATIONSHIP ( 'NONE' , 'NONE' ,  #50787, #7067 ) ;
#10384 = DIRECTION ( 'NONE',  ( 0.000000000000000000, 0.000000000000000000, 1.000000000000000000 ) ) ;
#10385 = CARTESIAN_POINT ( 'NONE',  ( 0.5455278134075216556, 3.346456692913386100, 1.062992125984246083 ) ) ;
#10386 = B_SPLINE_CURVE_WITH_KNOTS ( 'NONE', 3,
 ( #47766, #19666, #7804, #43154 ),
 .UNSPECIFIED., .F., .F.,
 ( 4, 4 ),
 ( 0.01189589409751768030, 0.03073709920686487629 ),
 .UNSPECIFIED. ) ;
#10387 = CARTESIAN_POINT ( 'NONE',  ( 0.5905511811023627100, 0.000000000000000000, 0.000000000000000000 ) ) ;
#10388 = EDGE_LOOP ( 'NONE', ( #48399, #30929, #49194, #48877 ) ) ;
#10389 = ORIENTED_EDGE ( 'NONE', *, *, #14789, .F. ) ;
#10390 = VECTOR ( 'NONE', #37210, 39.37007874015748143 ) ;
#10391 = CIRCLE ( 'NONE', #46614, 2.165354330708661568 ) ;
#10392 = CARTESIAN_POINT ( 'NONE',  ( 2.947574761915768171, 1.666714435463287236, -0.1816379373804911379 ) ) ;
#10393 = ORIENTED_EDGE ( 'NONE', *, *, #35623, .T. ) ;
#10394 = DIRECTION ( 'NONE',  ( -3.469446951953613696E-16, 0.000000000000000000, -1.000000000000000000 ) ) ;
#10395 = AXIS2_PLACEMENT_3D ( 'NONE', #20639, #1017, #13406 ) ;
#10396 = EDGE_CURVE ( 'NONE', #2834, #3813, #1241, .T. ) ;
#10397 = VECTOR ( 'NONE', #7576, 39.37007874015748143 ) ;
#10398 = CARTESIAN_POINT ( 'NONE',  ( 2.140277031474341118, 0.000000000000000000, -0.07969953553056360884 ) ) ;
#10399 = EDGE_CURVE ( 'NONE', #19912, #3116, #34300, .T. ) ;
#10400 = CARTESIAN_POINT ( 'NONE',  ( 1.181102362204724532, 0.5905511811023621549, 1.062992125984251413 ) ) ;
#10401 = CARTESIAN_POINT ( 'NONE',  ( 1.247448100859587239, 0.000000000000000000, -1.633239539486209591 ) ) ;
#10402 = EDGE_LOOP ( 'NONE', ( #40253, #4335, #50610, #44018 ) ) ;
#10403 = DIRECTION ( 'NONE',  ( 1.000000000000000000, -0.000000000000000000, 0.000000000000000000 ) ) ;
#10404 = FILL_AREA_STYLE_COLOUR ( '', #49072 ) ;
#10405 = CARTESIAN_POINT ( 'NONE',  ( 1.775400203342704764, 1.475394431724762478, -2.359903268218703332 ) ) ;
#10406 = VERTEX_POINT ( 'NONE', #46380 ) ;
#10407 = LINE ( 'NONE', #14788, #42196 ) ;
#10408 = LINE ( 'NONE', #17389, #36891 ) ;
#10409 = DIRECTION ( 'NONE',  ( -0.000000000000000000, 1.000000000000000000, -0.000000000000000000 ) ) ;
#10410 = VERTEX_POINT ( 'NONE', #49985 ) ;
#10411 = DIRECTION ( 'NONE',  ( -1.000000000000000000, 0.000000000000000000, -0.000000000000000000 ) ) ;
#10412 = ORIENTED_EDGE ( 'NONE', *, *, #32177, .F. ) ;
#10413 = PLANE ( 'NONE',  #48526 ) ;
#10415 = ORIENTED_EDGE ( 'NONE', *, *, #23474, .F. ) ;
#10414 = EDGE_CURVE ( 'NONE', #13250, #28289, #38919, .T. ) ;
#10416 = DIRECTION ( 'NONE',  ( 0.000000000000000000, 1.000000000000000000, 0.000000000000000000 ) ) ;
#10417 = CARTESIAN_POINT ( 'NONE',  ( 0.7513820654849657776, 1.719936709731724189, 2.142107623314860376 ) ) ;
#10418 = ADVANCED_FACE ( 'NONE', ( #19283 ), #35305, .F. ) ;
#10419 = DIRECTION ( 'NONE',  ( 0.000000000000000000, -1.000000000000000000, 0.000000000000000000 ) ) ;
#10420 = CARTESIAN_POINT ( 'NONE',  ( 0.000000000000000000, 3.346456692913386100, 0.000000000000000000 ) ) ;
#10421 = VECTOR ( 'NONE', #14266, 39.37007874015748143 ) ;
#10422 = ORIENTED_EDGE ( 'NONE', *, *, #6839, .F. ) ;
#10423 = ORIENTED_EDGE ( 'NONE', *, *, #30942, .T. ) ;
#10424 = CARTESIAN_POINT ( 'NONE',  ( 0.2727639067037609943, 3.346456692913386100, 1.220472440944875281 ) ) ;
#10425 = VECTOR ( 'NONE', #29096, 39.37007874015748143 ) ;
#10426 = LINE ( 'NONE', #38558, #45253 ) ;
#10427 = VECTOR ( 'NONE', #28857, 39.37007874015748143 ) ;
#10428 = ADVANCED_FACE ( 'NONE', ( #3552 ), #15428, .T. ) ;
#10429 = ORIENTED_EDGE ( 'NONE', *, *, #8840, .F. ) ;
#10430 = LINE ( 'NONE', #18429, #27512 ) ;
#10431 = CARTESIAN_POINT ( 'NONE',  ( -1.166969139818016199, 0.000000000000000000, -1.614173228346451605 ) ) ;
#10432 = DIRECTION ( 'NONE',  ( 0.01601477604151182663, -0.9998717552508123996, 0.000000000000000000 ) ) ;
#10433 = EDGE_CURVE ( 'NONE', #49700, #43929, #14922, .T. ) ;
#10434 = VECTOR ( 'NONE', #37044, 39.37007874015748143 ) ;
#10435 = ORIENTED_EDGE ( 'NONE', *, *, #44360, .F. ) ;
#10436 = ORIENTED_EDGE ( 'NONE', *, *, #9049, .F. ) ;
#10437 = CARTESIAN_POINT ( 'NONE',  ( 3.927031490892378253E-16, 3.346456692913386100, 1.692913385826762873 ) ) ;
#10438 = CARTESIAN_POINT ( 'NONE',  ( -3.927031490892378253E-16, 3.346456692913386100, -2.204724409448811429 ) ) ;
#10439 = VECTOR ( 'NONE', #46294, 39.37007874015748143 ) ;
#10440 = DIRECTION ( 'NONE',  ( 1.000000000000000000, 0.000000000000000000, 0.000000000000000000 ) ) ;
#10441 = ORIENTED_EDGE ( 'NONE', *, *, #16818, .T. ) ;
#10442 = CARTESIAN_POINT ( 'NONE',  ( 2.437180031585944651, 5.905511811023623991, -1.667735833703098969 ) ) ;
#10444 = VECTOR ( 'NONE', #1411, 39.37007874015748143 ) ;
#10443 = LINE ( 'NONE', #26185, #40875 ) ;
#10445 = ORIENTED_EDGE ( 'NONE', *, *, #33342, .F. ) ;
#10446 = LINE ( 'NONE', #45525, #27361 ) ;
#10447 = VERTEX_POINT ( 'NONE', #4833 ) ;
#10448 = VERTEX_POINT ( 'NONE', #4312 ) ;
#10449 = CARTESIAN_POINT ( 'NONE',  ( -2.164823134740035737, 1.574803149606302854, -0.04796011690018223833 ) ) ;
#10450 = DIRECTION ( 'NONE',  ( -3.986037398843765983E-20, -1.000000000000000000, -1.160734090543304660E-16 ) ) ;
#10451 = DIRECTION ( 'NONE',  ( -1.000000000000000000, 0.000000000000000000, -0.000000000000000000 ) ) ;
#10452 = ORIENTED_EDGE ( 'NONE', *, *, #24585, .T. ) ;
#10453 = CARTESIAN_POINT ( 'NONE',  ( -0.04921259842519708216, 1.608688524157807498, 2.242709805336809303 ) ) ;
#10454 = CARTESIAN_POINT ( 'NONE',  ( -1.712496953225537633, 0.000000000000000000, -0.7874015748031470974 ) ) ;
#10455 = EDGE_LOOP ( 'NONE', ( #38513, #10710, #3916, #46771 ) ) ;
#10456 = ORIENTED_EDGE ( 'NONE', *, *, #46972, .F. ) ;
#10457 = DIRECTION ( 'NONE',  ( 1.734723475976806848E-16, 0.000000000000000000, 1.000000000000000000 ) ) ;
#10458 = CARTESIAN_POINT ( 'NONE',  ( -2.339241080213612545, 1.682800407567106360, 1.802537235681883843 ) ) ;
#10459 = VECTOR ( 'NONE', #32451, 39.37007874015748143 ) ;
#10460 = CARTESIAN_POINT ( 'NONE',  ( -1.181102362204724088, 0.000000000000000000, 1.181102362204724088 ) ) ;
#10461 = ADVANCED_FACE ( 'NONE', ( #35811 ), #20313, .F. ) ;
#10462 = LINE ( 'NONE', #16366, #15357 ) ;
#10463 = FACE_OUTER_BOUND ( 'NONE', #41959, .T. ) ;
#10464 = AXIS2_PLACEMENT_3D ( 'NONE', #14646, #42510, #38650 ) ;
#10465 = EDGE_LOOP ( 'NONE', ( #30673, #47985, #1808, #39662 ) ) ;
#10466 = EDGE_CURVE ( 'NONE', #12085, #47811, #439, .T. ) ;
#10467 = CARTESIAN_POINT ( 'NONE',  ( -0.07591351300297359550, 0.000000000000000000, -2.047244094488181343 ) ) ;
#10468 = DIRECTION ( 'NONE',  ( -3.469446951953613696E-16, 0.000000000000000000, -1.000000000000000000 ) ) ;
#10469 = EDGE_CURVE ( 'NONE', #9339, #35392, #36071, .T. ) ;
#10470 = VERTEX_POINT ( 'NONE', #28826 ) ;
#10471 = CARTESIAN_POINT ( 'NONE',  ( -2.889674983507168893, 5.905511811023623991, -0.6090712660038039017 ) ) ;
#10472 = CARTESIAN_POINT ( 'NONE',  ( 2.164658444855302122, 5.905511811023623991, -0.04795272066889885720 ) ) ;
#10473 = EDGE_LOOP ( 'NONE', ( #29433, #2930, #31253, #23496 ) ) ;
#10474 = CARTESIAN_POINT ( 'NONE',  ( -2.165354330708661568, 3.346456692913386100, -6.146657985744592735E-16 ) ) ;
#10475 = VECTOR ( 'NONE', #20142, 39.37007874015748143 ) ;
#10476 = EDGE_CURVE ( 'NONE', #47415, #15540, #7461, .T. ) ;
#10477 = FACE_OUTER_BOUND ( 'NONE', #15905, .T. ) ;
#10478 = FACE_OUTER_BOUND ( 'NONE', #1853, .T. ) ;
#10479 = VECTOR ( 'NONE', #21737, 39.37007874015748143 ) ;
#10480 = ORIENTED_EDGE ( 'NONE', *, *, #48467, .T. ) ;
#10481 = DIRECTION ( 'NONE',  ( 0.000000000000000000, 0.000000000000000000, -1.000000000000000000 ) ) ;
#10482 = ORIENTED_EDGE ( 'NONE', *, *, #6100, .T. ) ;
#10483 = FACE_BOUND ( 'NONE', #37007, .T. ) ;
#10484 = DIRECTION ( 'NONE',  ( -0.9998717552508122886, -0.01601477604151181275, 0.000000000000000000 ) ) ;
#10485 = CARTESIAN_POINT ( 'NONE',  ( 1.560669927219590303, 3.346456692913386100, -1.929133858267710666 ) ) ;
#10486 = EDGE_CURVE ( 'NONE', #16772, #4281, #32203, .T. ) ;
#10487 = LINE ( 'NONE', #49174, #7851 ) ;
#10488 = VERTEX_POINT ( 'NONE', #12834 ) ;
#10489 = ORIENTED_EDGE ( 'NONE', *, *, #27716, .T. ) ;
#10490 = FACE_OUTER_BOUND ( 'NONE', #32850, .T. ) ;
#10491 = DIRECTION ( 'NONE',  ( -1.000000000000000000, 0.000000000000000000, -0.000000000000000000 ) ) ;
#10492 = EDGE_CURVE ( 'NONE', #2736, #23094, #23934, .T. ) ;
#10493 = DIRECTION ( 'NONE',  ( 1.000000000000000000, 0.000000000000000000, 0.000000000000000000 ) ) ;
#10494 = PLANE ( 'NONE',  #4645 ) ;
#10495 = VERTEX_POINT ( 'NONE', #9211 ) ;
#10496 = CARTESIAN_POINT ( 'NONE',  ( -1.556712866041156440, 1.694999912340861004, 2.509548638715847435 ) ) ;
#10497 = ORIENTED_EDGE ( 'NONE', *, *, #44380, .F. ) ;
#10498 = LINE ( 'NONE', #2242, #46358 ) ;
#10499 = VECTOR ( 'NONE', #2283, 39.37007874015748143 ) ;
#10500 = VECTOR ( 'NONE', #48076, 39.37007874015748854 ) ;
#10501 = CARTESIAN_POINT ( 'NONE',  ( 0.08139965876239094178, 1.610780518492231694, 0.000000000000000000 ) ) ;
#10502 = VECTOR ( 'NONE', #32184, 39.37007874015748143 ) ;
#10503 = ORIENTED_EDGE ( 'NONE', *, *, #21992, .F. ) ;
#10504 = CARTESIAN_POINT ( 'NONE',  ( 0.1067246931122726866, 0.02962905676920215767, 0.000000000000000000 ) ) ;
#10505 = ORIENTED_EDGE ( 'NONE', *, *, #24027, .T. ) ;
#10506 = ORIENTED_EDGE ( 'NONE', *, *, #35719, .T. ) ;
#10507 = EDGE_CURVE ( 'NONE', #37481, #1147, #20576, .T. ) ;
#10508 = ORIENTED_EDGE ( 'NONE', *, *, #29061, .T. ) ;
#10509 = EDGE_LOOP ( 'NONE', ( #7254, #138, #29791, #8883 ) ) ;
#10510 = DIRECTION ( 'NONE',  ( 1.000000000000000000, 0.000000000000000000, -3.469446951953613696E-16 ) ) ;
#10511 = EDGE_LOOP ( 'NONE', ( #42615, #23896, #11800, #2124 ) ) ;
#10513 = DIRECTION ( 'NONE',  ( -0.000000000000000000, 1.000000000000000000, -0.000000000000000000 ) ) ;
#10512 = VECTOR ( 'NONE', #7715, 39.37007874015748143 ) ;
#10514 = CARTESIAN_POINT ( 'NONE',  ( -0.6214413264104942103, 3.267716535433071279, 2.156057715732900040E-16 ) ) ;
#10515 = DIRECTION ( 'NONE',  ( -0.000000000000000000, 1.000000000000000000, -0.000000000000000000 ) ) ;
#10516 = CARTESIAN_POINT ( 'NONE',  ( 1.678360014056755389, 0.9972678649800447159, 1.995835756311929110 ) ) ;
#10517 = DIRECTION ( 'NONE',  ( 0.7660444431189771253, 0.6427876096865404731, -6.644376395600348305E-17 ) ) ;
#10518 = ORIENTED_EDGE ( 'NONE', *, *, #35917, .T. ) ;
#10519 = EDGE_CURVE ( 'NONE', #39188, #37274, #44312, .T. ) ;
#10520 = CARTESIAN_POINT ( 'NONE',  ( -0.8182917201112814842, 3.346456692913386100, 1.102362204724404160 ) ) ;
#10521 = DIRECTION ( 'NONE',  ( -0.000000000000000000, 1.000000000000000000, -0.000000000000000000 ) ) ;
#10522 = LINE ( 'NONE', #30399, #19389 ) ;
#10523 = DIRECTION ( 'NONE',  ( 0.000000000000000000, 0.000000000000000000, 1.000000000000000000 ) ) ;
#10524 = ADVANCED_FACE ( 'NONE', ( #4068 ), #8956, .T. ) ;
#10525 = VERTEX_POINT ( 'NONE', #43794 ) ;
#10526 = DIRECTION ( 'NONE',  ( -3.469446951953613696E-16, 0.000000000000000000, -1.000000000000000000 ) ) ;
#10527 = EDGE_CURVE ( 'NONE', #23763, #11950, #31948, .T. ) ;
#10528 = DIRECTION ( 'NONE',  ( -0.000000000000000000, 1.000000000000000000, -0.000000000000000000 ) ) ;
#10529 = ORIENTED_EDGE ( 'NONE', *, *, #28625, .T. ) ;
#10530 = CARTESIAN_POINT ( 'NONE',  ( 2.951990591674675368, 5.905511811023623991, -0.08331184815398307020 ) ) ;
#10531 = VECTOR ( 'NONE', #12502, 39.37007874015748143 ) ;
#10532 = VECTOR ( 'NONE', #37979, 39.37007874015748143 ) ;
#10533 = EDGE_CURVE ( 'NONE', #32010, #31869, #39937, .T. ) ;
#10534 = DIRECTION ( 'NONE',  ( 1.000000000000000000, -0.000000000000000000, 0.000000000000000000 ) ) ;
#10535 = VERTEX_POINT ( 'NONE', #16968 ) ;
#10536 = CIRCLE ( 'NONE', #31206, 2.165354330708661568 ) ;
#10537 = ORIENTED_EDGE ( 'NONE', *, *, #31782, .F. ) ;
#10538 = DIRECTION ( 'NONE',  ( 0.7071067811865483499, 1.579007132194770110E-15, -0.7071067811865466846 ) ) ;
#10539 = DIRECTION ( 'NONE',  ( 0.000000000000000000, 0.000000000000000000, -1.000000000000000000 ) ) ;
#10540 = FACE_OUTER_BOUND ( 'NONE', #49697, .T. ) ;
#10541 = LINE ( 'NONE', #41526, #21006 ) ;
#10542 = EDGE_CURVE ( 'NONE', #11695, #15891, #35555, .T. ) ;
#10543 = PLANE ( 'NONE',  #31892 ) ;
#10544 = VERTEX_POINT ( 'NONE', #47385 ) ;
#10545 = VECTOR ( 'NONE', #22701, 39.37007874015748143 ) ;
#10546 = CARTESIAN_POINT ( 'NONE',  ( 1.983515723912132378, 0.6859011407150840123, -3.558318873518431236 ) ) ;
#10547 = ORIENTED_EDGE ( 'NONE', *, *, #815, .T. ) ;
#10548 = VERTEX_POINT ( 'NONE', #20043 ) ;
#10549 = DIRECTION ( 'NONE',  ( -3.469446951953613696E-16, 0.000000000000000000, -1.000000000000000000 ) ) ;
#10550 = ORIENTED_EDGE ( 'NONE', *, *, #9113, .F. ) ;
#10551 = EDGE_CURVE ( 'NONE', #40146, #40614, #12318, .T. ) ;
#10552 = DIRECTION ( 'NONE',  ( -0.6579387259397138088, -8.738534663690390683E-17, 0.7530714660036099684 ) ) ;
#10553 = AXIS2_PLACEMENT_3D ( 'NONE', #25956, #41449, #45544 ) ;
#10554 = LINE ( 'NONE', #3059, #22740 ) ;
#10555 = ORIENTED_EDGE ( 'NONE', *, *, #30211, .F. ) ;
#10556 = DIRECTION ( 'NONE',  ( -0.000000000000000000, 1.000000000000000000, -0.000000000000000000 ) ) ;
#10557 = EDGE_CURVE ( 'NONE', #31520, #18162, #49812, .T. ) ;
#10558 = LINE ( 'NONE', #49495, #15833 ) ;
#10559 = CARTESIAN_POINT ( 'NONE',  ( 2.919426793319799707, 0.000000000000000000, 0.4451252810446820196 ) ) ;
#10560 = VERTEX_POINT ( 'NONE', #28053 ) ;
#10561 = ORIENTED_EDGE ( 'NONE', *, *, #5710, .T. ) ;
#10562 = PLANE ( 'NONE',  #20743 ) ;
#10563 = FACE_BOUND ( 'NONE', #47647, .T. ) ;
#10564 = ORIENTED_EDGE ( 'NONE', *, *, #33072, .T. ) ;
#10565 = EDGE_CURVE ( 'NONE', #26163, #40779, #4574, .T. ) ;
#10566 = CARTESIAN_POINT ( 'NONE',  ( 2.069629837364519886, 3.267716535433071279, -1.299212598425194320 ) ) ;
#10567 = CARTESIAN_POINT ( 'NONE',  ( 2.947574761915768171, 1.666714435463287236, -0.1816379373804911379 ) ) ;
#10568 = VECTOR ( 'NONE', #39804, 39.37007874015748143 ) ;
#10569 = VECTOR ( 'NONE', #11300, 39.37007874015748143 ) ;
#10570 = ORIENTED_EDGE ( 'NONE', *, *, #3910, .F. ) ;
#10571 = EDGE_LOOP ( 'NONE', ( #47866, #20010, #3386, #21874 ) ) ;
#10572 = DIRECTION ( 'NONE',  ( 1.000000000000000000, 0.000000000000000000, -3.469446951953613696E-16 ) ) ;
#10573 = LINE ( 'NONE', #50508, #31180 ) ;
#10574 = EDGE_CURVE ( 'NONE', #47459, #4557, #44052, .T. ) ;
#10575 = EDGE_LOOP ( 'NONE', ( #48532, #27670, #44801, #4745 ) ) ;
#10576 = ORIENTED_EDGE ( 'NONE', *, *, #22635, .F. ) ;
#10577 = CONICAL_SURFACE ( 'NONE', #24612, 3.483074324928249421, 1.244861948955335196 ) ;
#10579 = EDGE_CURVE ( 'NONE', #31953, #47312, #46109, .T. ) ;
#10578 = ORIENTED_EDGE ( 'NONE', *, *, #37477, .F. ) ;
#10580 = DIRECTION ( 'NONE',  ( -1.000000000000000000, 0.000000000000000000, 1.734723475976806848E-16 ) ) ;
#10581 = FACE_OUTER_BOUND ( 'NONE', #32876, .T. ) ;
#10582 = VECTOR ( 'NONE', #18670, 39.37007874015748143 ) ;
#10583 = DIRECTION ( 'NONE',  ( -3.469446951953613696E-16, 0.000000000000000000, -1.000000000000000000 ) ) ;
#10584 = CIRCLE ( 'NONE', #31215, 2.165354330708661568 ) ;
#10585 = ORIENTED_EDGE ( 'NONE', *, *, #39902, .F. ) ;
#10586 = ORIENTED_EDGE ( 'NONE', *, *, #33098, .T. ) ;
#10587 = DIRECTION ( 'NONE',  ( 0.000000000000000000, -1.000000000000000000, 0.000000000000000000 ) ) ;
#10588 = DIRECTION ( 'NONE',  ( -0.000000000000000000, 1.000000000000000000, -0.000000000000000000 ) ) ;
#10589 = B_SPLINE_CURVE_WITH_KNOTS ( 'NONE', 3,
 ( #39145, #18325, #13949, #26072 ),
 .UNSPECIFIED., .F., .F.,
 ( 4, 4 ),
 ( 2.018265806504230573E-07, 0.02001440840492994117 ),
 .UNSPECIFIED. ) ;
#10590 = CARTESIAN_POINT ( 'NONE',  ( 1.083598637574782142, 1.491270273546293046, 2.747180975113346246 ) ) ;
#10591 = VECTOR ( 'NONE', #5128, 39.37007874015748143 ) ;
#10592 = CARTESIAN_POINT ( 'NONE',  ( -0.4462886659516242527, 1.602328624241157851, 2.183640264916793861 ) ) ;
#10593 = CARTESIAN_POINT ( 'NONE',  ( -1.503492009532958695, 1.205361022782829114E-17, -0.9334790059352082725 ) ) ;
#10594 = EDGE_CURVE ( 'NONE', #33946, #8577, #1974, .T. ) ;
#10595 = DIRECTION ( 'NONE',  ( 8.902872254219889125E-17, 1.000000000000000000, 9.311674343991287120E-17 ) ) ;
#10596 = EDGE_CURVE ( 'NONE', #24456, #25931, #2233, .T. ) ;
#10597 = DIRECTION ( 'NONE',  ( 1.000000000000000000, 0.000000000000000000, 0.000000000000000000 ) ) ;
#10598 = ORIENTED_EDGE ( 'NONE', *, *, #20263, .T. ) ;
#10599 = LINE ( 'NONE', #14209, #13542 ) ;
#10600 = CARTESIAN_POINT ( 'NONE',  ( 0.000000000000000000, 3.267716535433071279, -0.6692913385826764205 ) ) ;
#10601 = ORIENTED_EDGE ( 'NONE', *, *, #45917, .T. ) ;
#10602 = ORIENTED_EDGE ( 'NONE', *, *, #35063, .T. ) ;
#10603 = DIRECTION ( 'NONE',  ( 0.000000000000000000, 1.000000000000000000, 0.000000000000000000 ) ) ;
#10604 = AXIS2_PLACEMENT_3D ( 'NONE', #31123, #19988, #35250 ) ;
#10605 = VERTEX_POINT ( 'NONE', #14101 ) ;
#10606 = EDGE_LOOP ( 'NONE', ( #30530, #48957, #5986, #18579 ) ) ;
#10607 = LINE ( 'NONE', #38241, #29563 ) ;
#10608 = CONICAL_SURFACE ( 'NONE', #30398, 2.246510896728926010, 0.01601546068027819014 ) ;
#10609 = ORIENTED_EDGE ( 'NONE', *, *, #28866, .F. ) ;
#10610 = VECTOR ( 'NONE', #9421, 39.37007874015748143 ) ;
#10611 = AXIS2_PLACEMENT_3D ( 'NONE', #9665, #41166, #1911 ) ;
#10612 = CARTESIAN_POINT ( 'NONE',  ( 1.062992125984251413, 0.5905511811023621549, -1.181102362204724754 ) ) ;
#10613 = CARTESIAN_POINT ( 'NONE',  ( -2.182111253630085290, 3.346456692913386100, -0.1968503937007880511 ) ) ;
#10614 = EDGE_CURVE ( 'NONE', #8862, #37378, #40972, .T. ) ;
#10615 = VECTOR ( 'NONE', #42128, 39.37007874015748143 ) ;
#10616 = ORIENTED_EDGE ( 'NONE', *, *, #19113, .F. ) ;
#10617 = DIRECTION ( 'NONE',  ( -8.881784197001250746E-15, 0.000000000000000000, 1.000000000000000000 ) ) ;
#10618 = ORIENTED_EDGE ( 'NONE', *, *, #3780, .T. ) ;
#10619 = ORIENTED_EDGE ( 'NONE', *, *, #40773, .F. ) ;
#10620 = CARTESIAN_POINT ( 'NONE',  ( -2.182111253630085290, 3.267716535433071279, 3.785359618865289765E-16 ) ) ;
#10621 = CARTESIAN_POINT ( 'NONE',  ( -2.014599508217050250, 1.642826054184012508, -0.8075617281263232083 ) ) ;
#10622 = CARTESIAN_POINT ( 'NONE',  ( 1.363819533518803251, 0.000000000000000000, 1.417322834645662777 ) ) ;
#10623 = LINE ( 'NONE', #25599, #10359 ) ;
#10624 = VECTOR ( 'NONE', #44044, 39.37007874015748143 ) ;
#10625 = EDGE_CURVE ( 'NONE', #11936, #20750, #41224, .T. ) ;
#10626 = ORIENTED_EDGE ( 'NONE', *, *, #15201, .T. ) ;
#10627 = ADVANCED_FACE ( 'NONE', ( #33231 ), #30114, .T. ) ;
#10628 = LINE ( 'NONE', #41360, #37010 ) ;
#10629 = LINE ( 'NONE', #42113, #39866 ) ;
#10630 = LINE ( 'NONE', #29738, #609 ) ;
#10631 = EDGE_CURVE ( 'NONE', #12457, #41521, #30103, .T. ) ;
#10632 = ORIENTED_EDGE ( 'NONE', *, *, #29666, .F. ) ;
#10633 = LINE ( 'NONE', #14504, #13372 ) ;
#10634 = DIRECTION ( 'NONE',  ( 0.01601477604151182663, -0.9998717552508123996, 0.000000000000000000 ) ) ;
#10635 = ADVANCED_FACE ( 'NONE', ( #5591 ), #6098, .F. ) ;
#10636 = EDGE_LOOP ( 'NONE', ( #34302, #25402, #34335, #27275 ) ) ;
#10637 = VERTEX_POINT ( 'NONE', #21089 ) ;
#10638 = DIRECTION ( 'NONE',  ( -0.5006757388967129074, 0.09282933006792923325, 0.8606430851168036522 ) ) ;
#10639 = DIRECTION ( 'NONE',  ( -0.000000000000000000, 1.000000000000000000, -0.000000000000000000 ) ) ;
#10640 = VECTOR ( 'NONE', #32339, 39.37007874015748143 ) ;
#10641 = CARTESIAN_POINT ( 'NONE',  ( 0.000000000000000000, 3.267716535433071279, 1.692913385826762873 ) ) ;
#10642 = LINE ( 'NONE', #17624, #47705 ) ;
#10643 = VERTEX_POINT ( 'NONE', #45567 ) ;
#10644 = ORIENTED_EDGE ( 'NONE', *, *, #34449, .F. ) ;
#10645 = CARTESIAN_POINT ( 'NONE',  ( -0.8182917201112819283, 0.000000000000000000, 2.047244094488179567 ) ) ;
#10646 = LINE ( 'NONE', #10133, #24314 ) ;
#10647 = ORIENTED_EDGE ( 'NONE', *, *, #25800, .T. ) ;
#10648 = LINE ( 'NONE', #26388, #35669 ) ;
#10649 = CARTESIAN_POINT ( 'NONE',  ( 0.000000000000000000, 3.267716535433071279, -2.204724409448810540 ) ) ;
#10650 = EDGE_CURVE ( 'NONE', #43639, #8308, #49173, .T. ) ;
#10651 = CONICAL_SURFACE ( 'NONE', #39491, 2.165354330708661568, 0.2617993877991570129 ) ;
#10652 = VECTOR ( 'NONE', #1943, 39.37007874015748143 ) ;
#10653 = ADVANCED_FACE ( 'NONE', ( #25463 ), #18229, .F. ) ;
#10654 = VECTOR ( 'NONE', #30354, 39.37007874015748143 ) ;
#10655 = CARTESIAN_POINT ( 'NONE',  ( 1.286500945617783609, 0.5223259443140828573, -1.854442115480348541 ) ) ;
#10656 = CARTESIAN_POINT ( 'NONE',  ( -1.712496953225537188, 0.000000000000000000, -0.1574803149606297248 ) ) ;
#10657 = PLANE ( 'NONE',  #11388 ) ;
#10658 = VERTEX_POINT ( 'NONE', #10229 ) ;
#10659 = CARTESIAN_POINT ( 'NONE',  ( -1.363819533518803473, 3.267716535433071279, 1.681890501046756192 ) ) ;
#10660 =( CONVERSION_BASED_UNIT ( 'INCH', #19391 ) LENGTH_UNIT ( ) NAMED_UNIT ( #7980 ) );
#10661 = VECTOR ( 'NONE', #30601, 39.37007874015748143 ) ;
#10662 = DIRECTION ( 'NONE',  ( 0.000000000000000000, 0.000000000000000000, 1.000000000000000000 ) ) ;
#10663 = ORIENTED_EDGE ( 'NONE', *, *, #11, .T. ) ;
#10664 = CARTESIAN_POINT ( 'NONE',  ( -0.07591351300297348448, 3.267716535433071279, 2.633779063002574070E-17 ) ) ;
#10665 = CARTESIAN_POINT ( 'NONE',  ( 2.491402175429654253, 1.758084086496218612, -1.585592796919505609 ) ) ;
#10666 = CARTESIAN_POINT ( 'NONE',  ( -0.3486774197067334380, 0.000000000000000000, 0.9448818897637749625 ) ) ;
#10667 = ORIENTED_EDGE ( 'NONE', *, *, #29358, .T. ) ;
#10668 = EDGE_CURVE ( 'NONE', #7899, #46993, #1459, .T. ) ;
#10669 = FACE_OUTER_BOUND ( 'NONE', #26939, .T. ) ;
#10670 = VERTEX_POINT ( 'NONE', #10485 ) ;
#10671 = CARTESIAN_POINT ( 'NONE',  ( -1.722370577523733459, 1.205361022782829114E-17, 0.2829729990490794655 ) ) ;
#10672 = ORIENTED_EDGE ( 'NONE', *, *, #23252, .F. ) ;
#10673 = PLANE ( 'NONE',  #45144 ) ;
#10674 = LINE ( 'NONE', #46015, #34280 ) ;
#10675 = FACE_OUTER_BOUND ( 'NONE', #3706, .T. ) ;
#10676 = DIRECTION ( 'NONE',  ( 0.000000000000000000, -1.000000000000000000, 0.000000000000000000 ) ) ;
#10677 = VECTOR ( 'NONE', #18110, 39.37007874015748143 ) ;
#10678 = ORIENTED_EDGE ( 'NONE', *, *, #21417, .F. ) ;
#10679 = ORIENTED_EDGE ( 'NONE', *, *, #36350, .T. ) ;
#10680 = CARTESIAN_POINT ( 'NONE',  ( -1.536664496436148184E-16, 3.346456692913386100, -1.141732283464564013 ) ) ;
#10681 = CARTESIAN_POINT ( 'NONE',  ( -1.593029370565769431, 3.267716535433071279, 1.377952755905504256 ) ) ;
#10682 = VERTEX_POINT ( 'NONE', #25975 ) ;
#10683 = DIRECTION ( 'NONE',  ( 1.734723475976806848E-16, -0.000000000000000000, 1.000000000000000000 ) ) ;
#10684 = LINE ( 'NONE', #38317, #23609 ) ;
#10685 = CARTESIAN_POINT ( 'NONE',  ( -1.363819533518803029, 3.267716535433071279, 2.365849761790804994E-16 ) ) ;
#10686 = VECTOR ( 'NONE', #35649, 39.37007874015748143 ) ;
#10687 = ORIENTED_EDGE ( 'NONE', *, *, #16855, .T. ) ;
#10688 = ORIENTED_EDGE ( 'NONE', *, *, #51039, .F. ) ;
#10689 = ADVANCED_FACE ( 'NONE', ( #9974 ), #17219, .F. ) ;
#10690 = LINE ( 'NONE', #2182, #4831 ) ;
#10691 = CARTESIAN_POINT ( 'NONE',  ( -1.684292108503798069, 5.905511811023623991, 1.406123411605399331 ) ) ;
#10692 = CARTESIAN_POINT ( 'NONE',  ( 1.560669927219590747, 0.000000000000000000, 0.7874015748031454320 ) ) ;
#10693 = EDGE_CURVE ( 'NONE', #16832, #46970, #5845, .T. ) ;
#10694 = EDGE_LOOP ( 'NONE', ( #22739, #13405, #20032, #48237, #48472 ) ) ;
#10695 = CARTESIAN_POINT ( 'NONE',  ( 1.015142113812069091, 3.346456692913386100, -1.845530509571139399 ) ) ;
#10696 = EDGE_CURVE ( 'NONE', #18996, #36035, #41646, .T. ) ;
#10697 = LINE ( 'NONE', #45776, #12015 ) ;
#10698 = ORIENTED_EDGE ( 'NONE', *, *, #1783, .T. ) ;
#10699 = CARTESIAN_POINT ( 'NONE',  ( 1.560669927219590747, 3.346456692913386100, 1.414498409778230492 ) ) ;
#10700 = VERTEX_POINT ( 'NONE', #22108 ) ;
#10701 = ORIENTED_EDGE ( 'NONE', *, *, #19402, .F. ) ;
#10702 = AXIS2_PLACEMENT_3D ( 'NONE', #4944, #16568, #43402 ) ;
#10703 = CARTESIAN_POINT ( 'NONE',  ( 0.2509731715796156282, 1.646304950397431410, -2.239533430214235121 ) ) ;
#10704 = CARTESIAN_POINT ( 'NONE',  ( 1.062992125984251413, 0.5905511811023621549, -1.062992125984252079 ) ) ;
#10705 = DIRECTION ( 'NONE',  ( 0.000000000000000000, 0.9659258262890662028, 0.2588190451025280114 ) ) ;
#10706 = DIRECTION ( 'NONE',  ( -0.000000000000000000, 1.000000000000000000, -0.000000000000000000 ) ) ;
#10707 = DIRECTION ( 'NONE',  ( -0.8805955318567322276, 0.000000000000000000, -0.4738686624730094610 ) ) ;
#10708 = ORIENTED_EDGE ( 'NONE', *, *, #35077, .F. ) ;
#10709 = ADVANCED_FACE ( 'NONE', ( #41471 ), #13599, .F. ) ;
#10710 = ORIENTED_EDGE ( 'NONE', *, *, #9538, .T. ) ;
#10711 = DIRECTION ( 'NONE',  ( -1.000000000000000000, 0.000000000000000000, 1.734723475976806848E-16 ) ) ;
#10712 = CARTESIAN_POINT ( 'NONE',  ( -2.298329623231348151, 1.683429673656728465, 1.853838580093637445 ) ) ;
#10713 = ADVANCED_FACE ( 'NONE', ( #13851 ), #45317, .T. ) ;
#10714 = VECTOR ( 'NONE', #37938, 39.37007874015748143 ) ;
#10715 = CARTESIAN_POINT ( 'NONE',  ( 1.733526556417521958, 0.000000000000000000, 0.1851600754179809072 ) ) ;
#10716 = EDGE_CURVE ( 'NONE', #31608, #26125, #15369, .T. ) ;
#10717 = LINE ( 'NONE', #41957, #26160 ) ;
#10718 = DIRECTION ( 'NONE',  ( -3.469446951953613696E-16, 0.000000000000000000, -1.000000000000000000 ) ) ;
#10719 = ORIENTED_EDGE ( 'NONE', *, *, #48004, .F. ) ;
#10720 = CARTESIAN_POINT ( 'NONE',  ( 1.363819533518803251, 3.346456692913386100, -0.1574803149606304187 ) ) ;
#10721 = ADVANCED_FACE ( 'NONE', ( #39111 ), #6196, .T. ) ;
#10722 = LINE ( 'NONE', #31101, #44637 ) ;
#10723 = VECTOR ( 'NONE', #24741, 39.37007874015748143 ) ;
#10724 = ORIENTED_EDGE ( 'NONE', *, *, #3103, .F. ) ;
#10725 = LINE ( 'NONE', #22849, #49528 ) ;
#10726 = CARTESIAN_POINT ( 'NONE',  ( -1.377952755905512472, 0.000000000000000000, -2.845674993400276405E-16 ) ) ;
#10727 = ORIENTED_EDGE ( 'NONE', *, *, #34603, .F. ) ;
#10728 = CARTESIAN_POINT ( 'NONE',  ( -1.879299076992925199, 0.5249316497054292707, -0.1336616210507489411 ) ) ;
#10729 = CARTESIAN_POINT ( 'NONE',  ( 0.000000000000000000, 1.574803149606302854, 0.000000000000000000 ) ) ;
#10730 = CARTESIAN_POINT ( 'NONE',  ( 0.000000000000000000, 2.755905511811024056, 0.000000000000000000 ) ) ;
#10731 = EDGE_LOOP ( 'NONE', ( #8633, #18588, #39422, #25079 ) ) ;
#10732 = DIRECTION ( 'NONE',  ( -3.469446951953613696E-16, 0.000000000000000000, -1.000000000000000000 ) ) ;
#10733 = EDGE_LOOP ( 'NONE', ( #45256, #39643, #35981, #17772 ) ) ;
#10734 = B_SPLINE_CURVE_WITH_KNOTS ( 'NONE', 3,
 ( #15601, #11224, #22588, #34972 ),
 .UNSPECIFIED., .F., .F.,
 ( 4, 4 ),
 ( 0.03086743659920977365, 0.04894270564625235326 ),
 .UNSPECIFIED. ) ;
#10735 = FACE_BOUND ( 'NONE', #44607, .T. ) ;
#10736 = CARTESIAN_POINT ( 'NONE',  ( 0.000000000000000000, 3.267716535433071279, -1.259842519685034690 ) ) ;
#10737 = CARTESIAN_POINT ( 'NONE',  ( -1.636583440222564301, 3.346456692913386100, -1.771653543307080581 ) ) ;
#10738 = ORIENTED_EDGE ( 'NONE', *, *, #13683, .T. ) ;
#10739 = VERTEX_POINT ( 'NONE', #46819 ) ;
#10740 = PLANE ( 'NONE',  #27323 ) ;
#10741 = LINE ( 'NONE', #14106, #15574 ) ;
#10742 = FACE_OUTER_BOUND ( 'NONE', #39963, .T. ) ;
#10743 = CARTESIAN_POINT ( 'NONE',  ( -1.721400284384397628, 0.0003482895740541699209, 0.2828415639128913361 ) ) ;
#10744 = LINE ( 'NONE', #30372, #10798 ) ;
#10745 = ORIENTED_EDGE ( 'NONE', *, *, #17782, .F. ) ;
#10746 = ORIENTED_EDGE ( 'NONE', *, *, #39136, .F. ) ;
#10747 = CARTESIAN_POINT ( 'NONE',  ( 1.560669927219590303, 0.000000000000000000, -1.614173228346452715 ) ) ;
#10748 = DIRECTION ( 'NONE',  ( -0.01601477604151182663, 0.9998717552508123996, -0.000000000000000000 ) ) ;
#10749 = EDGE_CURVE ( 'NONE', #5755, #23656, #46079, .T. ) ;
#10750 = VERTEX_POINT ( 'NONE', #6616 ) ;
#10751 = EDGE_CURVE ( 'NONE', #18996, #30156, #16609, .T. ) ;
#10752 = CARTESIAN_POINT ( 'NONE',  ( -0.8942052331142552601, 3.346456692913386100, -1.456692913385822186 ) ) ;
#10753 = ORIENTED_EDGE ( 'NONE', *, *, #2112, .F. ) ;
#10754 = ORIENTED_EDGE ( 'NONE', *, *, #2102, .F. ) ;
#10755 = EDGE_CURVE ( 'NONE', #7825, #28628, #26228, .T. ) ;
#10756 = AXIS2_PLACEMENT_3D ( 'NONE', #23392, #28032, #28541 ) ;
#10757 = AXIS2_PLACEMENT_3D ( 'NONE', #26192, #49641, #33005 ) ;
#10758 = ORIENTED_EDGE ( 'NONE', *, *, #9276, .F. ) ;
#10759 = VERTEX_POINT ( 'NONE', #46324 ) ;
#10760 = DIRECTION ( 'NONE',  ( 0.1785568947986370669, 0.000000000000000000, -0.9839295885986296675 ) ) ;
#10761 = VECTOR ( 'NONE', #50545, 39.37007874015748143 ) ;
#10762 = DIRECTION ( 'NONE',  ( -0.000000000000000000, -1.000000000000000000, -0.000000000000000000 ) ) ;
#10763 = CARTESIAN_POINT ( 'NONE',  ( -0.07591351300297333182, 3.267716535433071279, 0.4724409448818869817 ) ) ;
#10764 = EDGE_CURVE ( 'NONE', #1038, #4027, #31118, .T. ) ;
#10765 = LINE ( 'NONE', #38148, #18204 ) ;
#10767 = DIRECTION ( 'NONE',  ( -0.01601477604151182663, 0.9998717552508123996, -0.000000000000000000 ) ) ;
#10766 = B_SPLINE_CURVE_WITH_KNOTS ( 'NONE', 3,
 ( #4412, #20149, #8027, #7775 ),
 .UNSPECIFIED., .F., .F.,
 ( 4, 4 ),
 ( 1.206284417596563428E-05, 0.002512066550552098567 ),
 .UNSPECIFIED. ) ;
#10768 = CARTESIAN_POINT ( 'NONE',  ( -0.2178414669075503241, 0.5249316475426863970, -1.871410041343207542 ) ) ;
#10769 = VERTEX_POINT ( 'NONE', #18982 ) ;
#10770 = LINE ( 'NONE', #22898, #4384 ) ;
#10771 = CARTESIAN_POINT ( 'NONE',  ( -0.3857230305054721864, 0.000000000000000000, 1.849896105471422025 ) ) ;
#10772 = EDGE_CURVE ( 'NONE', #23541, #35962, #11495, .T. ) ;
#10773 = DIRECTION ( 'NONE',  ( 1.000000000000000000, 0.000000000000000000, 0.000000000000000000 ) ) ;
#10774 = FACE_OUTER_BOUND ( 'NONE', #26658, .T. ) ;
#10775 = ORIENTED_EDGE ( 'NONE', *, *, #48564, .F. ) ;
#10776 = CARTESIAN_POINT ( 'NONE',  ( -2.808237744966007643, 5.905511811023623991, 0.9124517550441288982 ) ) ;
#10777 = CARTESIAN_POINT ( 'NONE',  ( 1.836694934015037806, 1.638894784719147513, 1.401770057403159520 ) ) ;
#10778 = ORIENTED_EDGE ( 'NONE', *, *, #46603, .F. ) ;
#10779 = CARTESIAN_POINT ( 'NONE',  ( -0.8182917201112823724, 3.267716535433071279, 1.419509857074484278E-16 ) ) ;
#10780 = CARTESIAN_POINT ( 'NONE',  ( -2.165354330708661568, 1.673228346456695492, -4.271103535670736336E-20 ) ) ;
#10781 = VERTEX_POINT ( 'NONE', #38860 ) ;
#10782 = CARTESIAN_POINT ( 'NONE',  ( -0.8942052331142552601, 3.267716535433071279, 3.102397620449223960E-16 ) ) ;
#10783 = ORIENTED_EDGE ( 'NONE', *, *, #21437, .T. ) ;
#10784 = CARTESIAN_POINT ( 'NONE',  ( 0.1155636338427008941, -0.5222242541845523167, 0.000000000000000000 ) ) ;
#10785 = DIRECTION ( 'NONE',  ( 0.000000000000000000, 0.000000000000000000, -1.000000000000000000 ) ) ;
#10786 = CONICAL_SURFACE ( 'NONE', #43755, 2.493791675044291445, 0.4363323129985800519 ) ;
#10787 = DIRECTION ( 'NONE',  ( -1.000000000000000000, -0.000000000000000000, -0.000000000000000000 ) ) ;
#10788 = VECTOR ( 'NONE', #8324, 39.37007874015748143 ) ;
#10789 = CARTESIAN_POINT ( 'NONE',  ( -2.043170538425928662, 3.267716535433071279, -0.5118110236220464460 ) ) ;
#10790 = DIRECTION ( 'NONE',  ( -0.000000000000000000, 1.000000000000000000, -0.000000000000000000 ) ) ;
#10791 = ORIENTED_EDGE ( 'NONE', *, *, #24619, .F. ) ;
#10792 = CARTESIAN_POINT ( 'NONE',  ( -1.536664496436148184E-16, 0.000000000000000000, -1.141732283464564013 ) ) ;
#10793 = VERTEX_POINT ( 'NONE', #49925 ) ;
#10794 = ORIENTED_EDGE ( 'NONE', *, *, #5203, .F. ) ;
#10795 = CARTESIAN_POINT ( 'NONE',  ( 0.000000000000000000, 3.267716535433071279, -2.165354330708661568 ) ) ;
#10796 = VERTEX_POINT ( 'NONE', #34738 ) ;
#10797 = CARTESIAN_POINT ( 'NONE',  ( 1.363819533518803695, 0.000000000000000000, 1.732283464566921172 ) ) ;
#10798 = VECTOR ( 'NONE', #25988, 39.37007874015748143 ) ;
#10799 = CARTESIAN_POINT ( 'NONE',  ( 0.2727639067037602172, 0.000000000000000000, -1.732283464566922726 ) ) ;
#10800 = VERTEX_POINT ( 'NONE', #18738 ) ;
#10801 = CARTESIAN_POINT ( 'NONE',  ( 0.000000000000000000, 3.267716535433071279, 0.5905511811023582691 ) ) ;
#10802 = LINE ( 'NONE', #21415, #17501 ) ;
#10803 = EDGE_CURVE ( 'NONE', #41904, #30696, #3493, .T. ) ;
#10804 = FACE_OUTER_BOUND ( 'NONE', #16122, .T. ) ;
#10805 = ORIENTED_EDGE ( 'NONE', *, *, #8710, .T. ) ;
#10807 = EDGE_LOOP ( 'NONE', ( #43918, #25663, #4143, #14508 ) ) ;
#10806 = EDGE_CURVE ( 'NONE', #19754, #40954, #41979, .T. ) ;
#10808 = CARTESIAN_POINT ( 'NONE',  ( 0.002207914879453961535, -5.712274067634378313E-18, 0.04916304461325374242 ) ) ;
#10809 = FACE_BOUND ( 'NONE', #26272, .T. ) ;
#10810 = EDGE_LOOP ( 'NONE', ( #37929, #43182, #32461, #10918 ) ) ;
#10811 = EDGE_CURVE ( 'NONE', #38065, #38012, #38116, .T. ) ;
#10812 = LINE ( 'NONE', #35071, #22080 ) ;
#10813 = EDGE_CURVE ( 'NONE', #39458, #48829, #14451, .T. ) ;
#10815 = ORIENTED_EDGE ( 'NONE', *, *, #7786, .T. ) ;
#10814 = EDGE_CURVE ( 'NONE', #23656, #44436, #2734, .T. ) ;
#10816 = ORIENTED_EDGE ( 'NONE', *, *, #18813, .T. ) ;
#10817 = CARTESIAN_POINT ( 'NONE',  ( 0.000000000000000000, 1.574803149606302854, 0.000000000000000000 ) ) ;
#10818 = DIRECTION ( 'NONE',  ( -1.000000000000000000, 0.000000000000000000, 0.000000000000000000 ) ) ;
#10819 = ORIENTED_EDGE ( 'NONE', *, *, #17277, .T. ) ;
#10820 = VECTOR ( 'NONE', #47411, 39.37007874015748143 ) ;
#10821 = ORIENTED_EDGE ( 'NONE', *, *, #14765, .T. ) ;
#10822 = DIRECTION ( 'NONE',  ( 0.000000000000000000, 0.000000000000000000, -1.000000000000000000 ) ) ;
#10823 = AXIS2_PLACEMENT_3D ( 'NONE', #17708, #21581, #37591 ) ;
#10824 = DIRECTION ( 'NONE',  ( 1.000000000000000000, 0.000000000000000000, 0.000000000000000000 ) ) ;
#10825 = CIRCLE ( 'NONE', #90, 2.165354330708661568 ) ;
#10826 = EDGE_CURVE ( 'NONE', #33365, #15732, #50922, .T. ) ;
#10827 = B_SPLINE_CURVE_WITH_KNOTS ( 'NONE', 3,
 ( #10392, #26138, #6526, #50087 ),
 .UNSPECIFIED., .F., .F.,
 ( 4, 4 ),
 ( 2.003042141634280194E-07, 0.01590458885791005625 ),
 .UNSPECIFIED. ) ;
#10828 = B_SPLINE_CURVE_WITH_KNOTS ( 'NONE', 3,
 ( #32539, #17295, #48230, #5152 ),
 .UNSPECIFIED., .F., .F.,
 ( 4, 4 ),
 ( 0.1211873102087489551, 0.1625992483279400103 ),
 .UNSPECIFIED. ) ;
#10829 = DIRECTION ( 'NONE',  ( 1.000000000000000000, -0.000000000000000000, 0.000000000000000000 ) ) ;
#10830 = ORIENTED_EDGE ( 'NONE', *, *, #50156, .F. ) ;
#10831 = VERTEX_POINT ( 'NONE', #6862 ) ;
#10832 = CARTESIAN_POINT ( 'NONE',  ( -2.695799277629577162, 1.677241212940233872, -1.205759334241492509 ) ) ;
#10833 = LINE ( 'NONE', #6208, #23796 ) ;
#10834 = DIRECTION ( 'NONE',  ( -0.01601477604151182663, 0.9998717552508123996, -0.000000000000000000 ) ) ;
#10835 = ADVANCED_FACE ( 'NONE', ( #7118 ), #26780, .T. ) ;
#10836 = VECTOR ( 'NONE', #32278, 39.37007874015748143 ) ;
#10837 = LINE ( 'NONE', #26333, #9472 ) ;
#10838 = CARTESIAN_POINT ( 'NONE',  ( -1.014069264286641570, 0.5905511811023621549, 1.062992125984251635 ) ) ;
#10839 = VECTOR ( 'NONE', #26769, 39.37007874015748143 ) ;
#10840 = PLANE ( 'NONE',  #11159 ) ;
#10841 = EDGE_CURVE ( 'NONE', #31518, #41767, #18485, .T. ) ;
#10842 = PLANE ( 'NONE',  #44030 ) ;
#10843 = ORIENTED_EDGE ( 'NONE', *, *, #18207, .F. ) ;
#10844 = CARTESIAN_POINT ( 'NONE',  ( 1.636583440222563857, 3.346456692913386100, 1.574803149606291974 ) ) ;
#10845 = LINE ( 'NONE', #10600, #19473 ) ;
#10846 = VERTEX_POINT ( 'NONE', #38362 ) ;
#10847 = EDGE_CURVE ( 'NONE', #26492, #50693, #26726, .T. ) ;
#10848 = VERTEX_POINT ( 'NONE', #43989 ) ;
#10849 = DIRECTION ( 'NONE',  ( -1.000000000000000000, 0.000000000000000000, 1.734723475976806848E-16 ) ) ;
#10850 = CARTESIAN_POINT ( 'NONE',  ( -1.195183497228115035E-16, 3.267716535433071279, -1.574803149606293529 ) ) ;
#10851 = ORIENTED_EDGE ( 'NONE', *, *, #20545, .T. ) ;
#10852 = VERTEX_POINT ( 'NONE', #11996 ) ;
#10853 = LINE ( 'NONE', #42600, #33659 ) ;
#10854 = ORIENTED_EDGE ( 'NONE', *, *, #27350, .T. ) ;
#10855 = AXIS2_PLACEMENT_3D ( 'NONE', #38536, #50099, #42389 ) ;
#10856 = CARTESIAN_POINT ( 'NONE',  ( -1.985260859929297572, 0.000000000000000000, 0.6299212598425164567 ) ) ;
#10857 = DIRECTION ( 'NONE',  ( -1.000000000000000000, 0.000000000000000000, -0.000000000000000000 ) ) ;
#10858 = VECTOR ( 'NONE', #48869, 39.37007874015748143 ) ;
#10859 = VERTEX_POINT ( 'NONE', #32396 ) ;
#10860 = AXIS2_PLACEMENT_3D ( 'NONE', #8641, #1148, #24133 ) ;
#10861 = DIRECTION ( 'NONE',  ( 1.000000000000000000, -0.000000000000000000, 0.000000000000000000 ) ) ;
#10862 = ORIENTED_EDGE ( 'NONE', *, *, #44365, .T. ) ;
#10863 = ORIENTED_EDGE ( 'NONE', *, *, #29515, .T. ) ;
#10864 = CARTESIAN_POINT ( 'NONE',  ( -1.571896207478202800, 0.0009392905874082641340, 0.7899878318620054962 ) ) ;
#10865 = CARTESIAN_POINT ( 'NONE',  ( 1.266373210783726444, 1.640528807385599697, -2.667458607414338712 ) ) ;
#10867 = DIRECTION ( 'NONE',  ( -0.000000000000000000, 1.000000000000000000, -0.000000000000000000 ) ) ;
#10866 = CIRCLE ( 'NONE', #19909, 2.106299212598425008 ) ;
#10868 = CARTESIAN_POINT ( 'NONE',  ( 1.091055626815043311, 3.346456692913386100, 1.692913385826762873 ) ) ;
#10869 = EDGE_CURVE ( 'NONE', #11499, #12204, #24643, .T. ) ;
#10870 = VECTOR ( 'NONE', #32643, 39.37007874015748143 ) ;
#10871 = ORIENTED_EDGE ( 'NONE', *, *, #23687, .F. ) ;
#10872 = CARTESIAN_POINT ( 'NONE',  ( 0.3847164039870727414, 0.5249316475426861750, 1.844349136158301983 ) ) ;
#10873 = DIRECTION ( 'NONE',  ( 1.734723475976806848E-16, 0.000000000000000000, 1.000000000000000000 ) ) ;
#10874 = ADVANCED_FACE ( 'NONE', ( #24383 ), #27479, .F. ) ;
#10875 = CARTESIAN_POINT ( 'NONE',  ( -1.743516651958532115, 0.0004834999639498430428, -4.958524412099369637E-19 ) ) ;
#10876 = ADVANCED_FACE ( 'NONE', ( #28242 ), #43728, .F. ) ;
#10877 = VERTEX_POINT ( 'NONE', #36519 ) ;
#10878 = DIRECTION ( 'NONE',  ( 0.000000000000000000, -1.000000000000000000, 0.000000000000000000 ) ) ;
#10879 = VERTEX_POINT ( 'NONE', #39364 ) ;
#10880 = ORIENTED_EDGE ( 'NONE', *, *, #7042, .F. ) ;
#10881 = DIRECTION ( 'NONE',  ( 0.000000000000000000, 0.000000000000000000, 1.000000000000000000 ) ) ;
#10882 = DIRECTION ( 'NONE',  ( -3.986037398843765983E-20, -1.000000000000000000, -1.160734090543304660E-16 ) ) ;
#10883 = B_SPLINE_CURVE_WITH_KNOTS ( 'NONE', 3,
 ( #43867, #46950, #27613, #32022 ),
 .UNSPECIFIED., .F., .F.,
 ( 4, 4 ),
 ( 2.767205211280488720E-07, 0.002500421812205707271 ),
 .UNSPECIFIED. ) ;
#10884 = DIRECTION ( 'NONE',  ( -0.000000000000000000, 1.000000000000000000, -0.000000000000000000 ) ) ;
#10885 = DIRECTION ( 'NONE',  ( 0.01601477604151182663, -0.9998717552508123996, 0.000000000000000000 ) ) ;
#10886 = LINE ( 'NONE', #43379, #47743 ) ;
#10887 = ORIENTED_EDGE ( 'NONE', *, *, #41135, .T. ) ;
#10888 = VERTEX_POINT ( 'NONE', #44250 ) ;
#10889 = FACE_OUTER_BOUND ( 'NONE', #40006, .T. ) ;
#10890 = CARTESIAN_POINT ( 'NONE',  ( 2.139229417893225627, 0.000000000000000000, -0.3394403656973398742 ) ) ;
#10891 = ORIENTED_EDGE ( 'NONE', *, *, #22572, .F. ) ;
#10892 = CARTESIAN_POINT ( 'NONE',  ( -1.363819533518803473, 3.267716535433071279, 2.365849761790805980E-16 ) ) ;
#10893 = LINE ( 'NONE', #15276, #36669 ) ;
#10894 = VECTOR ( 'NONE', #28713, 39.37007874015748143 ) ;
#10895 = EDGE_CURVE ( 'NONE', #358, #49472, #43475, .T. ) ;
#10896 = FACE_OUTER_BOUND ( 'NONE', #43016, .T. ) ;
#10897 = CARTESIAN_POINT ( 'NONE',  ( 1.805735793522764476, 1.049866565067838264, 0.9158222789645976691 ) ) ;
#10899 = DIRECTION ( 'NONE',  ( 0.000000000000000000, 0.000000000000000000, -1.000000000000000000 ) ) ;
#10898 = VECTOR ( 'NONE', #6561, 39.37007874015748143 ) ;
#10900 = ORIENTED_EDGE ( 'NONE', *, *, #33293, .F. ) ;
#10901 = CARTESIAN_POINT ( 'NONE',  ( 0.000000000000000000, 3.346456692913386100, -2.165354330708661568 ) ) ;
#10902 = CARTESIAN_POINT ( 'NONE',  ( 1.636583440222563635, 3.267716535433071279, -1.259842519685035800 ) ) ;
#10903 = VECTOR ( 'NONE', #47088, 39.37007874015748143 ) ;
#10904 = B_SPLINE_CURVE_WITH_KNOTS ( 'NONE', 3,
 ( #41968, #10728, #6607, #45057 ),
 .UNSPECIFIED., .F., .F.,
 ( 4, 4 ),
 ( 0.1211873102087489551, 0.1625992483279400103 ),
 .UNSPECIFIED. ) ;
#10905 = FACE_OUTER_BOUND ( 'NONE', #15161, .T. ) ;
#10906 = EDGE_CURVE ( 'NONE', #19583, #11836, #40139, .T. ) ;
#10907 = ORIENTED_EDGE ( 'NONE', *, *, #22411, .T. ) ;
#10908 = VECTOR ( 'NONE', #8442, 39.37007874015748143 ) ;
#10909 = CARTESIAN_POINT ( 'NONE',  ( -0.1515599155143076138, 1.705474441417569320, -2.232975473887063966 ) ) ;
#10910 = CARTESIAN_POINT ( 'NONE',  ( 2.134533150281098024, 1.745516327274217572, -1.350025615906367715 ) ) ;
#10911 = CARTESIAN_POINT ( 'NONE',  ( 0.000000000000000000, 3.267716535433071279, 0.000000000000000000 ) ) ;
#10913 = EDGE_CURVE ( 'NONE', #47308, #46754, #4001, .T. ) ;
#10912 = ORIENTED_EDGE ( 'NONE', *, *, #11911, .F. ) ;
#10914 = FACE_OUTER_BOUND ( 'NONE', #44334, .T. ) ;
#10915 = EDGE_CURVE ( 'NONE', #8923, #25574, #8124, .T. ) ;
#10916 = ORIENTED_EDGE ( 'NONE', *, *, #10243, .F. ) ;
#10917 = DIRECTION ( 'NONE',  ( -0.000000000000000000, 1.000000000000000000, -0.000000000000000000 ) ) ;
#10918 = ORIENTED_EDGE ( 'NONE', *, *, #45843, .F. ) ;
#10919 = FACE_OUTER_BOUND ( 'NONE', #19552, .T. ) ;
#10920 = ORIENTED_EDGE ( 'NONE', *, *, #47434, .F. ) ;
#10921 = EDGE_CURVE ( 'NONE', #18547, #3514, #29498, .T. ) ;
#10922 = CARTESIAN_POINT ( 'NONE',  ( 0.2156685157584258827, 1.205361022782829114E-17, -2.945280361644574185 ) ) ;
#10923 = CYLINDRICAL_SURFACE ( 'NONE', #46940, 2.165354330708661568 ) ;
#10924 = CARTESIAN_POINT ( 'NONE',  ( -1.363819533518803473, 3.346456692913386100, -1.929133858267710000 ) ) ;
#10925 = VERTEX_POINT ( 'NONE', #47321 ) ;
#10926 = ORIENTED_EDGE ( 'NONE', *, *, #18769, .F. ) ;
#10927 = VERTEX_POINT ( 'NONE', #39620 ) ;
#10928 = LINE ( 'NONE', #22547, #14186 ) ;
#10929 = CARTESIAN_POINT ( 'NONE',  ( 1.551823387806912313, 1.049866565877818125, 1.300483131990376018 ) ) ;
#10930 = EDGE_LOOP ( 'NONE', ( #47146, #17646, #2488, #23129 ) ) ;
#10931 = CARTESIAN_POINT ( 'NONE',  ( 0.8182917201112819283, 3.267716535433071279, -0.9842519685039348154 ) ) ;
#10932 = DIRECTION ( 'NONE',  ( -3.469446951953613696E-16, 0.000000000000000000, -1.000000000000000000 ) ) ;
#10933 = FACE_OUTER_BOUND ( 'NONE', #36742, .T. ) ;
#10934 = EDGE_CURVE ( 'NONE', #13877, #47112, #32657, .T. ) ;
#10935 = EDGE_LOOP ( 'NONE', ( #23057, #36298, #2737, #45953 ) ) ;
#10936 = CIRCLE ( 'NONE', #44710, 2.165354330708661568 ) ;
#10937 = ORIENTED_EDGE ( 'NONE', *, *, #32651, .T. ) ;
#10938 = DIRECTION ( 'NONE',  ( 0.9362348706397368714, 1.288287287306305283E-16, 0.3513748240813434620 ) ) ;
#10939 = LINE ( 'NONE', #6571, #15902 ) ;
#10940 = PLANE ( 'NONE',  #16498 ) ;
#10941 = ADVANCED_FACE ( 'NONE', ( #43222 ), #7868, .F. ) ;
#10942 = EDGE_LOOP ( 'NONE', ( #10232, #34254, #50292, #48643 ) ) ;
#10943 = DIRECTION ( 'NONE',  ( -3.469446951953613696E-16, 0.000000000000000000, -1.000000000000000000 ) ) ;
#10944 = VECTOR ( 'NONE', #37110, 39.37007874015748143 ) ;
#10945 = CARTESIAN_POINT ( 'NONE',  ( -1.062992125984251413, 0.4724409448818890911, -1.181102362204724754 ) ) ;
#10946 = VERTEX_POINT ( 'NONE', #12770 ) ;
#10947 = DIRECTION ( 'NONE',  ( -1.000000000000000000, 0.000000000000000000, -0.000000000000000000 ) ) ;
#10948 = EDGE_LOOP ( 'NONE', ( #40425, #44746, #21812, #18456 ) ) ;
#10949 = AXIS2_PLACEMENT_3D ( 'NONE', #48218, #8758, #32008 ) ;
#10950 = EDGE_LOOP ( 'NONE', ( #26174, #5853, #27893, #13086 ) ) ;
#10951 = DIRECTION ( 'NONE',  ( 1.734723475976806848E-16, -0.000000000000000000, 1.000000000000000000 ) ) ;
#10952 = LINE ( 'NONE', #31334, #30840 ) ;
#10953 = AXIS2_PLACEMENT_3D ( 'NONE', #34650, #46483, #10136 ) ;
#10954 = VECTOR ( 'NONE', #22212, 39.37007874015748143 ) ;
#10955 = DIRECTION ( 'NONE',  ( -3.469446951953613696E-16, 0.000000000000000000, -1.000000000000000000 ) ) ;
#10956 = CARTESIAN_POINT ( 'NONE',  ( -0.2156685157583833057, 1.520013147563287648, -2.945280361644576850 ) ) ;
#10957 = CARTESIAN_POINT ( 'NONE',  ( -1.833791099076585995, 6.692913385826772199, -1.151507526013721527 ) ) ;
#10958 = ORIENTED_EDGE ( 'NONE', *, *, #1216, .F. ) ;
#10959 = EDGE_LOOP ( 'NONE', ( #30806, #26355, #4035, #11657 ) ) ;
#10960 = CARTESIAN_POINT ( 'NONE',  ( 1.014069264286642014, 0.000000000000000000, 1.062992125984251635 ) ) ;
#10961 = CARTESIAN_POINT ( 'NONE',  ( -2.161044708975090156, 0.000000000000000000, 0.1463148319730351032 ) ) ;
#10962 = EDGE_CURVE ( 'NONE', #24780, #46834, #9480, .T. ) ;
#10963 = DIRECTION ( 'NONE',  ( 0.000000000000000000, 0.000000000000000000, 1.000000000000000000 ) ) ;
#10964 = CARTESIAN_POINT ( 'NONE',  ( 0.2727639067037604947, 0.000000000000000000, 0.7874015748031454320 ) ) ;
#10965 = DIRECTION ( 'NONE',  ( 0.000000000000000000, 0.000000000000000000, -1.000000000000000000 ) ) ;
#10966 = ORIENTED_EDGE ( 'NONE', *, *, #35654, .F. ) ;
#10967 = CARTESIAN_POINT ( 'NONE',  ( -0.2727639067037602172, 3.267716535433071279, 1.417322834645662777 ) ) ;
#10968 = CARTESIAN_POINT ( 'NONE',  ( 0.000000000000000000, 3.267716535433071279, 0.9448818897637749625 ) ) ;
#10969 = ADVANCED_FACE ( 'NONE', ( #114 ), #35745, .F. ) ;
#10970 = ORIENTED_EDGE ( 'NONE', *, *, #10327, .F. ) ;
#10971 = DIRECTION ( 'NONE',  ( 1.000000000000000000, 0.000000000000000000, -3.469446951953613696E-16 ) ) ;
#10972 = ADVANCED_FACE ( 'NONE', ( #39876 ), #376, .F. ) ;
#10973 = DIRECTION ( 'NONE',  ( -1.000000000000000000, -0.000000000000000000, -0.000000000000000000 ) ) ;
#10974 = CARTESIAN_POINT ( 'NONE',  ( -1.610230546471095314, 0.000000000000000000, -0.7060526055843052706 ) ) ;
#10975 = EDGE_CURVE ( 'NONE', #19878, #24653, #49207, .T. ) ;
#10976 = LINE ( 'NONE', #7108, #33382 ) ;
#10977 = DIRECTION ( 'NONE',  ( -0.9998717552508122886, -0.01601477604151180928, 0.000000000000000000 ) ) ;
#10978 = ADVANCED_FACE ( 'NONE', ( #12251 ), #1397, .F. ) ;
#10979 = LINE ( 'NONE', #18478, #468 ) ;
#10980 = AXIS2_PLACEMENT_3D ( 'NONE', #6051, #21297, #48617 ) ;
#10981 = ORIENTED_EDGE ( 'NONE', *, *, #40061, .F. ) ;
#10982 = CARTESIAN_POINT ( 'NONE',  ( 2.182111253630085290, 0.000000000000000000, -0.3149606299212596716 ) ) ;
#10983 = ORIENTED_EDGE ( 'NONE', *, *, #19813, .T. ) ;
#10984 = FACE_BOUND ( 'NONE', #22744, .T. ) ;
#10985 = AXIS2_PLACEMENT_3D ( 'NONE', #16492, #28608, #2774 ) ;
#10986 = CARTESIAN_POINT ( 'NONE',  ( 0.08139965876239094178, 1.610780518492231694, 0.000000000000000000 ) ) ;
#10987 = FACE_OUTER_BOUND ( 'NONE', #40011, .T. ) ;
#10988 = EDGE_CURVE ( 'NONE', #7160, #47130, #37290, .T. ) ;
#10989 = B_SPLINE_CURVE_WITH_KNOTS ( 'NONE', 3,
 ( #13878, #10003, #25744, #41492 ),
 .UNSPECIFIED., .F., .F.,
 ( 4, 4 ),
 ( 0.0007795210587999083351, 0.003279804236056507553 ),
 .UNSPECIFIED. ) ;
#10990 = ORIENTED_EDGE ( 'NONE', *, *, #30882, .F. ) ;
#10991 = ORIENTED_EDGE ( 'NONE', *, *, #5994, .F. ) ;
#10992 = CARTESIAN_POINT ( 'NONE',  ( 1.833791099076603537, 1.574803149606302854, -1.151507526013694216 ) ) ;
#10993 = AXIS2_PLACEMENT_3D ( 'NONE', #43774, #8679, #47363 ) ;
#10994 = CARTESIAN_POINT ( 'NONE',  ( -1.327305354309126884, 0.5249316497054298258, -1.337120393289511266 ) ) ;
#10995 = CARTESIAN_POINT ( 'NONE',  ( 1.833433833923351353, 0.000000000000000000, 0.9448818897637746295 ) ) ;
#10996 = FACE_OUTER_BOUND ( 'NONE', #33314, .T. ) ;
#10997 = EDGE_CURVE ( 'NONE', #19533, #32006, #18166, .T. ) ;
#10998 = PLANE ( 'NONE',  #49132 ) ;
#10999 = DIRECTION ( 'NONE',  ( -0.01601477604151182663, 0.9998717552508123996, -0.000000000000000000 ) ) ;
#11000 = EDGE_CURVE ( 'NONE', #36209, #34423, #2443, .T. ) ;
#11001 = ORIENTED_EDGE ( 'NONE', *, *, #13430, .T. ) ;
#11002 = LINE ( 'NONE', #26739, #26270 ) ;
#11003 = CARTESIAN_POINT ( 'NONE',  ( -1.330126866422489007, 1.653789137470381254, -1.747037097613915568 ) ) ;
#11004 = EDGE_CURVE ( 'NONE', #47658, #15712, #33424, .T. ) ;
#11005 = CARTESIAN_POINT ( 'NONE',  ( -2.032045338671488288, 3.267716535433071279, 0.7480314960629874665 ) ) ;
#11006 = ORIENTED_EDGE ( 'NONE', *, *, #4353, .T. ) ;
#11007 = EDGE_CURVE ( 'NONE', #16948, #46637, #33677, .T. ) ;
#11008 = LINE ( 'NONE', #22128, #961 ) ;
#11009 = ORIENTED_EDGE ( 'NONE', *, *, #668, .T. ) ;
#11010 = ORIENTED_EDGE ( 'NONE', *, *, #1071, .F. ) ;
#11011 = ORIENTED_EDGE ( 'NONE', *, *, #27773, .T. ) ;
#11012 = ORIENTED_EDGE ( 'NONE', *, *, #39961, .T. ) ;
#11013 = CARTESIAN_POINT ( 'NONE',  ( -0.3486774197067340486, 0.000000000000000000, -1.456692913385822630 ) ) ;
#11014 = VECTOR ( 'NONE', #34124, 39.37007874015748143 ) ;
#11015 = CIRCLE ( 'NONE', #30807, 2.244934639244525076 ) ;
#11016 = DIRECTION ( 'NONE',  ( -3.469446951953613696E-16, 0.000000000000000000, -1.000000000000000000 ) ) ;
#11017 = DIRECTION ( 'NONE',  ( 0.6427876096865403621, 0.7660444431189770143, 1.115133390745971592E-16 ) ) ;
#11018 = VECTOR ( 'NONE', #6955, 39.37007874015748143 ) ;
#11019 = AXIS2_PLACEMENT_3D ( 'NONE', #46363, #35984, #50458 ) ;
#11020 = CARTESIAN_POINT ( 'NONE',  ( 2.298329729280814249, 1.755067388827460384, 1.853838447111812338 ) ) ;
#11021 = CARTESIAN_POINT ( 'NONE',  ( 0.08119777152254364916, 1.623385212329073957, 0.000000000000000000 ) ) ;
#11022 = PLANE ( 'NONE',  #46769 ) ;
#11023 = AXIS2_PLACEMENT_3D ( 'NONE', #47812, #16370, #28224 ) ;
#11024 = ORIENTED_EDGE ( 'NONE', *, *, #22284, .F. ) ;
#11025 = B_SPLINE_CURVE_WITH_KNOTS ( 'NONE', 3,
 ( #34279, #22398, #6902, #18776 ),
 .UNSPECIFIED., .F., .F.,
 ( 4, 4 ),
 ( 0.001628790289768138272, 0.004128914707219031623 ),
 .UNSPECIFIED. ) ;
#11026 = PLANE ( 'NONE',  #49678 ) ;
#11027 = DIRECTION ( 'NONE',  ( 1.734723475976806848E-16, 0.000000000000000000, 1.000000000000000000 ) ) ;
#11028 = DIRECTION ( 'NONE',  ( 1.734723475976806848E-16, -0.000000000000000000, 1.000000000000000000 ) ) ;
#11029 = DIRECTION ( 'NONE',  ( -1.000000000000000000, 0.000000000000000000, 0.000000000000000000 ) ) ;
#11030 = ORIENTED_EDGE ( 'NONE', *, *, #48812, .F. ) ;
#11031 = DIRECTION ( 'NONE',  ( -0.3090169943749447312, 1.104046895826785399E-16, -0.9510565162951544194 ) ) ;
#11032 = ADVANCED_FACE ( 'NONE', ( #2163 ), #17661, .F. ) ;
#11033 = CARTESIAN_POINT ( 'NONE',  ( 0.1968503937007873017, 3.267716535433071279, -1.259842519685035134 ) ) ;
#11034 = ORIENTED_EDGE ( 'NONE', *, *, #5615, .T. ) ;
#11035 = CARTESIAN_POINT ( 'NONE',  ( -1.743145509346916588, 0.000000000000000000, 0.000000000000000000 ) ) ;
#11036 = DIRECTION ( 'NONE',  ( -0.000000000000000000, 0.000000000000000000, 1.000000000000000000 ) ) ;
#11037 = EDGE_CURVE ( 'NONE', #23942, #3832, #40802, .T. ) ;
#11038 = ADVANCED_FACE ( 'NONE', ( #29270 ), #41405, .F. ) ;
#11039 = DIRECTION ( 'NONE',  ( -3.986037398843765983E-20, -1.000000000000000000, -1.160734090543304660E-16 ) ) ;
#11040 = VERTEX_POINT ( 'NONE', #6295 ) ;
#11041 = DIRECTION ( 'NONE',  ( -3.986037398843765983E-20, -1.000000000000000000, -1.160734090543304660E-16 ) ) ;
#11042 = EDGE_CURVE ( 'NONE', #28182, #8765, #33165, .T. ) ;
#11043 = CARTESIAN_POINT ( 'NONE',  ( -0.5455278134075214336, 0.000000000000000000, -1.141732283464563791 ) ) ;
#11044 = DIRECTION ( 'NONE',  ( -0.7530714660036099684, -1.160734090543304907E-16, -0.6579387259397138088 ) ) ;
#11045 = LINE ( 'NONE', #43027, #48969 ) ;
#11046 = DIRECTION ( 'NONE',  ( -3.469446951953613696E-16, 0.000000000000000000, -1.000000000000000000 ) ) ;
#11047 = EDGE_LOOP ( 'NONE', ( #27910, #47211, #46524, #34077, #46468 ) ) ;
#11048 = DIRECTION ( 'NONE',  ( -3.469446951953613696E-16, 0.000000000000000000, -1.000000000000000000 ) ) ;
#11049 = AXIS2_PLACEMENT_3D ( 'NONE', #14317, #1682, #13818 ) ;
#11050 = ORIENTED_EDGE ( 'NONE', *, *, #44486, .T. ) ;
#11051 = ORIENTED_EDGE ( 'NONE', *, *, #4678, .T. ) ;
#11052 = VECTOR ( 'NONE', #12295, 39.37007874015748143 ) ;
#11053 = CARTESIAN_POINT ( 'NONE',  ( 0.000000000000000000, 1.574803149606302854, 0.000000000000000000 ) ) ;
#11054 = ORIENTED_EDGE ( 'NONE', *, *, #33732, .F. ) ;
#11055 = LINE ( 'NONE', #6427, #16401 ) ;
#11056 = AXIS2_PLACEMENT_3D ( 'NONE', #18283, #13909, #10032 ) ;
#11057 = ADVANCED_FACE ( 'NONE', ( #37033 ), #49362, .F. ) ;
#11058 = DIRECTION ( 'NONE',  ( -1.858431260983764056E-16, 0.7660444431189770143, 0.6427876096865403621 ) ) ;
#11059 = ORIENTED_EDGE ( 'NONE', *, *, #12544, .T. ) ;
#11060 = VECTOR ( 'NONE', #33686, 39.37007874015748143 ) ;
#11061 = AXIS2_PLACEMENT_3D ( 'NONE', #9834, #44420, #17075 ) ;
#11062 = CARTESIAN_POINT ( 'NONE',  ( -2.134236802639925212, 0.000000000000000000, -2.040539317874611847 ) ) ;
#11063 = EDGE_CURVE ( 'NONE', #44945, #34145, #14037, .T. ) ;
#11064 = DIRECTION ( 'NONE',  ( -1.000000000000000000, 0.000000000000000000, -0.000000000000000000 ) ) ;
#11065 = AXIS2_PLACEMENT_3D ( 'NONE', #22721, #26087, #22224 ) ;
#11066 = LINE ( 'NONE', #26800, #29659 ) ;
#11067 = VERTEX_POINT ( 'NONE', #29785 ) ;
#11068 = ORIENTED_EDGE ( 'NONE', *, *, #29464, .T. ) ;
#11069 = EDGE_CURVE ( 'NONE', #20587, #25223, #37546, .T. ) ;
#11070 = CARTESIAN_POINT ( 'NONE',  ( 0.4696143004045476022, 0.000000000000000000, -1.929133858267710000 ) ) ;
#11071 = FACE_BOUND ( 'NONE', #42919, .T. ) ;
#11072 = EDGE_LOOP ( 'NONE', ( #41210, #21157, #27378, #36076 ) ) ;
#11073 = DIRECTION ( 'NONE',  ( 1.734723475976806848E-16, -0.000000000000000000, 1.000000000000000000 ) ) ;
#11074 = VERTEX_POINT ( 'NONE', #45501 ) ;
#11075 = ORIENTED_EDGE ( 'NONE', *, *, #41032, .T. ) ;
#11076 = DIRECTION ( 'NONE',  ( -3.469446951953613696E-16, 0.000000000000000000, -1.000000000000000000 ) ) ;
#11077 = CARTESIAN_POINT ( 'NONE',  ( 1.236813753895252166, 1.738537790538875027, -2.681693691597563767 ) ) ;
#11078 = ORIENTED_EDGE ( 'NONE', *, *, #46758, .T. ) ;
#11079 = CARTESIAN_POINT ( 'NONE',  ( -2.951990591674674924, 1.574803149606301744, 0.000000000000000000 ) ) ;
#11080 = VERTEX_POINT ( 'NONE', #25912 ) ;
#11081 = CARTESIAN_POINT ( 'NONE',  ( 0.1526763070133267952, 1.611922144458495687, -2.245379599360889600 ) ) ;
#11082 = CARTESIAN_POINT ( 'NONE',  ( 4.097771990496411591E-16, 3.346456692913386100, 2.106299212598425008 ) ) ;
#11083 = CARTESIAN_POINT ( 'NONE',  ( -0.3486774197067339376, 3.267716535433071279, -1.259842519685035134 ) ) ;
#11084 = ORIENTED_EDGE ( 'NONE', *, *, #49811, .F. ) ;
#11085 = ORIENTED_EDGE ( 'NONE', *, *, #11162, .F. ) ;
#11086 = CONICAL_SURFACE ( 'NONE', #8610, 3.483074324928249421, 1.244861948955335196 ) ;
#11087 = DIRECTION ( 'NONE',  ( 1.734723475976806848E-16, 0.000000000000000000, 1.000000000000000000 ) ) ;
#11088 = CARTESIAN_POINT ( 'NONE',  ( 0.000000000000000000, 3.267716535433071279, 0.6299212598425164567 ) ) ;
#11089 = AXIS2_PLACEMENT_3D ( 'NONE', #8097, #4991, #32371 ) ;
#11090 = DIRECTION ( 'NONE',  ( -0.7227948638273878901, 8.024280841161103757E-17, -0.6910626489868684219 ) ) ;
#11091 = CONICAL_SURFACE ( 'NONE', #39948, 2.244934639244524632, 1.554780866114618743 ) ;
#11092 = DIRECTION ( 'NONE',  ( 0.000000000000000000, 0.000000000000000000, 1.000000000000000000 ) ) ;
#11093 = VECTOR ( 'NONE', #30669, 39.37007874015748143 ) ;
#11094 = PLANE ( 'NONE',  #14109 ) ;
#11095 = AXIS2_PLACEMENT_3D ( 'NONE', #50224, #26773, #31417 ) ;
#11096 = PLANE ( 'NONE',  #32587 ) ;
#11097 = DIRECTION ( 'NONE',  ( -1.000000000000000000, -0.000000000000000000, -0.000000000000000000 ) ) ;
#11098 = EDGE_CURVE ( 'NONE', #5773, #45425, #9402, .T. ) ;
#11099 = VECTOR ( 'NONE', #7515, 39.37007874015748143 ) ;
#11100 = ORIENTED_EDGE ( 'NONE', *, *, #42723, .T. ) ;
#11101 = CARTESIAN_POINT ( 'NONE',  ( 0.000000000000000000, 6.692913385826772199, 0.000000000000000000 ) ) ;
#11102 = CARTESIAN_POINT ( 'NONE',  ( 1.645338673473796254, 0.05427277550655955352, -1.027111169014480296 ) ) ;
#11103 = EDGE_CURVE ( 'NONE', #25844, #47691, #3757, .T. ) ;
#11104 = VERTEX_POINT ( 'NONE', #9659 ) ;
#11105 = EDGE_CURVE ( 'NONE', #3117, #24926, #43645, .T. ) ;
#11106 = ORIENTED_EDGE ( 'NONE', *, *, #22656, .F. ) ;
#11107 = CARTESIAN_POINT ( 'NONE',  ( 1.062992125984252079, 0.5905511811023621549, -1.181102362204724754 ) ) ;
#11108 = CARTESIAN_POINT ( 'NONE',  ( -1.930190994932096782, 0.000000000000000000, -0.9827944786818723077 ) ) ;
#11109 = ORIENTED_EDGE ( 'NONE', *, *, #4967, .F. ) ;
#11110 = EDGE_CURVE ( 'NONE', #8562, #47259, #40642, .T. ) ;
#11111 = ORIENTED_EDGE ( 'NONE', *, *, #43850, .T. ) ;
#11112 = DIRECTION ( 'NONE',  ( 0.6579387259397027066, 0.000000000000000000, 0.7530714660036195163 ) ) ;
#11113 = VERTEX_POINT ( 'NONE', #41912 ) ;
#11114 = CARTESIAN_POINT ( 'NONE',  ( 0.000000000000000000, 3.267716535433071279, -1.102362204724405714 ) ) ;
#11115 = DIRECTION ( 'NONE',  ( -0.000000000000000000, 1.000000000000000000, -0.000000000000000000 ) ) ;
#11116 = EDGE_CURVE ( 'NONE', #15892, #12933, #34177, .T. ) ;
#11117 = VERTEX_POINT ( 'NONE', #3429 ) ;
#11118 = DIRECTION ( 'NONE',  ( -0.9998717552508121775, -0.01601477604151182663, 0.000000000000000000 ) ) ;
#11119 = AXIS2_PLACEMENT_3D ( 'NONE', #39019, #33898, #38027 ) ;
#11120 = B_SPLINE_CURVE_WITH_KNOTS ( 'NONE', 3,
 ( #42635, #46485, #38280, #30524 ),
 .UNSPECIFIED., .F., .F.,
 ( 4, 4 ),
 ( 2.051261343427981145E-07, 0.002500229005657641102 ),
 .UNSPECIFIED. ) ;
#11121 = ORIENTED_EDGE ( 'NONE', *, *, #29369, .F. ) ;
#11122 = EDGE_LOOP ( 'NONE', ( #32238, #41392, #14188, #31374 ) ) ;
#11123 = EDGE_CURVE ( 'NONE', #33470, #41056, #23292, .T. ) ;
#11124 = AXIS2_PLACEMENT_3D ( 'NONE', #17886, #49332, #49577 ) ;
#11125 = LINE ( 'NONE', #6747, #21891 ) ;
#11126 = CYLINDRICAL_SURFACE ( 'NONE', #17438, 2.164630168518208109 ) ;
#11127 = CARTESIAN_POINT ( 'NONE',  ( 1.636583440222563857, 0.000000000000000000, 0.9448818897637746295 ) ) ;
#11128 = VECTOR ( 'NONE', #46572, 39.37007874015748143 ) ;
#11129 = VERTEX_POINT ( 'NONE', #46511 ) ;
#11130 = CARTESIAN_POINT ( 'NONE',  ( 0.2727639067037604392, 0.000000000000000000, 0.2755905511810994302 ) ) ;
#11131 = DIRECTION ( 'NONE',  ( -1.000000000000000000, -0.000000000000000000, -0.000000000000000000 ) ) ;
#11132 = ORIENTED_EDGE ( 'NONE', *, *, #7138, .T. ) ;
#11133 = CARTESIAN_POINT ( 'NONE',  ( -0.8238130908517355966, 1.694707076513333410, 2.054984861273213337 ) ) ;
#11134 = CIRCLE ( 'NONE', #35863, 1.743387098533651480 ) ;
#11135 = ORIENTED_EDGE ( 'NONE', *, *, #26951, .T. ) ;
#11136 = VERTEX_POINT ( 'NONE', #6796 ) ;
#11137 = PRODUCT_CONTEXT ( 'NONE', #1884, 'mechanical' ) ;
#11138 = EDGE_CURVE ( 'NONE', #40564, #45493, #6553, .T. ) ;
#11139 = CARTESIAN_POINT ( 'NONE',  ( -0.07591351300297284610, 3.346456692913386100, 0.5905511811023582691 ) ) ;
#11140 = DIRECTION ( 'NONE',  ( -0.9195277725514544587, 0.000000000000000000, 0.3930250316539147803 ) ) ;
#11141 = DIRECTION ( 'NONE',  ( -3.469446951953613696E-16, 0.000000000000000000, -1.000000000000000000 ) ) ;
#11142 = DIRECTION ( 'NONE',  ( -0.000000000000000000, 1.000000000000000000, -0.000000000000000000 ) ) ;
#11143 = VERTEX_POINT ( 'NONE', #34426 ) ;
#11144 = ORIENTED_EDGE ( 'NONE', *, *, #38901, .F. ) ;
#11145 = PRESENTATION_STYLE_ASSIGNMENT (( #2640 ) ) ;
#11146 = LINE ( 'NONE', #15525, #12750 ) ;
#11147 = VERTEX_POINT ( 'NONE', #26909 ) ;
#11148 = LINE ( 'NONE', #10892, #15874 ) ;
#11149 = LINE ( 'NONE', #19138, #28390 ) ;
#11150 = PLANE ( 'NONE',  #15148 ) ;
#11151 = PLANE ( 'NONE',  #3821 ) ;
#11152 = PLANE ( 'NONE',  #38598 ) ;
#11153 = ORIENTED_EDGE ( 'NONE', *, *, #9491, .T. ) ;
#11154 = AXIS2_PLACEMENT_3D ( 'NONE', #23719, #4110, #39727 ) ;
#11155 = CARTESIAN_POINT ( 'NONE',  ( -1.166969139818015533, 3.346456692913386100, 0.1574803149606287811 ) ) ;
#11156 = LINE ( 'NONE', #7033, #9577 ) ;
#11157 = EDGE_CURVE ( 'NONE', #26859, #50859, #31048, .T. ) ;
#11158 = VECTOR ( 'NONE', #21846, 39.37007874015748143 ) ;
#11159 = AXIS2_PLACEMENT_3D ( 'NONE', #15221, #46426, #38473 ) ;
#11160 = CARTESIAN_POINT ( 'NONE',  ( 0.000000000000000000, 3.267716535433071279, 0.000000000000000000 ) ) ;
#11161 = VECTOR ( 'NONE', #46198, 39.37007874015748143 ) ;
#11162 = EDGE_CURVE ( 'NONE', #44618, #30787, #49609, .T. ) ;
#11163 = ORIENTED_EDGE ( 'NONE', *, *, #46725, .T. ) ;
#11164 = DIRECTION ( 'NONE',  ( 1.000000000000000000, 0.000000000000000000, -3.469446951953613696E-16 ) ) ;
#11165 = DIRECTION ( 'NONE',  ( -0.01601477604151182663, 0.9998717552508123996, -0.000000000000000000 ) ) ;
#11166 = CARTESIAN_POINT ( 'NONE',  ( 1.883550378546973381, 6.692913385826772199, -1.069467267250421294 ) ) ;
#11167 = EDGE_CURVE ( 'NONE', #15209, #39907, #47922, .T. ) ;
#11168 = VERTEX_POINT ( 'NONE', #22297 ) ;
#11169 = ADVANCED_FACE ( 'NONE', ( #38308 ), #11428, .F. ) ;
#11170 = LINE ( 'NONE', #34417, #31659 ) ;
#11171 = VECTOR ( 'NONE', #1976, 39.37007874015748143 ) ;
#11172 = ORIENTED_EDGE ( 'NONE', *, *, #34666, .F. ) ;
#11173 = DIRECTION ( 'NONE',  ( 0.000000000000000000, 0.000000000000000000, -1.000000000000000000 ) ) ;
#11174 = ORIENTED_EDGE ( 'NONE', *, *, #2821, .F. ) ;
#11175 = CARTESIAN_POINT ( 'NONE',  ( 0.08139965876239094178, 1.610780518492231694, 0.000000000000000000 ) ) ;
#11176 = ORIENTED_EDGE ( 'NONE', *, *, #36049, .F. ) ;
#11177 = CARTESIAN_POINT ( 'NONE',  ( 0.000000000000000000, 3.267716535433071279, -2.401574803149598480 ) ) ;
#11178 = DIRECTION ( 'NONE',  ( 0.000000000000000000, 1.160734090543304660E-16, -1.000000000000000000 ) ) ;
#11179 = LINE ( 'NONE', #42662, #23535 ) ;
#11180 = EDGE_CURVE ( 'NONE', #1205, #34792, #15049, .T. ) ;
#11181 = ORIENTED_EDGE ( 'NONE', *, *, #42500, .F. ) ;
#11182 = ORIENTED_EDGE ( 'NONE', *, *, #4694, .F. ) ;
#11183 = ORIENTED_EDGE ( 'NONE', *, *, #49346, .T. ) ;
#11184 = CARTESIAN_POINT ( 'NONE',  ( -1.195183497228115035E-16, 3.346456692913386100, -0.3149606299212591165 ) ) ;
#11185 = CARTESIAN_POINT ( 'NONE',  ( -0.5455278134075214336, 3.267716535433071279, -8.878505979408855953E-16 ) ) ;
#11186 = VERTEX_POINT ( 'NONE', #39042 ) ;
#11187 = EDGE_CURVE ( 'NONE', #1604, #24291, #7053, .T. ) ;
#11188 = CARTESIAN_POINT ( 'NONE',  ( 1.646369848953919135, 1.642880493769403927, -2.182308221245992552 ) ) ;
#11189 = DIRECTION ( 'NONE',  ( 0.000000000000000000, 0.000000000000000000, -1.000000000000000000 ) ) ;
#11190 = CARTESIAN_POINT ( 'NONE',  ( 2.823445274216730638, 1.450545469922353892, 0.8656477926280681245 ) ) ;
#11191 = EDGE_LOOP ( 'NONE', ( #36354, #13336, #49954, #46163 ) ) ;
#11192 = VERTEX_POINT ( 'NONE', #10417 ) ;
#11193 = FACE_OUTER_BOUND ( 'NONE', #44151, .T. ) ;
#11194 = FACE_OUTER_BOUND ( 'NONE', #29082, .T. ) ;
#11195 = ADVANCED_FACE ( 'NONE', ( #30293 ), #26167, .T. ) ;
#11196 = DIRECTION ( 'NONE',  ( -0.000000000000000000, 0.000000000000000000, 1.000000000000000000 ) ) ;
#11197 = ORIENTED_EDGE ( 'NONE', *, *, #17268, .T. ) ;
#11198 = LINE ( 'NONE', #15320, #22441 ) ;
#11199 = PLANE ( 'NONE',  #25246 ) ;
#11200 =( GEOMETRIC_REPRESENTATION_CONTEXT ( 3 ) GLOBAL_UNCERTAINTY_ASSIGNED_CONTEXT ( ( #28278 ) ) GLOBAL_UNIT_ASSIGNED_CONTEXT ( ( #8809, #43397, #8554 ) ) REPRESENTATION_CONTEXT ( 'NONE', 'WORKASPACE' ) );
#11201 = ORIENTED_EDGE ( 'NONE', *, *, #13743, .T. ) ;
#11202 = VECTOR ( 'NONE', #40962, 39.37007874015748143 ) ;
#11203 = FACE_OUTER_BOUND ( 'NONE', #11598, .T. ) ;
#11204 = ORIENTED_EDGE ( 'NONE', *, *, #21271, .F. ) ;
#11205 = ORIENTED_EDGE ( 'NONE', *, *, #4067, .T. ) ;
#11206 = FACE_OUTER_BOUND ( 'NONE', #3641, .T. ) ;
#11207 = DIRECTION ( 'NONE',  ( -0.000000000000000000, 1.000000000000000000, -0.000000000000000000 ) ) ;
#11208 = EDGE_CURVE ( 'NONE', #21585, #30221, #10674, .T. ) ;
#11209 = AXIS2_PLACEMENT_3D ( 'NONE', #15627, #15122, #30874 ) ;
#11210 = LINE ( 'NONE', #23835, #34638 ) ;
#11211 = AXIS2_PLACEMENT_3D ( 'NONE', #25109, #5484, #1352 ) ;
#11212 = FACE_OUTER_BOUND ( 'NONE', #46895, .T. ) ;
#11213 = CARTESIAN_POINT ( 'NONE',  ( 0.2727639067037604947, 3.346456692913386100, 0.1574803149606283648 ) ) ;
#11214 = EDGE_LOOP ( 'NONE', ( #1037, #21857 ) ) ;
#11215 = AXIS2_PLACEMENT_3D ( 'NONE', #43413, #35683, #8058 ) ;
#11216 = EDGE_CURVE ( 'NONE', #26667, #33610, #24552, .T. ) ;
#11217 = ORIENTED_EDGE ( 'NONE', *, *, #47904, .F. ) ;
#11218 = CARTESIAN_POINT ( 'NONE',  ( 1.909347346926324462, 3.346456692913386100, -0.7874015748031473194 ) ) ;
#11219 = CARTESIAN_POINT ( 'NONE',  ( -1.091055626815042645, 3.346456692913386100, -1.889763779527552146 ) ) ;
#11220 = EDGE_CURVE ( 'NONE', #12966, #41924, #45786, .T. ) ;
#11221 = DIRECTION ( 'NONE',  ( -1.000000000000000000, 0.000000000000000000, 1.734723475976806848E-16 ) ) ;
#11222 = CARTESIAN_POINT ( 'NONE',  ( 2.062746868503864572, 1.708132218730083807, 1.054125835973626968 ) ) ;
#11223 = ORIENTED_EDGE ( 'NONE', *, *, #25766, .F. ) ;
#11224 = CARTESIAN_POINT ( 'NONE',  ( -0.04921259842519708910, 1.714701585914776283, 2.715578020061004683 ) ) ;
#11225 = DIRECTION ( 'NONE',  ( -1.000000000000000000, 0.000000000000000000, 0.000000000000000000 ) ) ;
#11226 = ADVANCED_FACE ( 'NONE', ( #50114 ), #14801, .T. ) ;
#11227 = ORIENTED_EDGE ( 'NONE', *, *, #9824, .T. ) ;
#11228 = DIRECTION ( 'NONE',  ( -3.469446951953613696E-16, 0.000000000000000000, -1.000000000000000000 ) ) ;
#11229 = LINE ( 'NONE', #38851, #16238 ) ;
#11230 = DIRECTION ( 'NONE',  ( -9.701723960855857903E-17, 1.000000000000000000, 8.476140964546263859E-17 ) ) ;
#11231 = AXIS2_PLACEMENT_3D ( 'NONE', #19959, #16876, #92 ) ;
#11232 = CARTESIAN_POINT ( 'NONE',  ( 0.000000000000000000, 3.267716535433071279, 0.000000000000000000 ) ) ;
#11233 = CARTESIAN_POINT ( 'NONE',  ( -1.166969139818015755, 0.000000000000000000, 1.220472440944875281 ) ) ;
#11234 = ADVANCED_FACE ( 'NONE', ( #46262 ), #39200, .T. ) ;
#11235 = DIRECTION ( 'NONE',  ( -0.01601477604151182663, 0.9998717552508123996, -0.000000000000000000 ) ) ;
#11236 = AXIS2_PLACEMENT_3D ( 'NONE', #9837, #10090, #17833 ) ;
#11237 = VECTOR ( 'NONE', #28538, 39.37007874015748143 ) ;
#11238 = ORIENTED_EDGE ( 'NONE', *, *, #12375, .T. ) ;
#11239 = LINE ( 'NONE', #38110, #37054 ) ;
#11240 = ORIENTED_EDGE ( 'NONE', *, *, #7026, .T. ) ;
#11241 = CARTESIAN_POINT ( 'NONE',  ( 0.000000000000000000, 3.267716535433071279, 0.6299212598425164567 ) ) ;
#11242 = CIRCLE ( 'NONE', #14561, 2.874015748031496731 ) ;
#11243 = CARTESIAN_POINT ( 'NONE',  ( -0.6214413264104945434, 3.346456692913386100, -0.4724409448818886470 ) ) ;
#11244 = PLANE ( 'NONE',  #49853 ) ;
#11245 = VECTOR ( 'NONE', #32260, 39.37007874015748143 ) ;
#11246 = AXIS2_PLACEMENT_3D ( 'NONE', #35505, #39120, #50679 ) ;
#11247 = ORIENTED_EDGE ( 'NONE', *, *, #4359, .T. ) ;
#11248 = ORIENTED_EDGE ( 'NONE', *, *, #44134, .T. ) ;
#11249 = DIRECTION ( 'NONE',  ( 0.000000000000000000, 1.160734090543304660E-16, -1.000000000000000000 ) ) ;
#11250 = CARTESIAN_POINT ( 'NONE',  ( -1.891607981616729495, 1.579179190298960256, 1.073803248357834139 ) ) ;
#11251 = LINE ( 'NONE', #26979, #24215 ) ;
#11252 = CARTESIAN_POINT ( 'NONE',  ( -1.985260859929297572, 0.000000000000000000, -6.146657985744592735E-16 ) ) ;
#11253 = PLANE ( 'NONE',  #2191 ) ;
#11254 = CARTESIAN_POINT ( 'NONE',  ( 1.905671854841463952, 1.748959039950288341, 2.256015092822681645 ) ) ;
#11255 = ORIENTED_EDGE ( 'NONE', *, *, #4916, .T. ) ;
#11256 = CARTESIAN_POINT ( 'NONE',  ( 2.951990591674676256, 1.447429260878886348, -0.08331184815398369470 ) ) ;
#11257 = CARTESIAN_POINT ( 'NONE',  ( 1.091055626815042645, 3.267716535433071279, -0.6299212598425181220 ) ) ;
#11258 = EDGE_CURVE ( 'NONE', #12736, #25699, #10386, .T. ) ;
#11259 = CARTESIAN_POINT ( 'NONE',  ( 0.7855418668307558860, 0.000000000000000000, -2.846347029613733870 ) ) ;
#11260 = ORIENTED_EDGE ( 'NONE', *, *, #21209, .F. ) ;
#11261 = CARTESIAN_POINT ( 'NONE',  ( 2.161044708975088380, 1.205361022782829114E-17, 0.1463148319730657732 ) ) ;
#11262 = ORIENTED_EDGE ( 'NONE', *, *, #23929, .T. ) ;
#11263 = ORIENTED_EDGE ( 'NONE', *, *, #44365, .F. ) ;
#11264 = EDGE_CURVE ( 'NONE', #4750, #27191, #22702, .T. ) ;
#11265 = EDGE_CURVE ( 'NONE', #9222, #39032, #8056, .T. ) ;
#11266 = ADVANCED_FACE ( 'NONE', ( #12185 ), #20441, .T. ) ;
#11267 = AXIS2_PLACEMENT_3D ( 'NONE', #2018, #30148, #38163 ) ;
#11268 = ORIENTED_EDGE ( 'NONE', *, *, #2847, .F. ) ;
#11269 = ORIENTED_EDGE ( 'NONE', *, *, #47305, .F. ) ;
#11270 = CARTESIAN_POINT ( 'NONE',  ( -1.439733046521776139, 3.346456692913386100, 0.9448818897637749625 ) ) ;
#11271 = VECTOR ( 'NONE', #50273, 39.37007874015748143 ) ;
#11272 = VECTOR ( 'NONE', #43699, 39.37007874015748143 ) ;
#11273 = DIRECTION ( 'NONE',  ( -3.469446951953613696E-16, 0.000000000000000000, -1.000000000000000000 ) ) ;
#11274 = CARTESIAN_POINT ( 'NONE',  ( -2.012389709434417195, 1.049866565877818347, 0.2229346561180729214 ) ) ;
#11275 = CARTESIAN_POINT ( 'NONE',  ( 0.4517796511351843680, 1.715138028758778521, 2.213898087213642007 ) ) ;
#11276 = AXIS2_PLACEMENT_3D ( 'NONE', #12027, #39905, #4541 ) ;
#11277 = CARTESIAN_POINT ( 'NONE',  ( 2.320271282243135502, 1.712256942838378260, -0.1534657056239357720 ) ) ;
#11278 = EDGE_CURVE ( 'NONE', #16625, #9331, #4805, .T. ) ;
#11279 = VECTOR ( 'NONE', #45512, 39.37007874015748143 ) ;
#11280 = FACE_OUTER_BOUND ( 'NONE', #14703, .T. ) ;
#11281 = CARTESIAN_POINT ( 'NONE',  ( 1.474379988472116487, 1.633091647787944911, 1.762361831087230213 ) ) ;
#11282 = VERTEX_POINT ( 'NONE', #47510 ) ;
#11283 = DIRECTION ( 'NONE',  ( 1.000000000000000000, -0.000000000000000000, 0.000000000000000000 ) ) ;
#11284 = CARTESIAN_POINT ( 'NONE',  ( 0.2727639067037604947, 3.346456692913386100, 0.7874015748031454320 ) ) ;
#11285 = CARTESIAN_POINT ( 'NONE',  ( 0.2727639067037602172, 0.000000000000000000, -1.732283464566922726 ) ) ;
#11286 = CARTESIAN_POINT ( 'NONE',  ( -1.091055626815042201, 0.000000000000000000, 1.574803149606291974 ) ) ;
#11287 = EDGE_CURVE ( 'NONE', #4959, #39171, #36200, .T. ) ;
#11288 = ORIENTED_EDGE ( 'NONE', *, *, #38947, .T. ) ;
#11289 = CARTESIAN_POINT ( 'NONE',  ( -0.1071992566810134884, 0.000000000000000000, -1.740088185897663342 ) ) ;
#11290 = DIRECTION ( 'NONE',  ( 1.734723475976806848E-16, -0.000000000000000000, 1.000000000000000000 ) ) ;
#11291 = EDGE_LOOP ( 'NONE', ( #40473, #28471, #16129, #3350 ) ) ;
#11292 = DIRECTION ( 'NONE',  ( -0.01601477604151182663, 0.9998717552508123996, -0.000000000000000000 ) ) ;
#11293 = EDGE_CURVE ( 'NONE', #4560, #48286, #39297, .T. ) ;
#11294 = CARTESIAN_POINT ( 'NONE',  ( -0.8783128861146038968, 0.01385187720497466773, 1.565997986929510644 ) ) ;
#11295 = EDGE_CURVE ( 'NONE', #31964, #44522, #20807, .T. ) ;
#11296 = DIRECTION ( 'NONE',  ( -3.986037398843765983E-20, -1.000000000000000000, -1.160734090543304660E-16 ) ) ;
#11297 = ORIENTED_EDGE ( 'NONE', *, *, #7121, .T. ) ;
#11298 = DIRECTION ( 'NONE',  ( -0.000000000000000000, 1.000000000000000000, -0.000000000000000000 ) ) ;
#11299 = DIRECTION ( 'NONE',  ( 0.3090169943749582204, 1.288287287306305283E-16, -0.9510565162951500895 ) ) ;
#11300 = DIRECTION ( 'NONE',  ( -3.469446951953613696E-16, 0.000000000000000000, -1.000000000000000000 ) ) ;
#11301 = CARTESIAN_POINT ( 'NONE',  ( 0.000000000000000000, 3.267716535433071279, 1.220472440944875281 ) ) ;
#11302 = CARTESIAN_POINT ( 'NONE',  ( 1.779568955232893268, 1.574803149606302854, -1.233650562797287797 ) ) ;
#11303 = EDGE_LOOP ( 'NONE', ( #25179, #26304, #26689, #48105 ) ) ;
#11304 = VECTOR ( 'NONE', #42954, 39.37007874015748143 ) ;
#11305 = AXIS2_PLACEMENT_3D ( 'NONE', #2469, #45543, #6340 ) ;
#11306 = ORIENTED_EDGE ( 'NONE', *, *, #564, .T. ) ;
#11307 = EDGE_LOOP ( 'NONE', ( #50327, #49330, #36764, #4828 ) ) ;
#11308 = LINE ( 'NONE', #22676, #8089 ) ;
#11309 = ORIENTED_EDGE ( 'NONE', *, *, #12850, .T. ) ;
#11310 = CYLINDRICAL_SURFACE ( 'NONE', #40320, 2.165354330708661568 ) ;
#11311 = DIRECTION ( 'NONE',  ( 1.734723475976806848E-16, 0.000000000000000000, 1.000000000000000000 ) ) ;
#11312 = ORIENTED_EDGE ( 'NONE', *, *, #33851, .F. ) ;
#11313 = DIRECTION ( 'NONE',  ( -1.000000000000000000, 0.000000000000000000, -0.000000000000000000 ) ) ;
#11314 = ORIENTED_EDGE ( 'NONE', *, *, #7459, .F. ) ;
#11315 = DIRECTION ( 'NONE',  ( -1.000000000000000000, 0.000000000000000000, 0.000000000000000000 ) ) ;
#11316 = ORIENTED_EDGE ( 'NONE', *, *, #43915, .T. ) ;
#11317 = VERTEX_POINT ( 'NONE', #23804 ) ;
#11318 = FACE_OUTER_BOUND ( 'NONE', #24331, .T. ) ;
#11319 = ORIENTED_EDGE ( 'NONE', *, *, #38927, .F. ) ;
#11320 = VECTOR ( 'NONE', #15904, 39.37007874015748143 ) ;
#11321 = DIRECTION ( 'NONE',  ( 1.000000000000000000, 0.000000000000000000, 0.000000000000000000 ) ) ;
#11322 = EDGE_CURVE ( 'NONE', #39188, #65, #19914, .T. ) ;
#11323 = EDGE_CURVE ( 'NONE', #31195, #48901, #35431, .T. ) ;
#11324 = ORIENTED_EDGE ( 'NONE', *, *, #39841, .T. ) ;
#11325 = ORIENTED_EDGE ( 'NONE', *, *, #17846, .F. ) ;
#11326 = LINE ( 'NONE', #46659, #23267 ) ;
#11327 = EDGE_CURVE ( 'NONE', #20851, #48279, #40018, .T. ) ;
#11328 = LINE ( 'NONE', #43310, #8925 ) ;
#11329 = ORIENTED_EDGE ( 'NONE', *, *, #48118, .F. ) ;
#11330 = CARTESIAN_POINT ( 'NONE',  ( -2.454875160333845674, 3.189042514953126961, -0.3543307086614173040 ) ) ;
#11331 = ORIENTED_EDGE ( 'NONE', *, *, #40517, .T. ) ;
#11332 = DIRECTION ( 'NONE',  ( 1.000000000000000000, 0.000000000000000000, 0.000000000000000000 ) ) ;
#11333 = ADVANCED_FACE ( 'NONE', ( #4698 ), #39551, .F. ) ;
#11334 = CARTESIAN_POINT ( 'NONE',  ( -1.091055626815042201, 3.346456692913386100, 0.1181102362204705658 ) ) ;
#11335 = AXIS2_PLACEMENT_3D ( 'NONE', #4970, #1089, #41362 ) ;
#11336 = VECTOR ( 'NONE', #43143, 39.37007874015748143 ) ;
#11337 = CARTESIAN_POINT ( 'NONE',  ( 0.5455278134075211005, 3.267716535433071279, 0.7480314960629872445 ) ) ;
#11338 = VERTEX_POINT ( 'NONE', #44182 ) ;
#11339 = VERTEX_POINT ( 'NONE', #28178 ) ;
#11340 = LINE ( 'NONE', #6961, #1390 ) ;
#11341 = DIRECTION ( 'NONE',  ( -0.000000000000000000, 0.000000000000000000, 1.000000000000000000 ) ) ;
#11342 = PLANE ( 'NONE',  #25836 ) ;
#11343 = ADVANCED_FACE ( 'NONE', ( #47252 ), #46997, .F. ) ;
#11344 = PLANE ( 'NONE',  #5407 ) ;
#11345 = CARTESIAN_POINT ( 'NONE',  ( 1.015142113812069979, 3.346456692913386100, 1.912654141836395372 ) ) ;
#11346 = EDGE_CURVE ( 'NONE', #20275, #45649, #43004, .T. ) ;
#11347 = CARTESIAN_POINT ( 'NONE',  ( -0.2156685157583831947, 1.715903002249486997, -2.945280361644576850 ) ) ;
#11348 = CARTESIAN_POINT ( 'NONE',  ( -0.2727639067037608278, 3.267716535433071279, -1.299212598425193210 ) ) ;
#11349 = EDGE_CURVE ( 'NONE', #41298, #47368, #28474, .T. ) ;
#11350 = ORIENTED_EDGE ( 'NONE', *, *, #13103, .F. ) ;
#11351 = DIRECTION ( 'NONE',  ( 1.000000000000000000, 0.000000000000000000, -3.469446951953613696E-16 ) ) ;
#11352 = EDGE_CURVE ( 'NONE', #6103, #31288, #20176, .T. ) ;
#11353 = AXIS2_PLACEMENT_3D ( 'NONE', #41704, #7850, #18720 ) ;
#11354 = EDGE_CURVE ( 'NONE', #5106, #36537, #31304, .T. ) ;
#11355 = VERTEX_POINT ( 'NONE', #48787 ) ;
#11356 = VERTEX_POINT ( 'NONE', #40835 ) ;
#11357 = LINE ( 'NONE', #12367, #20097 ) ;
#11358 = CARTESIAN_POINT ( 'NONE',  ( -0.2727639067037607723, 3.346456692913386100, -0.1574803149606301411 ) ) ;
#11359 = VERTEX_POINT ( 'NONE', #10102 ) ;
#11360 = FACE_OUTER_BOUND ( 'NONE', #50627, .T. ) ;
#11361 = ORIENTED_EDGE ( 'NONE', *, *, #51018, .T. ) ;
#11362 = DIRECTION ( 'NONE',  ( -0.000000000000000000, 0.000000000000000000, 1.000000000000000000 ) ) ;
#11363 = EDGE_LOOP ( 'NONE', ( #49647, #42908, #8834, #46019 ) ) ;
#11364 = CARTESIAN_POINT ( 'NONE',  ( 0.5455278134075211005, 3.346456692913386100, 0.7480314960629872445 ) ) ;
#11365 = CARTESIAN_POINT ( 'NONE',  ( -1.294674717613570003, 1.049866565067837820, 1.556672598277949016 ) ) ;
#11366 = VECTOR ( 'NONE', #8888, 39.37007874015748143 ) ;
#11367 = VECTOR ( 'NONE', #49476, 39.37007874015748143 ) ;
#11368 = VERTEX_POINT ( 'NONE', #25335 ) ;
#11369 = DIRECTION ( 'NONE',  ( -0.000000000000000000, 0.000000000000000000, 1.000000000000000000 ) ) ;
#11370 = ORIENTED_EDGE ( 'NONE', *, *, #31210, .T. ) ;
#11371 = ORIENTED_EDGE ( 'NONE', *, *, #36883, .F. ) ;
#11372 = CARTESIAN_POINT ( 'NONE',  ( -2.014567149787738654, 1.675634971041569443, -0.8075478974698888646 ) ) ;
#11373 = LINE ( 'NONE', #42106, #7513 ) ;
#11374 = DIRECTION ( 'NONE',  ( -1.000000000000000000, -0.000000000000000000, -0.000000000000000000 ) ) ;
#11375 = VECTOR ( 'NONE', #38254, 39.37007874015748854 ) ;
#11376 = EDGE_LOOP ( 'NONE', ( #2157, #46433, #1483, #11963 ) ) ;
#11377 = VECTOR ( 'NONE', #30227, 39.37007874015748143 ) ;
#11378 = CARTESIAN_POINT ( 'NONE',  ( 3.519654186525858491E-16, 3.346456692913386100, 2.874015748031496731 ) ) ;
#11379 = CARTESIAN_POINT ( 'NONE',  ( 0.000000000000000000, 1.574803149606302854, 0.000000000000000000 ) ) ;
#11380 = ORIENTED_EDGE ( 'NONE', *, *, #31958, .T. ) ;
#11381 = VECTOR ( 'NONE', #7455, 39.37007874015748143 ) ;
#11382 = LINE ( 'NONE', #26619, #41382 ) ;
#11383 = EDGE_CURVE ( 'NONE', #44874, #31800, #44683, .T. ) ;
#11384 = EDGE_CURVE ( 'NONE', #23553, #25851, #9335, .T. ) ;
#11385 = ORIENTED_EDGE ( 'NONE', *, *, #3228, .F. ) ;
#11386 = ORIENTED_EDGE ( 'NONE', *, *, #21888, .F. ) ;
#11387 = CARTESIAN_POINT ( 'NONE',  ( 0.000000000000000000, 0.000000000000000000, 0.000000000000000000 ) ) ;
#11388 = AXIS2_PLACEMENT_3D ( 'NONE', #34904, #26642, #43134 ) ;
#11389 = ADVANCED_FACE ( 'NONE', ( #21214 ), #37223, .F. ) ;
#11390 = VERTEX_POINT ( 'NONE', #36970 ) ;
#11391 = CARTESIAN_POINT ( 'NONE',  ( -1.905671854841497481, 1.591126119768930147, 2.256015092822653223 ) ) ;
#11392 = LINE ( 'NONE', #42371, #2733 ) ;
#11393 = LINE ( 'NONE', #23508, #50788 ) ;
#11394 = CARTESIAN_POINT ( 'NONE',  ( 1.287906020515830141, 0.000000000000000000, 0.9448818897637746295 ) ) ;
#11395 = VERTEX_POINT ( 'NONE', #17848 ) ;
#11396 = ORIENTED_EDGE ( 'NONE', *, *, #35593, .F. ) ;
#11397 = PRESENTATION_STYLE_ASSIGNMENT (( #3652 ) ) ;
#11398 = CARTESIAN_POINT ( 'NONE',  ( -0.3486774197067334380, 0.000000000000000000, 0.6299212598425164567 ) ) ;
#11399 = ORIENTED_EDGE ( 'NONE', *, *, #45686, .F. ) ;
#11400 = DIRECTION ( 'NONE',  ( 1.000000000000000000, 0.000000000000000000, 0.000000000000000000 ) ) ;
#11401 = FACE_OUTER_BOUND ( 'NONE', #6382, .T. ) ;
#11402 = ADVANCED_FACE ( 'NONE', ( #25589 ), #33356, .F. ) ;
#11403 = CIRCLE ( 'NONE', #40271, 2.165354330708661568 ) ;
#11404 = LINE ( 'NONE', #20154, #28366 ) ;
#11405 = CARTESIAN_POINT ( 'NONE',  ( 0.8182917201112824834, 3.267716535433071279, 1.535433070866133898 ) ) ;
#11406 = FACE_OUTER_BOUND ( 'NONE', #15183, .T. ) ;
#11407 = ORIENTED_EDGE ( 'NONE', *, *, #14933, .T. ) ;
#11408 = LINE ( 'NONE', #34656, #26685 ) ;
#11410 = EDGE_CURVE ( 'NONE', #31480, #17017, #1143, .T. ) ;
#11409 = DIRECTION ( 'NONE',  ( 0.9998717552508121775, 0.01601477604151182663, 0.000000000000000000 ) ) ;
#11411 = B_SPLINE_CURVE_WITH_KNOTS ( 'NONE', 3,
 ( #38777, #10897, #26392, #22520 ),
 .UNSPECIFIED., .F., .F.,
 ( 4, 4 ),
 ( 0.1211775127643062444, 0.1625894504277921315 ),
 .UNSPECIFIED. ) ;
#11412 = EDGE_CURVE ( 'NONE', #50705, #45906, #9851, .T. ) ;
#11413 = AXIS2_PLACEMENT_3D ( 'NONE', #27697, #43441, #8086 ) ;
#11414 = VERTEX_POINT ( 'NONE', #36711 ) ;
#11415 = CLOSED_SHELL ( 'NONE', ( #33734, #15141, #18164, #25221, #43792, #43732, #34483, #26474, #16471, #35080, #38995, #34658, #31981, #43609, #24204, #50596, #45882, #47407, #45310, #25716, #31995, #21348, #22353, #42459, #30358, #22661, #11195, #50949, #2308, #22949, #43727, #39515, #36433, #43257, #46547, #2118, #31283, #49688, #50714, #23133, #9907, #26029, #6676, #50219, #36815, #38656, #50722, #28645, #45212, #8040, #23103, #41165, #18256, #19935, #47099, #23348, #48492, #30634, #2203, #6830, #49073, #4772, #38056, #4289, #15532, #37888, #33915, #33696, #21007, #46837, #38619, #48632, #8817, #24569, #27243, #4021, #26615, #43414, #1560, #35308, #26440, #34040, #44029, #7659, #34252, #2483, #672, #32886, #44561, #13166, #375, #38393, #22532, #48698, #19840, #27455, #50124, #37171, #31612, #23257, #11632, #8491, #43934, #6753, #12089, #8687, #17135, #3338, #297, #50940, #7855, #4222, #12677, #11548, #43409, #11521, #19531, #12579, #36951, #7853, #50690, #31455, #28117, #38644, #48377, #7019, #32496, #748, #32605, #40862, #26793, #30818, #10132, #2035, #12122, #20417, #33661, #1845, #40872, #15687, #48655, #28059, #3830, #10340, #5520, #17231, #40243, #44223, #44123, #26260, #11472, #49064, #11266, #42114, #6332, #19300, #3975, #4566, #31335, #7196, #48527, #14986, #44344, #4008, #47717, #12801, #26577, #15900, #17716, #46103, #11226, #2444, #19877, #17596, #30117, #4810, #42228, #7387, #39993, #37464, #50231, #50023, #36152, #5215, #7246, #41426, #26787, #8238, #41035, #10418, #39901, #4514, #28295, #31426, #22094, #18765, #25977, #7413, #23328, #46559, #19201, #7750, #31637, #14895, #19028, #10360, #26563, #1957, #45819, #33082, #41657, #36766, #7156, #29366, #33085, #23186, #41864, #29144, #47836, #42326, #27946, #11842, #41604, #28331, #37988, #10277, #7341, #7252, #411, #22492, #36238, #15266, #30238, #12670, #24578, #12969, #47170, #15407, #33389, #38175, #25106, #46880, #18504, #32759, #3320, #6700, #49177, #30345, #19468, #31792, #43503, #29483, #31684, #6516, #10721, #46009, #6985, #23199, #16369, #50969, #22527, #16357, #4200, #27605, #32819, #44157, #24978, #19362, #13420, #667, #14757, #22470, #16299, #39191, #9234, #25546, #46106, #15799, #11234, #26953, #42780, #50036, #46944, #1660, #5491, #35828, #35805, #2411, #25566, #2260, #10627, #13809, #7321, #20836, #42084, #13065, #15637, #1428, #19557, #893, #5758, #37305, #923, #36599, #37408, #47081, #31268, #23589, #46640, #19677, #33032, #21636, #37282, #28349, #27049, #23966, #49399, #41766, #16933, #50005, #31686, #34765, #45717, #45750, #31710, #10835, #44510, #29098, #22139, #47175, #45926, #25067, #21254, #50780, #28483, #21207, #25074, #20432, #5577, #3744, #20130, #31979, #43071, #31925, #48373, #37217, #1049, #40381, #41661, #31851, #12995, #18812, #22207, #6546, #13177, #10009, #9012, #28655, #8294, #46579, #24496, #42446, #6715, #44959, #18335, #7250, #9038, #11625, #44089, #2634, #15890, #23391, #32012, #29634, #37749, #19141, #9888, #37527, #6869, #42133, #45708, #14947, #9733, #24102, #16943, #13578, #15704, #42968, #26988, #47400, #16334, #47950, #25060, #19429, #45535, #15403, #35219, #31747, #1493, #27939, #22872, #19184, #48956, #40081, #39835, #3700, #38147, #25577, #16423, #1813, #17187, #44989, #32400, #25517, #46670, #33011, #31973, #21732, #50298, #46411, #10428, #18964, #13107, #9185, #26080, #11741, #35279, #38776, #38624, #32660, #50091, #35368, #50657, #38792, #44953, #26602, #46461, #35400, #23807, #44356, #9196, #34425, #43269, #35261, #46145, #19021, #24153, #45113, #29533, #19785, #48177, #9118, #17182, #39586, #25708, #1181, #34420, #27548, #500, #34580, #2756, #2506, #15423, #15368 ) ) ;
#11417 = CARTESIAN_POINT ( 'NONE',  ( -0.07591351300297284610, 3.267716535433071279, 0.5905511811023582691 ) ) ;
#11416 = AXIS2_PLACEMENT_3D ( 'NONE', #25785, #22176, #46143 ) ;
#11418 = DIRECTION ( 'NONE',  ( 1.734723475976806848E-16, -0.000000000000000000, 1.000000000000000000 ) ) ;
#11419 = DIRECTION ( 'NONE',  ( -0.01601477604151182663, 0.9998717552508123996, -0.000000000000000000 ) ) ;
#11420 = VERTEX_POINT ( 'NONE', #48533 ) ;
#11421 = VECTOR ( 'NONE', #45346, 39.37007874015748143 ) ;
#11422 = ORIENTED_EDGE ( 'NONE', *, *, #5161, .F. ) ;
#11423 = LINE ( 'NONE', #42897, #41096 ) ;
#11424 = VERTEX_POINT ( 'NONE', #49040 ) ;
#11425 = AXIS2_PLACEMENT_3D ( 'NONE', #32715, #26464, #49415 ) ;
#11426 = CARTESIAN_POINT ( 'NONE',  ( 0.1067246931122726866, 0.02962905676920215767, 0.000000000000000000 ) ) ;
#11427 = ORIENTED_EDGE ( 'NONE', *, *, #40616, .F. ) ;
#11428 = PLANE ( 'NONE',  #18581 ) ;
#11430 = VECTOR ( 'NONE', #9760, 39.37007874015748143 ) ;
#11429 = CARTESIAN_POINT ( 'NONE',  ( 1.955075903006588067, 1.470442306530027832, 2.212852075800510576 ) ) ;
#11431 = CARTESIAN_POINT ( 'NONE',  ( -0.07591351300297333182, 3.346456692913386100, -1.102362204724405714 ) ) ;
#11432 = ORIENTED_EDGE ( 'NONE', *, *, #49234, .T. ) ;
#11433 = VERTEX_POINT ( 'NONE', #13216 ) ;
#11434 = ORIENTED_EDGE ( 'NONE', *, *, #50211, .F. ) ;
#11435 = DIRECTION ( 'NONE',  ( 1.000000000000000000, 0.000000000000000000, 0.000000000000000000 ) ) ;
#11436 = DIRECTION ( 'NONE',  ( -0.9998717552508122886, -0.01601477604151185785, 0.000000000000000000 ) ) ;
#11437 = ORIENTED_EDGE ( 'NONE', *, *, #48016, .T. ) ;
#11438 = ORIENTED_EDGE ( 'NONE', *, *, #45234, .F. ) ;
#11439 = CARTESIAN_POINT ( 'NONE',  ( 1.517339494376257703, 1.637296765517717523, -2.004713174013318611 ) ) ;
#11440 = FACE_OUTER_BOUND ( 'NONE', #12657, .T. ) ;
#11441 = DIRECTION ( 'NONE',  ( 1.734723475976806848E-16, 0.000000000000000000, 1.000000000000000000 ) ) ;
#11442 = ORIENTED_EDGE ( 'NONE', *, *, #28707, .F. ) ;
#11443 = ORIENTED_EDGE ( 'NONE', *, *, #14264, .F. ) ;
#11444 = CARTESIAN_POINT ( 'NONE',  ( 0.7423782071083085965, 3.267716535433071279, -1.456692913385822630 ) ) ;
#11445 = DIRECTION ( 'NONE',  ( -3.986037398843765983E-20, -1.000000000000000000, -1.160734090543304660E-16 ) ) ;
#11446 = VECTOR ( 'NONE', #4771, 39.37007874015748854 ) ;
#11447 = LINE ( 'NONE', #27183, #9687 ) ;
#11448 = EDGE_LOOP ( 'NONE', ( #19058, #3748, #12242, #27453 ) ) ;
#11449 = DIRECTION ( 'NONE',  ( -0.000000000000000000, 1.000000000000000000, -0.000000000000000000 ) ) ;
#11450 = LINE ( 'NONE', #43685, #10397 ) ;
#11451 = ORIENTED_EDGE ( 'NONE', *, *, #47463, .F. ) ;
#11452 = EDGE_CURVE ( 'NONE', #795, #2123, #4950, .T. ) ;
#11453 = LINE ( 'NONE', #39325, #6823 ) ;
#11454 = EDGE_LOOP ( 'NONE', ( #29971, #23237, #30711, #22689 ) ) ;
#11455 = EDGE_LOOP ( 'NONE', ( #23404, #30407, #24057, #7077 ) ) ;
#11456 = CARTESIAN_POINT ( 'NONE',  ( 0.000000000000000000, 3.267716535433071279, 1.732283464566920950 ) ) ;
#11457 = LINE ( 'NONE', #30831, #39046 ) ;
#11458 = EDGE_CURVE ( 'NONE', #6407, #22173, #16966, .T. ) ;
#11459 = CIRCLE ( 'NONE', #49337, 2.106299212598425008 ) ;
#11460 = DIRECTION ( 'NONE',  ( -0.9998717552508122886, -0.01601477604151182316, 0.000000000000000000 ) ) ;
#11461 = EDGE_CURVE ( 'NONE', #30195, #27463, #37482, .T. ) ;
#11462 = CARTESIAN_POINT ( 'NONE',  ( 0.7423782071083082634, 0.000000000000000000, -1.771653543307081025 ) ) ;
#11463 = ADVANCED_FACE ( 'NONE', ( #5204 ), #36456, .F. ) ;
#11465 = CARTESIAN_POINT ( 'NONE',  ( 0.8182917201112824834, 0.000000000000000000, 1.417322834645662777 ) ) ;
#11464 = VECTOR ( 'NONE', #26330, 39.37007874015748143 ) ;
#11466 = ORIENTED_EDGE ( 'NONE', *, *, #22284, .T. ) ;
#11467 = EDGE_LOOP ( 'NONE', ( #8833, #14753 ) ) ;
#11468 = CIRCLE ( 'NONE', #40331, 1.850107469027523432 ) ;
#11469 = ORIENTED_EDGE ( 'NONE', *, *, #33103, .F. ) ;
#11470 = CARTESIAN_POINT ( 'NONE',  ( 2.755905511811024056, 4.960629921259846142, 1.023622047244094446 ) ) ;
#11471 = DIRECTION ( 'NONE',  ( 1.000000000000000000, -0.000000000000000000, 0.000000000000000000 ) ) ;
#11472 = ADVANCED_FACE ( 'NONE', ( #13467 ), #29202, .T. ) ;
#11473 = B_SPLINE_CURVE_WITH_KNOTS ( 'NONE', 3,
 ( #6998, #2872, #22746, #15248 ),
 .UNSPECIFIED., .F., .F.,
 ( 4, 4 ),
 ( 2.032912801187147383E-07, 0.002500496937475709964 ),
 .UNSPECIFIED. ) ;
#11474 = CARTESIAN_POINT ( 'NONE',  ( 0.000000000000000000, 3.267716535433071279, -2.047244094488182231 ) ) ;
#11475 = LINE ( 'NONE', #35222, #13022 ) ;
#11476 = ORIENTED_EDGE ( 'NONE', *, *, #24113, .F. ) ;
#11477 = DIRECTION ( 'NONE',  ( -0.000000000000000000, 1.000000000000000000, -0.000000000000000000 ) ) ;
#11478 = ADVANCED_FACE ( 'NONE', ( #13727 ), #25846, .F. ) ;
#11479 = CARTESIAN_POINT ( 'NONE',  ( -1.166969139818016199, 3.267716535433071279, -0.9842519685039344823 ) ) ;
#11480 = ORIENTED_EDGE ( 'NONE', *, *, #43960, .F. ) ;
#11481 = CARTESIAN_POINT ( 'NONE',  ( 1.015142113812069979, 3.346456692913386100, 1.220472440944875281 ) ) ;
#11482 = CARTESIAN_POINT ( 'NONE',  ( 0.000000000000000000, 3.267716535433071279, -0.1574803149606304187 ) ) ;
#11483 = CARTESIAN_POINT ( 'NONE',  ( 0.000000000000000000, 0.07874015748031502893, -0.3937007874015748254 ) ) ;
#11484 = AXIS2_PLACEMENT_3D ( 'NONE', #31826, #7562, #35184 ) ;
#11485 = EDGE_CURVE ( 'NONE', #41810, #15466, #14685, .T. ) ;
#11486 = CARTESIAN_POINT ( 'NONE',  ( 0.000000000000000000, 3.267716535433071279, -2.204724409448811429 ) ) ;
#11487 = PLANE ( 'NONE',  #26671 ) ;
#11488 = CARTESIAN_POINT ( 'NONE',  ( -0.5455278134075208785, 3.346456692913386100, 1.889763779527550369 ) ) ;
#11489 = EDGE_LOOP ( 'NONE', ( #47299, #49264, #21843, #18435 ) ) ;
#11490 = CARTESIAN_POINT ( 'NONE',  ( -1.743268982565497449, 0.0004610889948519912205, -0.02902809809614041725 ) ) ;
#11491 = VERTEX_POINT ( 'NONE', #48280 ) ;
#11492 = DIRECTION ( 'NONE',  ( -0.9989930665413151445, 0.000000000000000000, 0.04486483035050446017 ) ) ;
#11493 = EDGE_CURVE ( 'NONE', #15175, #23260, #2341, .T. ) ;
#11494 = VECTOR ( 'NONE', #26445, 39.37007874015748143 ) ;
#11495 = LINE ( 'NONE', #50420, #50645 ) ;
#11496 = CARTESIAN_POINT ( 'NONE',  ( -1.909347346926324906, 0.000000000000000000, -1.102362204724405492 ) ) ;
#11497 = AXIS2_PLACEMENT_3D ( 'NONE', #26468, #38359, #10481 ) ;
#11498 = VERTEX_POINT ( 'NONE', #40580 ) ;
#11499 = VERTEX_POINT ( 'NONE', #30988 ) ;
#11500 = LINE ( 'NONE', #42972, #19906 ) ;
#11501 = LINE ( 'NONE', #39116, #27092 ) ;
#11502 = CARTESIAN_POINT ( 'NONE',  ( 0.000000000000000000, 3.267716535433071279, -0.8267716535433055070 ) ) ;
#11503 = CARTESIAN_POINT ( 'NONE',  ( 1.771435203777392386, 1.736274727556916808, 1.475617711110977615 ) ) ;
#11504 = VECTOR ( 'NONE', #23873, 39.37007874015748143 ) ;
#11505 = DIRECTION ( 'NONE',  ( -0.01601477604151182663, 0.9998717552508123996, -0.000000000000000000 ) ) ;
#11506 = LINE ( 'NONE', #23367, #6680 ) ;
#11507 = ORIENTED_EDGE ( 'NONE', *, *, #5290, .F. ) ;
#11508 = CARTESIAN_POINT ( 'NONE',  ( -1.363819533518803029, 3.267716535433071279, 0.1574803149606287811 ) ) ;
#11509 = LINE ( 'NONE', #26487, #18348 ) ;
#11510 = LINE ( 'NONE', #15386, #42979 ) ;
#11511 = ORIENTED_EDGE ( 'NONE', *, *, #18126, .F. ) ;
#11512 = CARTESIAN_POINT ( 'NONE',  ( -1.776015597772149013, 0.5249316475426857309, 0.6288076367337267492 ) ) ;
#11513 = EDGE_LOOP ( 'NONE', ( #35371, #36602, #28545, #23968 ) ) ;
#11514 = ORIENTED_EDGE ( 'NONE', *, *, #46224, .F. ) ;
#11515 = CARTESIAN_POINT ( 'NONE',  ( -2.454875160333845674, 3.242921367653845977, -0.03937007874015881204 ) ) ;
#11516 = EDGE_CURVE ( 'NONE', #31565, #28182, #49545, .T. ) ;
#11517 = AXIS2_PLACEMENT_3D ( 'NONE', #40527, #40784, #16781 ) ;
#11518 = VERTEX_POINT ( 'NONE', #18613 ) ;
#11519 = EDGE_LOOP ( 'NONE', ( #39414, #34696, #45526, #22041 ) ) ;
#11520 = CARTESIAN_POINT ( 'NONE',  ( -2.932638728931780125, 5.905511811023623991, 0.3475908556737787314 ) ) ;
#11521 = ADVANCED_FACE ( 'NONE', ( #45691 ), #10357, .T. ) ;
#11522 = ORIENTED_EDGE ( 'NONE', *, *, #6221, .T. ) ;
#11523 = B_SPLINE_CURVE_WITH_KNOTS ( 'NONE', 3,
 ( #49046, #36976, #36462, #48285 ),
 .UNSPECIFIED., .F., .F.,
 ( 4, 4 ),
 ( 0.01141953369039028915, 0.03073634068572588668 ),
 .UNSPECIFIED. ) ;
#11524 = CARTESIAN_POINT ( 'NONE',  ( 0.4696143004045479352, 0.000000000000000000, -1.102362204724405714 ) ) ;
#11525 = CARTESIAN_POINT ( 'NONE',  ( 0.04921259842519669359, 1.621581020286960051, 2.952755905511811108 ) ) ;
#11526 = VECTOR ( 'NONE', #37511, 39.37007874015748143 ) ;
#11527 = CARTESIAN_POINT ( 'NONE',  ( 0.1968503937007878568, 0.000000000000000000, 2.204724409448808764 ) ) ;
#11528 = CARTESIAN_POINT ( 'NONE',  ( 0.4178893628429310447, -0.2057703422145251981, -2.141165755267305126 ) ) ;
#11529 = DIRECTION ( 'NONE',  ( 1.000000000000000000, 0.000000000000000000, -3.469446951953613696E-16 ) ) ;
#11530 = ORIENTED_EDGE ( 'NONE', *, *, #48432, .F. ) ;
#11531 = CARTESIAN_POINT ( 'NONE',  ( -0.3486774197067339376, 3.346456692913386100, -0.9448818897637762948 ) ) ;
#11532 = CARTESIAN_POINT ( 'NONE',  ( 0.4696143004045479352, 3.346456692913386100, -1.417322834645664331 ) ) ;
#11533 = VECTOR ( 'NONE', #40581, 39.37007874015748143 ) ;
#11534 = CARTESIAN_POINT ( 'NONE',  ( 0.6150616064519864867, 0.03777100275179151589, 1.778883059170359493 ) ) ;
#11535 = CARTESIAN_POINT ( 'NONE',  ( -1.062992125984252079, 0.5905511811023621549, -1.014069264286642236 ) ) ;
#11536 = EDGE_LOOP ( 'NONE', ( #5022, #49162, #46160, #48607 ) ) ;
#11537 = DIRECTION ( 'NONE',  ( 0.9749279121818259508, 0.000000000000000000, -0.2225209339563041788 ) ) ;
#11538 = CARTESIAN_POINT ( 'NONE',  ( 1.363819533518803251, 3.346456692913386100, 0.1574803149606283648 ) ) ;
#11539 = VERTEX_POINT ( 'NONE', #34615 ) ;
#11540 = LINE ( 'NONE', #43529, #20492 ) ;
#11541 = EDGE_CURVE ( 'NONE', #36491, #42385, #22236, .T. ) ;
#11542 = CARTESIAN_POINT ( 'NONE',  ( -1.405664884363581502, 1.586962458333645021, 1.683711065981816857 ) ) ;
#11543 = CARTESIAN_POINT ( 'NONE',  ( -1.387241876633674265, 6.692913385826772199, 1.662624236931676602 ) ) ;
#11544 = EDGE_LOOP ( 'NONE', ( #4723, #10092, #49757, #20224 ) ) ;
#11545 = LINE ( 'NONE', #27281, #35522 ) ;
#11546 = EDGE_CURVE ( 'NONE', #4710, #43170, #38740, .T. ) ;
#11547 = CARTESIAN_POINT ( 'NONE',  ( 0.000000000000000000, 3.267716535433071279, 1.259842519685033357 ) ) ;
#11548 = ADVANCED_FACE ( 'NONE', ( #45945 ), #34864, .T. ) ;
#11549 = FACE_OUTER_BOUND ( 'NONE', #17347, .T. ) ;
#11550 = CARTESIAN_POINT ( 'NONE',  ( -1.363819533518803473, 3.346456692913386100, -0.9842519685039344823 ) ) ;
#11551 = ORIENTED_EDGE ( 'NONE', *, *, #27710, .F. ) ;
#11552 = EDGE_CURVE ( 'NONE', #21109, #15197, #26353, .T. ) ;
#11553 = VERTEX_POINT ( 'NONE', #50296 ) ;
#11554 = ORIENTED_EDGE ( 'NONE', *, *, #43894, .T. ) ;
#11555 = CARTESIAN_POINT ( 'NONE',  ( 0.7423782071083084855, 3.267716535433071279, -2.575641807848709208E-16 ) ) ;
#11556 = ORIENTED_EDGE ( 'NONE', *, *, #24712, .F. ) ;
#11557 = EDGE_CURVE ( 'NONE', #9319, #2383, #14989, .T. ) ;
#11558 = LINE ( 'NONE', #47134, #45224 ) ;
#11559 = CARTESIAN_POINT ( 'NONE',  ( -2.793030215715272213, 1.573188339825353665, 0.9592557174602283077 ) ) ;
#11560 = ORIENTED_EDGE ( 'NONE', *, *, #40974, .T. ) ;
#11561 = EDGE_CURVE ( 'NONE', #22568, #47433, #30231, .T. ) ;
#11562 = VECTOR ( 'NONE', #27263, 39.37007874015748143 ) ;
#11563 = CARTESIAN_POINT ( 'NONE',  ( -3.927031490892378253E-16, 0.000000000000000000, -2.204724409448811429 ) ) ;
#11564 = VECTOR ( 'NONE', #47544, 39.37007874015748143 ) ;
#11565 = ORIENTED_EDGE ( 'NONE', *, *, #15275, .F. ) ;
#11566 = DIRECTION ( 'NONE',  ( 1.734723475976806848E-16, -0.000000000000000000, 1.000000000000000000 ) ) ;
#11567 = VERTEX_POINT ( 'NONE', #11364 ) ;
#11568 = ORIENTED_EDGE ( 'NONE', *, *, #44486, .F. ) ;
#11569 = DIRECTION ( 'NONE',  ( -0.9998717552508122886, -0.01601477604151181275, 0.000000000000000000 ) ) ;
#11570 = ORIENTED_EDGE ( 'NONE', *, *, #27046, .T. ) ;
#11571 = VECTOR ( 'NONE', #27861, 39.37007874015748143 ) ;
#11572 = EDGE_CURVE ( 'NONE', #26402, #38556, #22485, .T. ) ;
#11573 = CARTESIAN_POINT ( 'NONE',  ( -0.3381173457103609503, 6.692913385826772199, 2.138793126519845877 ) ) ;
#11574 = VERTEX_POINT ( 'NONE', #2862 ) ;
#11575 = EDGE_LOOP ( 'NONE', ( #35167, #33777, #21563, #4332 ) ) ;
#11576 = ADVANCED_FACE ( 'NONE', ( #46448 ), #30738, .F. ) ;
#11577 = DIRECTION ( 'NONE',  ( -0.7071067811865466846, -0.7071067811865483499, -6.409875621278517705E-17 ) ) ;
#11578 = CARTESIAN_POINT ( 'NONE',  ( -2.454875160333845674, 3.232777166330581320, -0.1574803149606298636 ) ) ;
#11579 = ORIENTED_EDGE ( 'NONE', *, *, #19428, .T. ) ;
#11580 = CARTESIAN_POINT ( 'NONE',  ( -0.5455278134075208785, 0.000000000000000000, 1.377952755905504256 ) ) ;
#11581 = VERTEX_POINT ( 'NONE', #38243 ) ;
#11582 = CARTESIAN_POINT ( 'NONE',  ( 0.8182917201112819283, 3.267716535433071279, -0.1574803149606301411 ) ) ;
#11583 = PLANE ( 'NONE',  #31620 ) ;
#11584 = CARTESIAN_POINT ( 'NONE',  ( -0.3486774197067337711, 3.267716535433071279, 1.209717811016578338E-16 ) ) ;
#11585 = EDGE_CURVE ( 'NONE', #11040, #12778, #29302, .T. ) ;
#11586 = VERTEX_POINT ( 'NONE', #37735 ) ;
#11587 = ORIENTED_EDGE ( 'NONE', *, *, #30685, .T. ) ;
#11588 = DIRECTION ( 'NONE',  ( 0.000000000000000000, 0.000000000000000000, -1.000000000000000000 ) ) ;
#11589 = LINE ( 'NONE', #27325, #24516 ) ;
#11590 = CARTESIAN_POINT ( 'NONE',  ( -1.091055626815042201, 3.267716535433071279, 0.4330708661417290162 ) ) ;
#11591 = DIRECTION ( 'NONE',  ( -1.729310098864894520E-17, 1.000000000000000000, -1.276627980444842972E-16 ) ) ;
#11592 = FACE_OUTER_BOUND ( 'NONE', #7198, .T. ) ;
#11593 = AXIS2_PLACEMENT_3D ( 'NONE', #10205, #6840, #25955 ) ;
#11594 = CIRCLE ( 'NONE', #18205, 2.244934639244525076 ) ;
#11595 = CARTESIAN_POINT ( 'NONE',  ( 0.1067246931122726866, 0.02962905676920215767, 0.000000000000000000 ) ) ;
#11596 = ORIENTED_EDGE ( 'NONE', *, *, #42809, .F. ) ;
#11597 = LINE ( 'NONE', #489, #36609 ) ;
#11598 = EDGE_LOOP ( 'NONE', ( #36240, #50614, #16843, #1901 ) ) ;
#11599 = DIRECTION ( 'NONE',  ( -3.469446951953613696E-16, 0.000000000000000000, -1.000000000000000000 ) ) ;
#11600 = VECTOR ( 'NONE', #13355, 39.37007874015748143 ) ;
#11601 = ORIENTED_EDGE ( 'NONE', *, *, #2556, .T. ) ;
#11602 = ORIENTED_EDGE ( 'NONE', *, *, #27769, .F. ) ;
#11603 = DIRECTION ( 'NONE',  ( 1.000000000000000000, 0.000000000000000000, -3.469446951953613696E-16 ) ) ;
#11604 = CARTESIAN_POINT ( 'NONE',  ( 0.000000000000000000, 3.267716535433071279, 1.732283464566921172 ) ) ;
#11605 = EDGE_CURVE ( 'NONE', #14773, #31439, #50052, .T. ) ;
#11606 = ORIENTED_EDGE ( 'NONE', *, *, #14541, .F. ) ;
#11607 = EDGE_CURVE ( 'NONE', #45259, #45523, #18104, .T. ) ;
#11608 = EDGE_CURVE ( 'NONE', #21172, #575, #42345, .T. ) ;
#11609 = CARTESIAN_POINT ( 'NONE',  ( 0.000000000000000000, 6.692913385826772199, 0.000000000000000000 ) ) ;
#11610 = VERTEX_POINT ( 'NONE', #22989 ) ;
#11611 = CARTESIAN_POINT ( 'NONE',  ( 1.909347346926324684, 3.346456692913386100, 0.4724409448818868706 ) ) ;
#11612 = VERTEX_POINT ( 'NONE', #14225 ) ;
#11613 = CARTESIAN_POINT ( 'NONE',  ( 2.136190583516914820, 1.205361022782829114E-17, -0.1451986319116555235 ) ) ;
#11614 = DIRECTION ( 'NONE',  ( -0.01601477604151182663, 0.9998717552508123996, -0.000000000000000000 ) ) ;
#11615 = EDGE_LOOP ( 'NONE', ( #21883, #12922, #35801, #40905 ) ) ;
#11616 = CARTESIAN_POINT ( 'NONE',  ( -2.071704270381554913, 3.346456692913386100, -0.6299212598425177889 ) ) ;
#11617 = ORIENTED_EDGE ( 'NONE', *, *, #25727, .T. ) ;
#11618 = ORIENTED_EDGE ( 'NONE', *, *, #50865, .T. ) ;
#11619 = CARTESIAN_POINT ( 'NONE',  ( -0.5085650345005219286, 1.025569181085919546, 2.526811340751392354 ) ) ;
#11620 = LINE ( 'NONE', #44889, #8364 ) ;
#11621 = DIRECTION ( 'NONE',  ( -1.000000000000000000, -0.000000000000000000, -0.000000000000000000 ) ) ;
#11622 = EDGE_CURVE ( 'NONE', #28528, #46686, #29974, .T. ) ;
#11623 = CONICAL_SURFACE ( 'NONE', #30586, 2.165354330708661568, 0.2617993877991570129 ) ;
#11624 = ORIENTED_EDGE ( 'NONE', *, *, #10847, .T. ) ;
#11625 = ADVANCED_FACE ( 'NONE', ( #12381 ), #28513, .T. ) ;
#11626 = VECTOR ( 'NONE', #13108, 39.37007874015748143 ) ;
#11627 = CARTESIAN_POINT ( 'NONE',  ( 0.4098391620725875262, 1.049866565067838486, 1.982786943644938793 ) ) ;
#11628 = PLANE ( 'NONE',  #38225 ) ;
#11629 = ORIENTED_EDGE ( 'NONE', *, *, #31742, .F. ) ;
#11630 = ADVANCED_FACE ( 'NONE', ( #15735 ), #32014, .F. ) ;
#11631 = DIRECTION ( 'NONE',  ( -3.469446951953613696E-16, 0.000000000000000000, -1.000000000000000000 ) ) ;
#11632 = ADVANCED_FACE ( 'NONE', ( #47194 ), #43093, .T. ) ;
#11633 = EDGE_CURVE ( 'NONE', #26232, #17597, #15997, .T. ) ;
#11634 = VERTEX_POINT ( 'NONE', #43860 ) ;
#11635 = ORIENTED_EDGE ( 'NONE', *, *, #40884, .F. ) ;
#11636 = VECTOR ( 'NONE', #49809, 39.37007874015748143 ) ;
#11637 = DIRECTION ( 'NONE',  ( -0.4357934065752705477, 0.2785571346213377986, 0.8558563136047259157 ) ) ;
#11638 = ORIENTED_EDGE ( 'NONE', *, *, #7210, .F. ) ;
#11639 = CARTESIAN_POINT ( 'NONE',  ( 2.623503965249849301, 1.760141956857387724, 1.355882097269874187 ) ) ;
#11640 = AXIS2_PLACEMENT_3D ( 'NONE', #35289, #160, #44041 ) ;
#11641 = CARTESIAN_POINT ( 'NONE',  ( -0.07591351300297333182, 3.346456692913386100, -1.417322834645664331 ) ) ;
#11642 =( BOUNDED_CURVE ( )  B_SPLINE_CURVE ( 3, ( #32635, #20996, #44727, #1882 ),
 .UNSPECIFIED., .F., .F. ) 
 B_SPLINE_CURVE_WITH_KNOTS ( ( 4, 4 ),
 ( 2.670688157552317588, 2.721475174429009325 ),
 .UNSPECIFIED. ) 
 CURVE ( )  GEOMETRIC_REPRESENTATION_ITEM ( )  RATIONAL_B_SPLINE_CURVE ( ( 1.000000000000000000, 0.9997850681263177330, 0.9997850681263177330, 1.000000000000000000 ) ) 
 REPRESENTATION_ITEM ( '' )  );
#11643 = CARTESIAN_POINT ( 'NONE',  ( -0.6529837180168072130, 0.8335264911517247244, 0.6529837180168073241 ) ) ;
#11644 = CARTESIAN_POINT ( 'NONE',  ( 1.686980615242215098, -1.638433421555315900E-16, 1.408267424185159156 ) ) ;
#11645 = ORIENTED_EDGE ( 'NONE', *, *, #17366, .F. ) ;
#11646 = ORIENTED_EDGE ( 'NONE', *, *, #23546, .F. ) ;
#11647 = CARTESIAN_POINT ( 'NONE',  ( -2.164823134740036181, 1.673236549936605977, -0.04796011690018290446 ) ) ;
#11648 = VERTEX_POINT ( 'NONE', #51050 ) ;
#11649 = DIRECTION ( 'NONE',  ( 1.000000000000000000, 0.000000000000000000, -3.469446951953613696E-16 ) ) ;
#11650 = DIRECTION ( 'NONE',  ( -3.469446951953613696E-16, 0.000000000000000000, -1.000000000000000000 ) ) ;
#11651 = LINE ( 'NONE', #32055, #32521 ) ;
#11652 = CARTESIAN_POINT ( 'NONE',  ( -0.8182917201112814842, 0.000000000000000000, 1.102362204724404160 ) ) ;
#11653 = DIRECTION ( 'NONE',  ( -0.000000000000000000, 0.000000000000000000, 1.000000000000000000 ) ) ;
#11654 = ORIENTED_EDGE ( 'NONE', *, *, #38435, .F. ) ;
#11655 = DIRECTION ( 'NONE',  ( 0.9989930665413144784, -5.247434042673083099E-18, 0.04486483035051863633 ) ) ;
#11656 = DIRECTION ( 'NONE',  ( -0.9998717552508122886, -0.01601477604151182316, 0.000000000000000000 ) ) ;
#11657 = ORIENTED_EDGE ( 'NONE', *, *, #25041, .F. ) ;
#11658 = AXIS2_PLACEMENT_3D ( 'NONE', #33211, #48894, #13586 ) ;
#11659 = ORIENTED_EDGE ( 'NONE', *, *, #48452, .F. ) ;
#11660 = DIRECTION ( 'NONE',  ( -0.000000000000000000, 1.000000000000000000, -0.000000000000000000 ) ) ;
#11661 = AXIS2_PLACEMENT_3D ( 'NONE', #48110, #8653, #5038 ) ;
#11662 = CARTESIAN_POINT ( 'NONE',  ( -0.8182917201112814842, 0.000000000000000000, 1.732283464566921172 ) ) ;
#11663 = DIRECTION ( 'NONE',  ( -0.8805955318567391110, 0.000000000000000000, 0.4738686624729965269 ) ) ;
#11664 = ORIENTED_EDGE ( 'NONE', *, *, #7180, .F. ) ;
#11665 = ADVANCED_FACE ( 'NONE', ( #509 ), #19602, .F. ) ;
#11666 = CONICAL_SURFACE ( 'NONE', #24052, 2.244934639244524632, 1.554780866114618743 ) ;
#11667 = B_SPLINE_CURVE_WITH_KNOTS ( 'NONE', 3,
 ( #3560, #4078, #46886, #11559 ),
 .UNSPECIFIED., .F., .F.,
 ( 4, 4 ),
 ( 4.925214732546996801E-05, 0.05034361238089160584 ),
 .UNSPECIFIED. ) ;
#11668 = ADVANCED_FACE ( 'NONE', ( #20114 ), #15493, .F. ) ;
#11669 = ORIENTED_EDGE ( 'NONE', *, *, #49095, .F. ) ;
#11670 = DIRECTION ( 'NONE',  ( -6.104789737168038204E-17, 1.000000000000000000, -1.134460028949771622E-16 ) ) ;
#11671 = AXIS2_PLACEMENT_3D ( 'NONE', #44131, #48734, #49250 ) ;
#11672 = VERTEX_POINT ( 'NONE', #11613 ) ;
#11673 = CARTESIAN_POINT ( 'NONE',  ( 0.000000000000000000, 1.574803149606302854, 0.000000000000000000 ) ) ;
#11674 = EDGE_CURVE ( 'NONE', #4283, #7287, #7994, .T. ) ;
#11675 = VERTEX_POINT ( 'NONE', #27100 ) ;
#11676 = CARTESIAN_POINT ( 'NONE',  ( 1.909347346926324684, 0.000000000000000000, 0.5905511811023582691 ) ) ;
#11677 = DIRECTION ( 'NONE',  ( 0.000000000000000000, 0.000000000000000000, -1.000000000000000000 ) ) ;
#11678 = CARTESIAN_POINT ( 'NONE',  ( -1.909347346926324906, 0.000000000000000000, -0.7874015748031470974 ) ) ;
#11679 = VERTEX_POINT ( 'NONE', #35374 ) ;
#11680 = EDGE_LOOP ( 'NONE', ( #42931, #15965, #16547, #1635 ) ) ;
#11681 = ORIENTED_EDGE ( 'NONE', *, *, #28818, .T. ) ;
#11682 = DIRECTION ( 'NONE',  ( -1.000000000000000000, 0.000000000000000000, -0.000000000000000000 ) ) ;
#11683 = CARTESIAN_POINT ( 'NONE',  ( -0.8182917201112819283, 3.267716535433071279, -0.9842519685039342603 ) ) ;
#11684 = EDGE_LOOP ( 'NONE', ( #40604, #5551, #7989, #50179 ) ) ;
#11685 = ORIENTED_EDGE ( 'NONE', *, *, #32856, .F. ) ;
#11686 = DIRECTION ( 'NONE',  ( 0.000000000000000000, 0.000000000000000000, -1.000000000000000000 ) ) ;
#11687 = FACE_OUTER_BOUND ( 'NONE', #48421, .T. ) ;
#11688 = DIRECTION ( 'NONE',  ( -0.01601477604151182663, 0.9998717552508123996, -0.000000000000000000 ) ) ;
#11689 = ORIENTED_EDGE ( 'NONE', *, *, #35623, .F. ) ;
#11690 = ORIENTED_EDGE ( 'NONE', *, *, #6457, .F. ) ;
#11691 = ADVANCED_FACE ( 'NONE', ( #38982 ), #40007, .F. ) ;
#11692 = CARTESIAN_POINT ( 'NONE',  ( 2.347234779702823460, 1.650446160227867498, -0.9497368662867726741 ) ) ;
#11693 = CARTESIAN_POINT ( 'NONE',  ( -1.556712866041156440, 1.694999912340861004, 2.509548638715847435 ) ) ;
#11694 = CARTESIAN_POINT ( 'NONE',  ( -1.363819533518803473, 3.267716535433071279, -1.102362204724405270 ) ) ;
#11695 = VERTEX_POINT ( 'NONE', #20382 ) ;
#11696 = CARTESIAN_POINT ( 'NONE',  ( -2.182111253630085290, 3.346456692913386100, 0.4330708661417290162 ) ) ;
#11697 = DIRECTION ( 'NONE',  ( -1.000000000000000000, 0.000000000000000000, 1.734723475976806848E-16 ) ) ;
#11698 = ORIENTED_EDGE ( 'NONE', *, *, #23423, .F. ) ;
#11699 = EDGE_CURVE ( 'NONE', #44656, #48838, #39234, .T. ) ;
#11700 = DIRECTION ( 'NONE',  ( -1.000000000000000000, -0.000000000000000000, -0.000000000000000000 ) ) ;
#11701 = VERTEX_POINT ( 'NONE', #24262 ) ;
#11702 = ORIENTED_EDGE ( 'NONE', *, *, #42900, .T. ) ;
#11703 = LINE ( 'NONE', #11957, #40278 ) ;
#11704 = DIRECTION ( 'NONE',  ( -0.9989930665413151445, 0.000000000000000000, 0.04486483035050446017 ) ) ;
#11705 = VECTOR ( 'NONE', #37782, 39.37007874015748143 ) ;
#11707 = VECTOR ( 'NONE', #11631, 39.37007874015748143 ) ;
#11706 = CARTESIAN_POINT ( 'NONE',  ( -0.3937007874015747699, 0.3937007874015748254, -1.220472440944881942 ) ) ;
#11708 = DIRECTION ( 'NONE',  ( -0.000000000000000000, -1.000000000000000000, -0.000000000000000000 ) ) ;
#11709 = DIRECTION ( 'NONE',  ( 1.000000000000000000, 0.000000000000000000, -3.469446951953613696E-16 ) ) ;
#11710 = ORIENTED_EDGE ( 'NONE', *, *, #2043, .F. ) ;
#11711 = ORIENTED_EDGE ( 'NONE', *, *, #6642, .F. ) ;
#11712 = AXIS2_PLACEMENT_3D ( 'NONE', #18561, #29920, #6433 ) ;
#11713 = VECTOR ( 'NONE', #42745, 39.37007874015748143 ) ;
#11714 = ORIENTED_EDGE ( 'NONE', *, *, #39841, .F. ) ;
#11715 = CARTESIAN_POINT ( 'NONE',  ( -1.091055626815042645, 3.267716535433071279, 1.801691980386209258 ) ) ;
#11716 = LINE ( 'NONE', #48066, #33363 ) ;
#11717 = VECTOR ( 'NONE', #31172, 39.37007874015748143 ) ;
#11718 = CARTESIAN_POINT ( 'NONE',  ( 0.000000000000000000, 2.344748451760389596, 0.000000000000000000 ) ) ;
#11719 = DIRECTION ( 'NONE',  ( 0.000000000000000000, 0.000000000000000000, -1.000000000000000000 ) ) ;
#11720 = EDGE_LOOP ( 'NONE', ( #30492, #29158, #36509, #13733 ) ) ;
#11721 = LINE ( 'NONE', #27460, #8514 ) ;
#11722 = PLANE ( 'NONE',  #17464 ) ;
#11723 = VERTEX_POINT ( 'NONE', #35877 ) ;
#11724 = CARTESIAN_POINT ( 'NONE',  ( -1.205050450470247725, 0.008618577144216254052, 1.304493073717302165 ) ) ;
#11725 = LINE ( 'NONE', #10726, #26952 ) ;
#11726 = DIRECTION ( 'NONE',  ( -0.000000000000000000, 1.000000000000000000, -0.000000000000000000 ) ) ;
#11727 = ORIENTED_EDGE ( 'NONE', *, *, #3130, .T. ) ;
#11728 = CARTESIAN_POINT ( 'NONE',  ( 0.1968503937007878568, 3.346456692913386100, 2.156388021673882438 ) ) ;
#11729 = DIRECTION ( 'NONE',  ( -1.000000000000000000, 0.000000000000000000, -0.000000000000000000 ) ) ;
#11730 = FACE_OUTER_BOUND ( 'NONE', #1776, .T. ) ;
#11731 = EDGE_CURVE ( 'NONE', #38209, #20260, #32271, .T. ) ;
#11732 = EDGE_CURVE ( 'NONE', #27199, #17243, #31754, .T. ) ;
#11733 = VERTEX_POINT ( 'NONE', #27351 ) ;
#11734 = DIRECTION ( 'NONE',  ( -0.000000000000000000, 0.000000000000000000, 1.000000000000000000 ) ) ;
#11735 = ORIENTED_EDGE ( 'NONE', *, *, #5648, .T. ) ;
#11736 = LINE ( 'NONE', #3491, #7247 ) ;
#11737 = EDGE_CURVE ( 'NONE', #49343, #27036, #47963, .T. ) ;
#11738 = CIRCLE ( 'NONE', #15858, 2.165354330708661568 ) ;
#11739 = CARTESIAN_POINT ( 'NONE',  ( 1.909347346926324684, 3.346456692913386100, 0.5905511811023582691 ) ) ;
#11740 = LINE ( 'NONE', #8126, #444 ) ;
#11741 = ADVANCED_FACE ( 'NONE', ( #42845 ), #43606, .F. ) ;
#11742 = CIRCLE ( 'NONE', #9282, 2.106299212598425008 ) ;
#11743 = EDGE_LOOP ( 'NONE', ( #46911, #23339, #8851, #8659 ) ) ;
#11744 = VERTEX_POINT ( 'NONE', #23231 ) ;
#11745 = DIRECTION ( 'NONE',  ( 1.734723475976806848E-16, -0.000000000000000000, 1.000000000000000000 ) ) ;
#11746 = CARTESIAN_POINT ( 'NONE',  ( 0.6529837180168055477, 0.8335264911517253905, -0.6529837180168074351 ) ) ;
#11747 = ORIENTED_EDGE ( 'NONE', *, *, #41706, .T. ) ;
#11748 = VECTOR ( 'NONE', #1009, 39.37007874015748143 ) ;
#11749 = DIRECTION ( 'NONE',  ( 1.000000000000000000, 0.000000000000000000, -3.469446951953613696E-16 ) ) ;
#11750 = LINE ( 'NONE', #50932, #36787 ) ;
#11751 = LINE ( 'NONE', #50933, #9587 ) ;
#11752 = VECTOR ( 'NONE', #991, 39.37007874015748143 ) ;
#11753 = CARTESIAN_POINT ( 'NONE',  ( -1.722315009890285964, 1.692409705881639859, -2.398471918869278241 ) ) ;
#11754 = CIRCLE ( 'NONE', #43061, 1.743387098533651480 ) ;
#11755 = VERTEX_POINT ( 'NONE', #3619 ) ;
#11756 = EDGE_CURVE ( 'NONE', #29154, #9083, #25282, .T. ) ;
#11757 = ORIENTED_EDGE ( 'NONE', *, *, #46574, .F. ) ;
#11758 = CARTESIAN_POINT ( 'NONE',  ( 0.000000000000000000, 1.574803149606302854, 0.000000000000000000 ) ) ;
#11759 = DIRECTION ( 'NONE',  ( 1.000000000000000000, 0.000000000000000000, 0.000000000000000000 ) ) ;
#11760 = ORIENTED_EDGE ( 'NONE', *, *, #14003, .F. ) ;
#11761 = EDGE_CURVE ( 'NONE', #39073, #36917, #1531, .T. ) ;
#11762 = CARTESIAN_POINT ( 'NONE',  ( -1.909347346926324462, 3.346456692913386100, 1.021348170950612255 ) ) ;
#11763 = ORIENTED_EDGE ( 'NONE', *, *, #45329, .F. ) ;
#11764 = ORIENTED_EDGE ( 'NONE', *, *, #18809, .T. ) ;
#11765 = CARTESIAN_POINT ( 'NONE',  ( 1.953585199828835828, 3.346456692913386100, 0.7874015748031456541 ) ) ;
#11766 = ORIENTED_EDGE ( 'NONE', *, *, #38495, .T. ) ;
#11767 = VERTEX_POINT ( 'NONE', #44624 ) ;
#11768 = PLANE ( 'NONE',  #49958 ) ;
#11769 = ORIENTED_EDGE ( 'NONE', *, *, #42264, .F. ) ;
#11770 = CARTESIAN_POINT ( 'NONE',  ( 1.015142113812069091, 0.000000000000000000, -1.732283464566923614 ) ) ;
#11771 = EDGE_CURVE ( 'NONE', #26516, #37629, #18492, .T. ) ;
#11772 = DIRECTION ( 'NONE',  ( -0.000000000000000000, -1.000000000000000000, -0.000000000000000000 ) ) ;
#11773 = CARTESIAN_POINT ( 'NONE',  ( 0.7423782071083082634, 3.346456692913386100, -2.086614173228340086 ) ) ;
#11774 = DIRECTION ( 'NONE',  ( 0.000000000000000000, -0.000000000000000000, 1.000000000000000000 ) ) ;
#11775 = VECTOR ( 'NONE', #30058, 39.37007874015748143 ) ;
#11776 = DIRECTION ( 'NONE',  ( 1.734723475976806848E-16, -0.000000000000000000, 1.000000000000000000 ) ) ;
#11777 = DIRECTION ( 'NONE',  ( -1.000000000000000000, 0.000000000000000000, 1.734723475976806848E-16 ) ) ;
#11778 = ORIENTED_EDGE ( 'NONE', *, *, #13043, .F. ) ;
#11779 = DIRECTION ( 'NONE',  ( 1.734723475976806848E-16, -0.000000000000000000, 1.000000000000000000 ) ) ;
#11780 = CARTESIAN_POINT ( 'NONE',  ( -1.091055626815042645, 3.267716535433071279, -0.6299212598425177889 ) ) ;
#11781 = CARTESIAN_POINT ( 'NONE',  ( 0.04921259842519690175, 0.02870789531899127500, 1.849213118431110914 ) ) ;
#11782 = VECTOR ( 'NONE', #22206, 39.37007874015748143 ) ;
#11783 = AXIS2_PLACEMENT_3D ( 'NONE', #46422, #31220, #219 ) ;
#11784 = ORIENTED_EDGE ( 'NONE', *, *, #24264, .T. ) ;
#11785 = CARTESIAN_POINT ( 'NONE',  ( -0.8942052331142552601, 3.267716535433071279, 1.889763779527550147 ) ) ;
#11786 = CARTESIAN_POINT ( 'NONE',  ( -0.7869067874564349419, 0.000000000000000000, -1.671666005015433276 ) ) ;
#11787 = EDGE_LOOP ( 'NONE', ( #49054, #9261, #5360 ) ) ;
#11788 = LINE ( 'NONE', #35041, #29570 ) ;
#11789 = CARTESIAN_POINT ( 'NONE',  ( 2.283576142937052467, 0.5219377364620079174, -0.1518177250174685688 ) ) ;
#11790 = CARTESIAN_POINT ( 'NONE',  ( 0.3015460593140593115, 0.000000000000000000, 1.937268728265797213 ) ) ;
#11791 = AXIS2_PLACEMENT_3D ( 'NONE', #27779, #4047, #35539 ) ;
#11792 = CARTESIAN_POINT ( 'NONE',  ( 1.091055626815042645, 3.267716535433071279, -0.8267716535433055070 ) ) ;
#11793 = VERTEX_POINT ( 'NONE', #45830 ) ;
#11794 = DIRECTION ( 'NONE',  ( -1.000000000000000000, 0.000000000000000000, 1.734723475976806848E-16 ) ) ;
#11795 = ADVANCED_FACE ( 'NONE', ( #28377 ), #28891, .F. ) ;
#11796 = LINE ( 'NONE', #42534, #25871 ) ;
#11797 = CARTESIAN_POINT ( 'NONE',  ( 2.106197740627111514, 3.201134874551266218, -1.299212598425194320 ) ) ;
#11799 = EDGE_CURVE ( 'NONE', #27409, #329, #16777, .T. ) ;
#11798 = PLANE ( 'NONE',  #5353 ) ;
#11800 = ORIENTED_EDGE ( 'NONE', *, *, #15285, .T. ) ;
#11801 = EDGE_CURVE ( 'NONE', #3259, #13403, #25025, .T. ) ;
#11802 = ORIENTED_EDGE ( 'NONE', *, *, #3588, .F. ) ;
#11803 = ORIENTED_EDGE ( 'NONE', *, *, #16002, .F. ) ;
#11804 = CARTESIAN_POINT ( 'NONE',  ( 1.836342932631641167, 0.000000000000000000, 1.044063857347276469 ) ) ;
#11805 = ORIENTED_EDGE ( 'NONE', *, *, #20608, .T. ) ;
#11806 = LINE ( 'NONE', #47395, #31212 ) ;
#11807 = DIRECTION ( 'NONE',  ( -0.000000000000000000, -1.000000000000000000, -0.000000000000000000 ) ) ;
#11808 = ORIENTED_EDGE ( 'NONE', *, *, #14954, .F. ) ;
#11809 = CARTESIAN_POINT ( 'NONE',  ( 1.091055626815042645, 0.000000000000000000, 0.1181102362204704270 ) ) ;
#11810 = ORIENTED_EDGE ( 'NONE', *, *, #29204, .T. ) ;
#11811 = LINE ( 'NONE', #4083, #10096 ) ;
#11812 = VECTOR ( 'NONE', #37181, 39.37007874015748143 ) ;
#11813 = LINE ( 'NONE', #31702, #50310 ) ;
#11814 = ORIENTED_EDGE ( 'NONE', *, *, #9889, .T. ) ;
#11815 = VERTEX_POINT ( 'NONE', #9278 ) ;
#11816 = DIRECTION ( 'NONE',  ( -1.000000000000000000, 0.000000000000000000, -0.000000000000000000 ) ) ;
#11817 = VECTOR ( 'NONE', #20234, 39.37007874015748143 ) ;
#11818 = VERTEX_POINT ( 'NONE', #33299 ) ;
#11819 = AXIS2_PLACEMENT_3D ( 'NONE', #43575, #4101, #27829 ) ;
#11820 = AXIS2_PLACEMENT_3D ( 'NONE', #49082, #5244, #36752 ) ;
#11821 = CARTESIAN_POINT ( 'NONE',  ( 0.000000000000000000, 3.267716535433071279, 1.574803149606291974 ) ) ;
#11822 = EDGE_CURVE ( 'NONE', #12892, #41081, #34250, .T. ) ;
#11823 = ORIENTED_EDGE ( 'NONE', *, *, #37478, .T. ) ;
#11824 = ORIENTED_EDGE ( 'NONE', *, *, #11412, .T. ) ;
#11825 = CARTESIAN_POINT ( 'NONE',  ( 1.771435203777392386, 1.736274727556916808, 1.475617711110977615 ) ) ;
#11826 = VECTOR ( 'NONE', #21769, 39.37007874015748143 ) ;
#11827 = CARTESIAN_POINT ( 'NONE',  ( -1.843472447131334624, 1.579950168977349412, -1.157898127912315944 ) ) ;
#11828 = VERTEX_POINT ( 'NONE', #1276 ) ;
#11829 = CARTESIAN_POINT ( 'NONE',  ( 0.08139965876239094178, 1.610780518492231694, 0.000000000000000000 ) ) ;
#11830 = EDGE_CURVE ( 'NONE', #23434, #15077, #36394, .T. ) ;
#11831 = ORIENTED_EDGE ( 'NONE', *, *, #48650, .T. ) ;
#11832 = CARTESIAN_POINT ( 'NONE',  ( 2.100227814008711391, 1.467797480264206866, -2.076109931251913565 ) ) ;
#11833 = CARTESIAN_POINT ( 'NONE',  ( 1.560669927219590525, 3.267716535433071279, -0.03937007874015908959 ) ) ;
#11834 = DIRECTION ( 'NONE',  ( 0.000000000000000000, 0.000000000000000000, -1.000000000000000000 ) ) ;
#11835 = EDGE_LOOP ( 'NONE', ( #25811, #50938, #8499, #21645 ) ) ;
#11836 = VERTEX_POINT ( 'NONE', #6624 ) ;
#11837 = LINE ( 'NONE', #3335, #4669 ) ;
#11838 = CARTESIAN_POINT ( 'NONE',  ( -2.949046704851476353, 1.673284050348918583, -0.1488625813693291167 ) ) ;
#11839 = CARTESIAN_POINT ( 'NONE',  ( 1.833433833923351353, 3.346456692913386100, -0.9448818897637765168 ) ) ;
#11840 = EDGE_CURVE ( 'NONE', #38140, #22211, #38006, .T. ) ;
#11841 = CARTESIAN_POINT ( 'NONE',  ( 2.695799277629594037, 1.662794757381320654, -1.205759334241453651 ) ) ;
#11842 = ADVANCED_FACE ( 'NONE', ( #37168 ), #3791, .T. ) ;
#11843 = DIRECTION ( 'NONE',  ( -0.000000000000000000, -1.000000000000000000, -0.000000000000000000 ) ) ;
#11844 = LINE ( 'NONE', #8234, #28426 ) ;
#11845 = ORIENTED_EDGE ( 'NONE', *, *, #38896, .T. ) ;
#11846 = DIRECTION ( 'NONE',  ( 0.000000000000000000, 0.000000000000000000, 1.000000000000000000 ) ) ;
#11847 = VECTOR ( 'NONE', #44779, 39.37007874015748143 ) ;
#11848 = ORIENTED_EDGE ( 'NONE', *, *, #2503, .T. ) ;
#11849 = DIRECTION ( 'NONE',  ( -3.469446951953613696E-16, 0.000000000000000000, -1.000000000000000000 ) ) ;
#11850 = CIRCLE ( 'NONE', #10211, 1.850107469027523432 ) ;
#11851 = EDGE_LOOP ( 'NONE', ( #26186, #17368, #17472, #27037 ) ) ;
#11852 = VECTOR ( 'NONE', #29004, 39.37007874015748143 ) ;
#11853 = EDGE_CURVE ( 'NONE', #24076, #28575, #24774, .T. ) ;
#11855 = VECTOR ( 'NONE', #3913, 39.37007874015748143 ) ;
#11854 = CARTESIAN_POINT ( 'NONE',  ( -0.07591351300297284610, 3.267716535433071279, 1.850393700787392293 ) ) ;
#11856 = LINE ( 'NONE', #39224, #36105 ) ;
#11857 = ORIENTED_EDGE ( 'NONE', *, *, #36304, .F. ) ;
#11858 = EDGE_CURVE ( 'NONE', #380, #12101, #41986, .T. ) ;
#11859 = EDGE_CURVE ( 'NONE', #38271, #196, #21412, .T. ) ;
#11860 = VECTOR ( 'NONE', #25321, 39.37007874015748143 ) ;
#11861 = CARTESIAN_POINT ( 'NONE',  ( -1.788632549858358844, 3.346456692913386100, 1.220472440944875059 ) ) ;
#11862 = EDGE_CURVE ( 'NONE', #12327, #34870, #33047, .T. ) ;
#11863 = ORIENTED_EDGE ( 'NONE', *, *, #47305, .T. ) ;
#11864 = DIRECTION ( 'NONE',  ( 0.000000000000000000, 0.000000000000000000, -1.000000000000000000 ) ) ;
#11865 = EDGE_LOOP ( 'NONE', ( #10292, #42063, #12346, #28554 ) ) ;
#11866 = CARTESIAN_POINT ( 'NONE',  ( -0.1692531782225912829, -0.6299212598425202314, 0.3335283217915853138 ) ) ;
#11867 = CARTESIAN_POINT ( 'NONE',  ( 0.000000000000000000, 3.267716535433071279, -1.574803149606293307 ) ) ;
#11868 = ORIENTED_EDGE ( 'NONE', *, *, #40634, .T. ) ;
#11869 = CARTESIAN_POINT ( 'NONE',  ( 1.930249146414562578, 0.05883613814988478824, 0.3111320644955062886 ) ) ;
#11870 = ORIENTED_EDGE ( 'NONE', *, *, #38433, .F. ) ;
#11871 = ORIENTED_EDGE ( 'NONE', *, *, #24355, .T. ) ;
#11872 = DIRECTION ( 'NONE',  ( 1.000000000000000000, 0.000000000000000000, -3.469446951953613696E-16 ) ) ;
#11873 = PLANE ( 'NONE',  #9996 ) ;
#11874 = DIRECTION ( 'NONE',  ( 0.000000000000000000, 0.000000000000000000, -1.000000000000000000 ) ) ;
#11875 = ORIENTED_EDGE ( 'NONE', *, *, #48721, .T. ) ;
#11876 = CARTESIAN_POINT ( 'NONE',  ( -1.593029370565769431, 3.346456692913386100, 1.377952755905504256 ) ) ;
#11877 = CARTESIAN_POINT ( 'NONE',  ( 2.932638728931774352, 1.447899366913586672, 0.3475908556738225297 ) ) ;
#11878 = ADVANCED_FACE ( 'NONE', ( #4894 ), #17036, .F. ) ;
#11879 = ORIENTED_EDGE ( 'NONE', *, *, #25507, .T. ) ;
#11880 = LINE ( 'NONE', #30755, #11707 ) ;
#11881 = AXIS2_PLACEMENT_3D ( 'NONE', #23011, #19372, #45970 ) ;
#11882 = VECTOR ( 'NONE', #23258, 39.37007874015748143 ) ;
#11883 = VERTEX_POINT ( 'NONE', #32791 ) ;
#11884 = AXIS2_PLACEMENT_3D ( 'NONE', #36746, #21246, #20477 ) ;
#11885 = ORIENTED_EDGE ( 'NONE', *, *, #31265, .T. ) ;
#11886 = ITEM_DEFINED_TRANSFORMATION ( 'NONE', 'NONE', #16838,  #26741 ) ;
#11887 = ADVANCED_FACE ( 'NONE', ( #29148 ), #48473, .F. ) ;
#11888 = VECTOR ( 'NONE', #3805, 39.37007874015748143 ) ;
#11889 = EDGE_LOOP ( 'NONE', ( #40690, #659, #13278, #35686 ) ) ;
#11890 = CARTESIAN_POINT ( 'NONE',  ( 1.025452293874513643, 0.4349011127721510994, 1.051609096396380005 ) ) ;
#11891 = AXIS2_PLACEMENT_3D ( 'NONE', #47690, #28096, #1000 ) ;
#11892 = DIRECTION ( 'NONE',  ( 1.000000000000000000, -0.000000000000000000, 0.000000000000000000 ) ) ;
#11893 = EDGE_CURVE ( 'NONE', #19488, #17373, #2137, .T. ) ;
#11894 = EDGE_CURVE ( 'NONE', #50620, #33133, #22615, .T. ) ;
#11895 = PLANE ( 'NONE',  #43432 ) ;
#11896 = CARTESIAN_POINT ( 'NONE',  ( 2.182111253630085290, 0.000000000000000000, 0.1181102362204698858 ) ) ;
#11897 = ORIENTED_EDGE ( 'NONE', *, *, #42636, .F. ) ;
#11898 = ORIENTED_EDGE ( 'NONE', *, *, #37185, .T. ) ;
#11899 = VECTOR ( 'NONE', #46930, 39.37007874015748143 ) ;
#11900 = CARTESIAN_POINT ( 'NONE',  ( -0.3136974817027967100, 1.522126940893053337, -2.936457595020224520 ) ) ;
#11901 = CARTESIAN_POINT ( 'NONE',  ( 1.560669927219590303, 3.267716535433071279, -1.614173228346452715 ) ) ;
#11902 = ORIENTED_EDGE ( 'NONE', *, *, #29400, .T. ) ;
#11903 = DIRECTION ( 'NONE',  ( -3.469446951953613696E-16, 0.000000000000000000, -1.000000000000000000 ) ) ;
#11904 = CARTESIAN_POINT ( 'NONE',  ( -1.551823387637203178, 1.049866565067837820, 1.300483131855000529 ) ) ;
#11905 = CARTESIAN_POINT ( 'NONE',  ( 1.363819533518803251, 3.346456692913386100, 0.1574803149606283648 ) ) ;
#11906 = LINE ( 'NONE', #284, #28540 ) ;
#11907 = CARTESIAN_POINT ( 'NONE',  ( 0.4330136603435739695, 0.5160455853568215456, -2.362204724409448620 ) ) ;
#11908 = ORIENTED_EDGE ( 'NONE', *, *, #1841, .F. ) ;
#11909 = CARTESIAN_POINT ( 'NONE',  ( 1.387241876633648285, 6.692913385826772199, 1.662624236931697919 ) ) ;
#11910 = LINE ( 'NONE', #23787, #6262 ) ;
#11911 = EDGE_CURVE ( 'NONE', #15133, #50731, #42975, .T. ) ;
#11912 = ORIENTED_EDGE ( 'NONE', *, *, #32691, .T. ) ;
#11914 = VERTEX_POINT ( 'NONE', #3001 ) ;
#11913 = ADVANCED_FACE ( 'NONE', ( #7878 ), #27491, .F. ) ;
#11915 = DIRECTION ( 'NONE',  ( -0.000000000000000000, 1.000000000000000000, -0.000000000000000000 ) ) ;
#11916 = CARTESIAN_POINT ( 'NONE',  ( 0.1968503937007876903, 3.267716535433071279, -6.829619984160666674E-17 ) ) ;
#11917 = DIRECTION ( 'NONE',  ( 1.734723475976806848E-16, 0.000000000000000000, 1.000000000000000000 ) ) ;
#11918 = VERTEX_POINT ( 'NONE', #26479 ) ;
#11919 = ADVANCED_FACE ( 'NONE', ( #39374 ), #7128, .F. ) ;
#11920 = EDGE_CURVE ( 'NONE', #50546, #4697, #11750, .T. ) ;
#11921 = AXIS2_PLACEMENT_3D ( 'NONE', #50153, #6595, #14588 ) ;
#11922 = EDGE_CURVE ( 'NONE', #7866, #20944, #1695, .T. ) ;
#11923 = ORIENTED_EDGE ( 'NONE', *, *, #37893, .F. ) ;
#11924 = VECTOR ( 'NONE', #15770, 39.37007874015748143 ) ;
#11925 = DIRECTION ( 'NONE',  ( -0.8584487936018727616, 0.000000000000000000, 0.5128992774058948045 ) ) ;
#11926 = ORIENTED_EDGE ( 'NONE', *, *, #27624, .T. ) ;
#11927 = CARTESIAN_POINT ( 'NONE',  ( 0.000000000000000000, 3.267716535433071279, -1.102362204724405270 ) ) ;
#11928 = VECTOR ( 'NONE', #1907, 39.37007874015748143 ) ;
#11929 = ORIENTED_EDGE ( 'NONE', *, *, #36020, .T. ) ;
#11930 = DIRECTION ( 'NONE',  ( 0.000000000000000000, -1.000000000000000000, 0.000000000000000000 ) ) ;
#11931 = DIRECTION ( 'NONE',  ( -0.04261736568783054679, -0.000000000000000000, -0.9990914673551315461 ) ) ;
#11932 = DIRECTION ( 'NONE',  ( 0.01601477604151182663, -0.9998717552508123996, 0.000000000000000000 ) ) ;
#11933 = ORIENTED_EDGE ( 'NONE', *, *, #26620, .F. ) ;
#11934 = DIMENSIONAL_EXPONENTS ( 1.000000000000000000, 0.000000000000000000, 0.000000000000000000, 0.000000000000000000, 0.000000000000000000, 0.000000000000000000, 0.000000000000000000 ) ;
#11935 = ORIENTED_EDGE ( 'NONE', *, *, #6968, .F. ) ;
#11936 = VERTEX_POINT ( 'NONE', #38371 ) ;
#11937 = CARTESIAN_POINT ( 'NONE',  ( -1.662320194739477675, 5.905511811023623991, -1.388601395075574896 ) ) ;
#11938 = AXIS2_PLACEMENT_3D ( 'NONE', #3387, #4148, #22761 ) ;
#11939 = CARTESIAN_POINT ( 'NONE',  ( 1.287906020515830585, 0.000000000000000000, 1.574803149606291974 ) ) ;
#11940 = ORIENTED_EDGE ( 'NONE', *, *, #19592, .T. ) ;
#11941 = ORIENTED_EDGE ( 'NONE', *, *, #30443, .F. ) ;
#11942 = CARTESIAN_POINT ( 'NONE',  ( 0.3344856439320825214, 0.000000000000000000, 1.935533671922775145 ) ) ;
#11943 = CARTESIAN_POINT ( 'NONE',  ( 0.000000000000000000, 6.692913385826772199, 0.000000000000000000 ) ) ;
#11944 = DIRECTION ( 'NONE',  ( -1.000000000000000000, 0.000000000000000000, 0.000000000000000000 ) ) ;
#11945 = ORIENTED_EDGE ( 'NONE', *, *, #13972, .F. ) ;
#11946 = ORIENTED_EDGE ( 'NONE', *, *, #26701, .T. ) ;
#11947 = CARTESIAN_POINT ( 'NONE',  ( 0.5455278134075217666, 3.346456692913386100, 1.259842519685033357 ) ) ;
#11948 = CARTESIAN_POINT ( 'NONE',  ( 0.3543214468173200293, 1.713577057256821190, 2.228085083314873316 ) ) ;
#11949 = DIRECTION ( 'NONE',  ( 0.000000000000000000, 0.000000000000000000, -1.000000000000000000 ) ) ;
#11950 = VERTEX_POINT ( 'NONE', #30616 ) ;
#11951 = CARTESIAN_POINT ( 'NONE',  ( 2.755905511811024056, 2.913385826771657250, -1.023622047244094224 ) ) ;
#11952 = DIRECTION ( 'NONE',  ( 1.734723475976806848E-16, -0.000000000000000000, 1.000000000000000000 ) ) ;
#11953 = ORIENTED_EDGE ( 'NONE', *, *, #49831, .T. ) ;
#11954 = LINE ( 'NONE', #35202, #43055 ) ;
#11955 = VERTEX_POINT ( 'NONE', #7629 ) ;
#11956 = ORIENTED_EDGE ( 'NONE', *, *, #26760, .F. ) ;
#11957 = CARTESIAN_POINT ( 'NONE',  ( -0.6214413264104945434, 3.346456692913386100, 2.047244094488179567 ) ) ;
#11958 = LINE ( 'NONE', #39834, #17692 ) ;
#11959 = CARTESIAN_POINT ( 'NONE',  ( -0.4892674838277497606, 1.703934057431762739, 2.420473071843689983 ) ) ;
#11960 = EDGE_CURVE ( 'NONE', #40968, #42434, #50429, .T. ) ;
#11961 = FACE_OUTER_BOUND ( 'NONE', #37239, .T. ) ;
#11962 = CARTESIAN_POINT ( 'NONE',  ( 1.287906020515830141, 3.346456692913386100, -8.878505979408855953E-16 ) ) ;
#11963 = ORIENTED_EDGE ( 'NONE', *, *, #8437, .F. ) ;
#11965 = ADVANCED_FACE ( 'NONE', ( #18744 ), #46086, .F. ) ;
#11964 = ORIENTED_EDGE ( 'NONE', *, *, #14695, .F. ) ;
#11966 = AXIS2_PLACEMENT_3D ( 'NONE', #46675, #42079, #38471 ) ;
#11967 = VECTOR ( 'NONE', #1542, 39.37007874015748143 ) ;
#11968 = VECTOR ( 'NONE', #487, 39.37007874015748143 ) ;
#11969 = ORIENTED_EDGE ( 'NONE', *, *, #11541, .T. ) ;
#11970 = CARTESIAN_POINT ( 'NONE',  ( -1.985260859929298016, 3.346456692913386100, -0.9448818897637762948 ) ) ;
#11971 = CARTESIAN_POINT ( 'NONE',  ( -2.156388021673881994, 3.346456692913386100, -0.1968503937007880511 ) ) ;
#11972 = AXIS2_PLACEMENT_3D ( 'NONE', #1650, #48848, #45005 ) ;
#11973 = B_SPLINE_CURVE_WITH_KNOTS ( 'NONE', 3,
 ( #5056, #149, #15898, #43516 ),
 .UNSPECIFIED., .F., .F.,
 ( 4, 4 ),
 ( 3.418973662664240344E-07, 0.04653147169244552933 ),
 .UNSPECIFIED. ) ;
#11974 = CARTESIAN_POINT ( 'NONE',  ( -1.236813753895213086, 1.601547340627394567, -2.681693691597581974 ) ) ;
#11975 = DIRECTION ( 'NONE',  ( 0.9510565162951500895, -3.590656546124792943E-17, 0.3090169943749582204 ) ) ;
#11976 = VECTOR ( 'NONE', #36012, 39.37007874015748143 ) ;
#11977 = ORIENTED_EDGE ( 'NONE', *, *, #19942, .T. ) ;
#11978 = DIRECTION ( 'NONE',  ( 1.000000000000000000, 0.000000000000000000, 0.000000000000000000 ) ) ;
#11979 = EDGE_CURVE ( 'NONE', #19240, #6809, #14523, .T. ) ;
#11980 = DIRECTION ( 'NONE',  ( -0.01601477604151182663, 0.9998717552508123996, -0.000000000000000000 ) ) ;
#11981 = VERTEX_POINT ( 'NONE', #3755 ) ;
#11982 = DIRECTION ( 'NONE',  ( -3.469446951953613696E-16, 0.000000000000000000, -1.000000000000000000 ) ) ;
#11983 = ADVANCED_FACE ( 'NONE', ( #10996 ), #42227, .F. ) ;
#11984 = CARTESIAN_POINT ( 'NONE',  ( 1.942974145993213053, 1.745987691644603323, -1.925760030027876990 ) ) ;
#11985 = LINE ( 'NONE', #27218, #10661 ) ;
#11986 = ORIENTED_EDGE ( 'NONE', *, *, #35882, .T. ) ;
#11987 = CARTESIAN_POINT ( 'NONE',  ( -2.182111253630085290, 3.267716535433071279, -0.5118110236220464460 ) ) ;
#11988 = CARTESIAN_POINT ( 'NONE',  ( -1.363819533518803473, 3.346456692913386100, -1.605145679676863057 ) ) ;
#11989 = EDGE_CURVE ( 'NONE', #23167, #38385, #19742, .T. ) ;
#11990 = CARTESIAN_POINT ( 'NONE',  ( -1.909347346926324906, 0.000000000000000000, -1.102362204724405492 ) ) ;
#11991 = ADVANCED_FACE ( 'NONE', ( #10742 ), #38622, .F. ) ;
#11992 = ORIENTED_EDGE ( 'NONE', *, *, #5458, .F. ) ;
#11993 = CARTESIAN_POINT ( 'NONE',  ( 0.5455278134075208785, 0.000000000000000000, -1.771653543307081025 ) ) ;
#11994 = ORIENTED_EDGE ( 'NONE', *, *, #26876, .F. ) ;
#11995 = FACE_OUTER_BOUND ( 'NONE', #10950, .T. ) ;
#11996 = CARTESIAN_POINT ( 'NONE',  ( -1.363819533518803029, 3.346456692913386100, 0.5905511811023582691 ) ) ;
#11997 = DIRECTION ( 'NONE',  ( -1.000000000000000000, 0.000000000000000000, -0.000000000000000000 ) ) ;
#11998 = CARTESIAN_POINT ( 'NONE',  ( 1.560669927219590747, 3.267716535433071279, 1.102362204724403938 ) ) ;
#11999 = ORIENTED_EDGE ( 'NONE', *, *, #12739, .F. ) ;
#12000 = ORIENTED_EDGE ( 'NONE', *, *, #47322, .F. ) ;
#12001 = DIRECTION ( 'NONE',  ( -3.469446951953613696E-16, 0.000000000000000000, -1.000000000000000000 ) ) ;
#12002 = VECTOR ( 'NONE', #29514, 39.37007874015748143 ) ;
#12003 = CARTESIAN_POINT ( 'NONE',  ( -1.439733046521777027, 3.346456692913386100, 1.377952755905504256 ) ) ;
#12004 = VECTOR ( 'NONE', #17456, 39.37007874015748143 ) ;
#12005 = ORIENTED_EDGE ( 'NONE', *, *, #16165, .T. ) ;
#12006 = DIRECTION ( 'NONE',  ( -3.469446951953613696E-16, 0.000000000000000000, -1.000000000000000000 ) ) ;
#12007 = CARTESIAN_POINT ( 'NONE',  ( -2.695799277629576718, 5.905511811023623991, -1.205759334241493175 ) ) ;
#12008 = CARTESIAN_POINT ( 'NONE',  ( -1.405548054723555707, 1.619772730168859365, 1.683577343699150575 ) ) ;
#12009 = VECTOR ( 'NONE', #40067, 39.37007874015748143 ) ;
#12010 = CARTESIAN_POINT ( 'NONE',  ( 1.015142113812069757, 3.267716535433071279, -3.521981712565033375E-16 ) ) ;
#12011 = VERTEX_POINT ( 'NONE', #50185 ) ;
#12012 = VERTEX_POINT ( 'NONE', #46335 ) ;
#12013 = ORIENTED_EDGE ( 'NONE', *, *, #33141, .F. ) ;
#12014 = CARTESIAN_POINT ( 'NONE',  ( 0.000000000000000000, 2.755905511811027164, 0.000000000000000000 ) ) ;
#12015 = VECTOR ( 'NONE', #45273, 39.37007874015748143 ) ;
#12016 = DIRECTION ( 'NONE',  ( 1.734723475976806848E-16, 0.000000000000000000, 1.000000000000000000 ) ) ;
#12017 = LINE ( 'NONE', #38877, #39717 ) ;
#12019 = VECTOR ( 'NONE', #8569, 39.37007874015748143 ) ;
#12018 = FACE_BOUND ( 'NONE', #10731, .T. ) ;
#12020 = ORIENTED_EDGE ( 'NONE', *, *, #18697, .F. ) ;
#12021 = CARTESIAN_POINT ( 'NONE',  ( -2.277873973731453727, 1.562946399538843290, 1.879489153247635214 ) ) ;
#12022 = ORIENTED_EDGE ( 'NONE', *, *, #2788, .F. ) ;
#12023 = ORIENTED_EDGE ( 'NONE', *, *, #37798, .T. ) ;
#12024 = CARTESIAN_POINT ( 'NONE',  ( -2.451020605438007482, 3.251186424478681225, -0.03937007874015881204 ) ) ;
#12025 = VERTEX_POINT ( 'NONE', #26735 ) ;
#12026 = ORIENTED_EDGE ( 'NONE', *, *, #42959, .F. ) ;
#12027 = CARTESIAN_POINT ( 'NONE',  ( -0.2727639067037610499, 0.000000000000000000, -2.047244094488181343 ) ) ;
#12028 = EDGE_LOOP ( 'NONE', ( #47185, #40918, #24307, #8085 ) ) ;
#12029 = EDGE_CURVE ( 'NONE', #7052, #10796, #44741, .T. ) ;
#12030 = ADVANCED_FACE ( 'NONE', ( #38869 ), #31125, .F. ) ;
#12031 = CARTESIAN_POINT ( 'NONE',  ( 0.000000000000000000, 3.267716535433071279, 0.4330708661417287386 ) ) ;
#12032 = CARTESIAN_POINT ( 'NONE',  ( 0.8329809839909850799, 1.633788288308783976, -2.833254665166554442 ) ) ;
#12033 = EDGE_CURVE ( 'NONE', #15466, #48433, #4517, .T. ) ;
#12034 = DIRECTION ( 'NONE',  ( 1.000000000000000000, 0.000000000000000000, -3.469446951953613696E-16 ) ) ;
#12035 = VECTOR ( 'NONE', #45989, 39.37007874015748143 ) ;
#12036 = DIRECTION ( 'NONE',  ( 1.000000000000000000, 0.000000000000000000, -3.469446951953613696E-16 ) ) ;
#12037 = CARTESIAN_POINT ( 'NONE',  ( 2.734482843737263025, 0.000000000000000000, -1.115254632218672937 ) ) ;
#12038 = LINE ( 'NONE', #35283, #28634 ) ;
#12039 = COLOUR_RGB ( '',0.7921568627450980005, 0.8196078431372548767, 0.9333333333333333481 ) ;
#12040 = ORIENTED_EDGE ( 'NONE', *, *, #13584, .F. ) ;
#12041 = FACE_OUTER_BOUND ( 'NONE', #9622, .T. ) ;
#12042 = AXIS2_PLACEMENT_3D ( 'NONE', #6391, #29103, #41254 ) ;
#12043 = CARTESIAN_POINT ( 'NONE',  ( -0.5455278134075208785, 3.346456692913386100, 1.889763779527550369 ) ) ;
#12044 = CARTESIAN_POINT ( 'NONE',  ( 0.000000000000000000, 3.267716535433071279, -1.929133858267711110 ) ) ;
#12045 = ORIENTED_EDGE ( 'NONE', *, *, #15254, .T. ) ;
#12046 = CARTESIAN_POINT ( 'NONE',  ( 0.000000000000000000, 3.267716535433071279, 1.535433070866133898 ) ) ;
#12047 = EDGE_CURVE ( 'NONE', #4899, #14448, #40656, .T. ) ;
#12048 = CYLINDRICAL_SURFACE ( 'NONE', #21183, 2.165354330708661568 ) ;
#12049 = ORIENTED_EDGE ( 'NONE', *, *, #50736, .T. ) ;
#12050 = CARTESIAN_POINT ( 'NONE',  ( -1.740978969773838037, 0.000000000000000000, 0.09160132170885167124 ) ) ;
#12051 = AXIS2_PLACEMENT_3D ( 'NONE', #12891, #36130, #29134 ) ;
#12052 = CARTESIAN_POINT ( 'NONE',  ( -0.8182917201112819283, 0.000000000000000000, -0.1574803149606301411 ) ) ;
#12053 = FACE_OUTER_BOUND ( 'NONE', #28231, .T. ) ;
#12054 = AXIS2_PLACEMENT_3D ( 'NONE', #45323, #30371, #49433 ) ;
#12055 = ADVANCED_FACE ( 'NONE', ( #12780 ), #40411, .F. ) ;
#12056 = CARTESIAN_POINT ( 'NONE',  ( 1.636583440222563857, 0.000000000000000000, 1.062992125984245639 ) ) ;
#12057 = ORIENTED_EDGE ( 'NONE', *, *, #21705, .F. ) ;
#12058 = DIRECTION ( 'NONE',  ( -0.000000000000000000, 1.000000000000000000, -0.000000000000000000 ) ) ;
#12059 = CARTESIAN_POINT ( 'NONE',  ( 1.630393911741433000, 1.635590496292660179, -1.626902725537468619 ) ) ;
#12060 = DIRECTION ( 'NONE',  ( -3.469446951953613696E-16, 0.000000000000000000, -1.000000000000000000 ) ) ;
#12061 = CARTESIAN_POINT ( 'NONE',  ( -2.182111253630085290, 0.000000000000000000, 0.6299212598425164567 ) ) ;
#12062 = ORIENTED_EDGE ( 'NONE', *, *, #40590, .T. ) ;
#12063 = ORIENTED_EDGE ( 'NONE', *, *, #50314, .T. ) ;
#12064 = VERTEX_POINT ( 'NONE', #28511 ) ;
#12065 = CARTESIAN_POINT ( 'NONE',  ( 0.2727639067037604947, 3.346456692913386100, 0.4724409448818868706 ) ) ;
#12066 = VERTEX_POINT ( 'NONE', #35756 ) ;
#12067 = LINE ( 'NONE', #7684, #24616 ) ;
#12068 = DIRECTION ( 'NONE',  ( -1.000000000000000000, 0.000000000000000000, 1.734723475976806848E-16 ) ) ;
#12069 = EDGE_CURVE ( 'NONE', #7241, #23605, #35504, .T. ) ;
#12070 = ORIENTED_EDGE ( 'NONE', *, *, #8663, .F. ) ;
#12071 = DIRECTION ( 'NONE',  ( -1.734839586111147642E-16, 0.000000000000000000, 1.000000000000000000 ) ) ;
#12072 = ORIENTED_EDGE ( 'NONE', *, *, #29948, .T. ) ;
#12073 = CARTESIAN_POINT ( 'NONE',  ( 1.015142113812069313, 3.267716535433071279, -3.521981712565032882E-16 ) ) ;
#12074 = CIRCLE ( 'NONE', #25274, 2.106299212598425008 ) ;
#12075 = CARTESIAN_POINT ( 'NONE',  ( 0.000000000000000000, 6.692913385826772199, 0.000000000000000000 ) ) ;
#12076 = VECTOR ( 'NONE', #30638, 39.37007874015748143 ) ;
#12077 = ORIENTED_EDGE ( 'NONE', *, *, #49769, .F. ) ;
#12078 = ORIENTED_EDGE ( 'NONE', *, *, #28475, .F. ) ;
#12079 = VECTOR ( 'NONE', #23086, 39.37007874015748143 ) ;
#12080 = CARTESIAN_POINT ( 'NONE',  ( 1.287906020515830141, 3.346456692913386100, 0.3149606299212578953 ) ) ;
#12081 = ORIENTED_EDGE ( 'NONE', *, *, #32686, .T. ) ;
#12082 = VECTOR ( 'NONE', #6806, 39.37007874015748143 ) ;
#12083 = DIRECTION ( 'NONE',  ( -3.469446951953613696E-16, 0.000000000000000000, -1.000000000000000000 ) ) ;
#12084 = AXIS2_PLACEMENT_3D ( 'NONE', #40172, #4796, #35777 ) ;
#12085 = VERTEX_POINT ( 'NONE', #8645 ) ;
#12086 = ORIENTED_EDGE ( 'NONE', *, *, #5348, .F. ) ;
#12087 = LINE ( 'NONE', #12595, #8351 ) ;
#12088 = CONICAL_SURFACE ( 'NONE', #12946, 2.244934639244524632, 1.554780866114618743 ) ;
#12089 = ADVANCED_FACE ( 'NONE', ( #8900 ), #24655, .F. ) ;
#12090 = CARTESIAN_POINT ( 'NONE',  ( 1.363819533518803695, 3.346456692913386100, 1.681890501046755748 ) ) ;
#12091 = ORIENTED_EDGE ( 'NONE', *, *, #44921, .F. ) ;
#12092 = CARTESIAN_POINT ( 'NONE',  ( 0.1946224253818716055, 1.718530757508495155, -2.711439145546752805 ) ) ;
#12093 = ORIENTED_EDGE ( 'NONE', *, *, #32283, .F. ) ;
#12094 = CARTESIAN_POINT ( 'NONE',  ( 0.000000000000000000, 0.000000000000000000, 0.000000000000000000 ) ) ;
#12095 = EDGE_CURVE ( 'NONE', #37382, #36994, #5028, .T. ) ;
#12096 = LINE ( 'NONE', #39974, #20065 ) ;
#12097 = EDGE_CURVE ( 'NONE', #23181, #13035, #124, .T. ) ;
#12098 = EDGE_CURVE ( 'NONE', #3114, #15411, #36531, .T. ) ;
#12099 = LINE ( 'NONE', #31985, #45336 ) ;
#12100 = ORIENTED_EDGE ( 'NONE', *, *, #50894, .F. ) ;
#12101 = VERTEX_POINT ( 'NONE', #13037 ) ;
#12102 = CARTESIAN_POINT ( 'NONE',  ( -1.477691947303356290, 1.684234009953186728, 1.616556376299586706 ) ) ;
#12103 = DIRECTION ( 'NONE',  ( -3.469446951953613696E-16, 0.000000000000000000, -1.000000000000000000 ) ) ;
#12104 = LINE ( 'NONE', #43328, #19229 ) ;
#12105 = FACE_OUTER_BOUND ( 'NONE', #26520, .T. ) ;
#12106 = FACE_OUTER_BOUND ( 'NONE', #21149, .T. ) ;
#12107 = CARTESIAN_POINT ( 'NONE',  ( 2.378961647330872786, 3.346456692913386100, 0.3149606299212573401 ) ) ;
#12108 = EDGE_CURVE ( 'NONE', #38164, #18815, #24138, .T. ) ;
#12109 = ORIENTED_EDGE ( 'NONE', *, *, #24237, .T. ) ;
#12110 = AXIS2_PLACEMENT_3D ( 'NONE', #22032, #33154, #9385 ) ;
#12111 = DIRECTION ( 'NONE',  ( -3.469446951953613696E-16, 0.000000000000000000, -1.000000000000000000 ) ) ;
#12112 = ORIENTED_EDGE ( 'NONE', *, *, #16826, .F. ) ;
#12113 = AXIS2_PLACEMENT_3D ( 'NONE', #39978, #4610, #24235 ) ;
#12114 = LINE ( 'NONE', #4367, #6129 ) ;
#12115 = ADVANCED_FACE ( 'NONE', ( #16910 ), #32670, .F. ) ;
#12116 = VERTEX_POINT ( 'NONE', #47843 ) ;
#12117 = LINE ( 'NONE', #15484, #28325 ) ;
#12118 = LINE ( 'NONE', #39741, #45145 ) ;
#12119 = CARTESIAN_POINT ( 'NONE',  ( -0.3486774197067342151, 0.000000000000000000, -2.204724409448810540 ) ) ;
#12120 = VECTOR ( 'NONE', #14512, 39.37007874015748143 ) ;
#12121 = ORIENTED_EDGE ( 'NONE', *, *, #32225, .F. ) ;
#12122 = ADVANCED_FACE ( 'NONE', ( #15871 ), #16397, .F. ) ;
#12123 = CARTESIAN_POINT ( 'NONE',  ( -0.5455278134075214336, 0.000000000000000000, -1.259842519685035134 ) ) ;
#12124 = VERTEX_POINT ( 'NONE', #12007 ) ;
#12125 = FACE_OUTER_BOUND ( 'NONE', #33658, .T. ) ;
#12126 = EDGE_CURVE ( 'NONE', #11080, #27247, #39886, .T. ) ;
#12127 = VERTEX_POINT ( 'NONE', #23883 ) ;
#12128 = CARTESIAN_POINT ( 'NONE',  ( 2.182111253630085290, 0.000000000000000000, 0.3149606299212573401 ) ) ;
#12129 = DIRECTION ( 'NONE',  ( 1.000000000000000000, -0.000000000000000000, 0.000000000000000000 ) ) ;
#12130 = ORIENTED_EDGE ( 'NONE', *, *, #9620, .T. ) ;
#12131 = CARTESIAN_POINT ( 'NONE',  ( 1.636583440222563857, 3.346456692913386100, 0.6299212598425164567 ) ) ;
#12132 = ORIENTED_EDGE ( 'NONE', *, *, #41942, .T. ) ;
#12133 = ORIENTED_EDGE ( 'NONE', *, *, #9881, .F. ) ;
#12134 = ADVANCED_FACE ( 'NONE', ( #16656 ), #39629, .F. ) ;
#12135 = DIRECTION ( 'NONE',  ( 1.734723475976806848E-16, -0.000000000000000000, 1.000000000000000000 ) ) ;
#12136 = LINE ( 'NONE', #27869, #30632 ) ;
#12137 = DIRECTION ( 'NONE',  ( -1.000000000000000000, 0.000000000000000000, 1.734723475976806848E-16 ) ) ;
#12138 = EDGE_CURVE ( 'NONE', #1443, #17373, #28253, .T. ) ;
#12139 = VERTEX_POINT ( 'NONE', #36276 ) ;
#12140 = DIRECTION ( 'NONE',  ( 0.7660444431189771253, 0.6427876096865404731, 2.214792131866782686E-16 ) ) ;
#12141 = CARTESIAN_POINT ( 'NONE',  ( -0.8942052331142560373, 3.267716535433071279, 3.102397620449225933E-16 ) ) ;
#12142 = VECTOR ( 'NONE', #30249, 39.37007874015748143 ) ;
#12143 = CONICAL_SURFACE ( 'NONE', #31094, 2.246510896728926010, 0.01601546068027819014 ) ;
#12144 = ORIENTED_EDGE ( 'NONE', *, *, #5179, .T. ) ;
#12145 = LINE ( 'NONE', #39510, #18344 ) ;
#12146 = ORIENTED_EDGE ( 'NONE', *, *, #23341, .F. ) ;
#12147 = ORIENTED_EDGE ( 'NONE', *, *, #15427, .F. ) ;
#12148 = ORIENTED_EDGE ( 'NONE', *, *, #14086, .F. ) ;
#12149 = DIRECTION ( 'NONE',  ( -3.469446951953613696E-16, 0.000000000000000000, -1.000000000000000000 ) ) ;
#12150 = EDGE_CURVE ( 'NONE', #12012, #20408, #900, .T. ) ;
#12151 = CARTESIAN_POINT ( 'NONE',  ( 0.000000000000000000, 3.267716535433071279, 0.000000000000000000 ) ) ;
#12152 = DIRECTION ( 'NONE',  ( -0.000000000000000000, 1.000000000000000000, -0.000000000000000000 ) ) ;
#12153 = ADVANCED_FACE ( 'NONE', ( #6043 ), #37556, .F. ) ;
#12154 = LINE ( 'NONE', #12930, #14004 ) ;
#12155 = ORIENTED_EDGE ( 'NONE', *, *, #13034, .T. ) ;
#12156 = EDGE_LOOP ( 'NONE', ( #32934, #45150, #17157, #16343 ) ) ;
#12157 = PLANE ( 'NONE',  #40327 ) ;
#12158 = CARTESIAN_POINT ( 'NONE',  ( 0.5455278134075214336, 3.267716535433071279, -9.463399047163224412E-17 ) ) ;
#12159 = CIRCLE ( 'NONE', #8887, 0.3740157480314960647 ) ;
#12160 = EDGE_LOOP ( 'NONE', ( #49466, #26596, #6573, #4515 ) ) ;
#12161 = CARTESIAN_POINT ( 'NONE',  ( -2.464291103507776359, 5.905511811023623991, -1.626664315311337594 ) ) ;
#12162 = PLANE ( 'NONE',  #36337 ) ;
#12163 = CARTESIAN_POINT ( 'NONE',  ( -0.3486774197067339376, 3.346456692913386100, -0.3149606299212593941 ) ) ;
#12164 = CARTESIAN_POINT ( 'NONE',  ( 1.818390528211208945, 3.346456692913386100, 1.062992125984245639 ) ) ;
#12165 = ORIENTED_EDGE ( 'NONE', *, *, #20123, .F. ) ;
#12166 = FACE_OUTER_BOUND ( 'NONE', #2814, .T. ) ;
#12167 = LINE ( 'NONE', #12423, #2131 ) ;
#12168 = ORIENTED_EDGE ( 'NONE', *, *, #8273, .F. ) ;
#12169 = VERTEX_POINT ( 'NONE', #41417 ) ;
#12170 = PLANE ( 'NONE',  #46338 ) ;
#12171 = CARTESIAN_POINT ( 'NONE',  ( -0.3486774197067334380, 0.000000000000000000, 1.259842519685033357 ) ) ;
#12172 = DIRECTION ( 'NONE',  ( 5.500355109725808462E-17, -1.000000000000000000, -1.022137253806221654E-16 ) ) ;
#12173 = CIRCLE ( 'NONE', #39382, 2.246510896728926010 ) ;
#12174 = ORIENTED_EDGE ( 'NONE', *, *, #2417, .T. ) ;
#12175 = VECTOR ( 'NONE', #32319, 39.37007874015748143 ) ;
#12176 = EDGE_CURVE ( 'NONE', #17328, #26916, #18177, .T. ) ;
#12177 = ORIENTED_EDGE ( 'NONE', *, *, #28654, .T. ) ;
#12178 = CARTESIAN_POINT ( 'NONE',  ( -0.5455278134075209895, 3.267716535433071279, 9.463399047163218249E-17 ) ) ;
#12179 = VECTOR ( 'NONE', #31196, 39.37007874015748143 ) ;
#12180 = ORIENTED_EDGE ( 'NONE', *, *, #24652, .T. ) ;
#12181 = CARTESIAN_POINT ( 'NONE',  ( 1.138972962972652603, 1.733361078862474258, -2.478525195789229585 ) ) ;
#12182 = EDGE_CURVE ( 'NONE', #36547, #5893, #29022, .T. ) ;
#12183 = ORIENTED_EDGE ( 'NONE', *, *, #43624, .F. ) ;
#12184 = VECTOR ( 'NONE', #17284, 39.37007874015748143 ) ;
#12185 = FACE_OUTER_BOUND ( 'NONE', #42986, .T. ) ;
#12186 = CARTESIAN_POINT ( 'NONE',  ( -1.091055626815042201, 3.346456692913386100, 0.3149606299212580063 ) ) ;
#12187 = DIRECTION ( 'NONE',  ( -3.469446951953613696E-16, 0.000000000000000000, -1.000000000000000000 ) ) ;
#12188 = EDGE_CURVE ( 'NONE', #32849, #40833, #35526, .T. ) ;
#12189 = EDGE_CURVE ( 'NONE', #31898, #27834, #41173, .T. ) ;
#12190 = VECTOR ( 'NONE', #20341, 39.37007874015748143 ) ;
#12191 = ORIENTED_EDGE ( 'NONE', *, *, #48460, .T. ) ;
#12192 = ORIENTED_EDGE ( 'NONE', *, *, #3396, .F. ) ;
#12193 = VERTEX_POINT ( 'NONE', #33687 ) ;
#12194 = LINE ( 'NONE', #8319, #38119 ) ;
#12195 = LINE ( 'NONE', #19416, #1573 ) ;
#12196 = EDGE_LOOP ( 'NONE', ( #41789, #2823, #30735, #35585 ) ) ;
#12197 = ORIENTED_EDGE ( 'NONE', *, *, #1824, .F. ) ;
#12198 = EDGE_CURVE ( 'NONE', #10769, #34717, #25408, .T. ) ;
#12199 = CARTESIAN_POINT ( 'NONE',  ( -1.236813753895212642, 1.541669022091038732, -2.681693691597581974 ) ) ;
#12200 = DIRECTION ( 'NONE',  ( -0.000000000000000000, 1.000000000000000000, -0.000000000000000000 ) ) ;
#12201 = CARTESIAN_POINT ( 'NONE',  ( -2.748374859398606596, 2.755905511811027164, -0.3226306186023588096 ) ) ;
#12202 = VECTOR ( 'NONE', #18146, 39.37007874015748854 ) ;
#12203 = ORIENTED_EDGE ( 'NONE', *, *, #22125, .T. ) ;
#12204 = VERTEX_POINT ( 'NONE', #29796 ) ;
#12205 = DIRECTION ( 'NONE',  ( 0.000000000000000000, 0.000000000000000000, -1.000000000000000000 ) ) ;
#12206 = CARTESIAN_POINT ( 'NONE',  ( -1.022351642223462997E-16, 0.000000000000000000, -9.058396573151636093E-17 ) ) ;
#12207 = LINE ( 'NONE', #328, #31131 ) ;
#12208 = EDGE_LOOP ( 'NONE', ( #4469, #33411, #9150, #12898 ) ) ;
#12209 = LINE ( 'NONE', #24597, #38904 ) ;
#12210 = FACE_OUTER_BOUND ( 'NONE', #34318, .T. ) ;
#12211 = VERTEX_POINT ( 'NONE', #33933 ) ;
#12212 = CARTESIAN_POINT ( 'NONE',  ( -1.166969139818015533, 3.346456692913386100, 1.417322834645662777 ) ) ;
#12213 = EDGE_LOOP ( 'NONE', ( #45185, #44678, #9, #31961 ) ) ;
#12214 = ORIENTED_EDGE ( 'NONE', *, *, #46265, .F. ) ;
#12215 = LINE ( 'NONE', #42438, #17179 ) ;
#12216 = DIRECTION ( 'NONE',  ( -0.000000000000000000, 1.000000000000000000, -0.000000000000000000 ) ) ;
#12217 = EDGE_CURVE ( 'NONE', #19764, #13466, #17413, .T. ) ;
#12218 = CARTESIAN_POINT ( 'NONE',  ( -0.3486774197067334380, 3.267716535433071279, 1.259842519685033357 ) ) ;
#12219 = AXIS2_PLACEMENT_3D ( 'NONE', #7550, #43152, #39294 ) ;
#12220 = LINE ( 'NONE', #3712, #7988 ) ;
#12221 = EDGE_CURVE ( 'NONE', #35595, #26317, #17672, .T. ) ;
#12222 = DIRECTION ( 'NONE',  ( -1.000000000000000000, 0.000000000000000000, -0.000000000000000000 ) ) ;
#12223 = ORIENTED_EDGE ( 'NONE', *, *, #857, .T. ) ;
#12224 = EDGE_LOOP ( 'NONE', ( #13540, #7611, #12971, #37694 ) ) ;
#12225 = EDGE_CURVE ( 'NONE', #5907, #48573, #31229, .T. ) ;
#12226 = ORIENTED_EDGE ( 'NONE', *, *, #31613, .F. ) ;
#12227 = CARTESIAN_POINT ( 'NONE',  ( -1.863748091109392213, 3.346456692913386100, -1.102362204724405492 ) ) ;
#12228 = CYLINDRICAL_SURFACE ( 'NONE', #1214, 2.165354330708661568 ) ;
#12229 = AXIS2_PLACEMENT_3D ( 'NONE', #48106, #8906, #40663 ) ;
#12230 = VECTOR ( 'NONE', #46195, 39.37007874015748143 ) ;
#12231 = VECTOR ( 'NONE', #38143, 39.37007874015748143 ) ;
#12232 = FACE_OUTER_BOUND ( 'NONE', #25481, .T. ) ;
#12233 = CARTESIAN_POINT ( 'NONE',  ( -0.04921259842519689481, 0.000000000000000000, 2.952755905511811108 ) ) ;
#12234 = ORIENTED_EDGE ( 'NONE', *, *, #34303, .F. ) ;
#12235 = CARTESIAN_POINT ( 'NONE',  ( 1.287906020515829919, 3.346456692913386100, -2.086614173228339641 ) ) ;
#12236 = VECTOR ( 'NONE', #22598, 39.37007874015748143 ) ;
#12237 = DIRECTION ( 'NONE',  ( -3.986037398843765983E-20, -1.000000000000000000, -1.160734090543304660E-16 ) ) ;
#12238 = ORIENTED_EDGE ( 'NONE', *, *, #18847, .T. ) ;
#12239 = DIRECTION ( 'NONE',  ( 0.000000000000000000, 0.000000000000000000, -1.000000000000000000 ) ) ;
#12240 = CARTESIAN_POINT ( 'NONE',  ( -1.195183497228115035E-16, 0.000000000000000000, -0.3149606299212591165 ) ) ;
#12241 = CARTESIAN_POINT ( 'NONE',  ( -2.162130742952123263, 3.267716535433071279, 0.1181102362204704270 ) ) ;
#12242 = ORIENTED_EDGE ( 'NONE', *, *, #37118, .F. ) ;
#12243 = PLANE ( 'NONE',  #32528 ) ;
#12244 = DIRECTION ( 'NONE',  ( -3.986037398843765983E-20, -1.000000000000000000, -1.160734090543304660E-16 ) ) ;
#12245 = DIRECTION ( 'NONE',  ( -1.000000000000000000, -0.000000000000000000, -0.000000000000000000 ) ) ;
#12246 = ORIENTED_EDGE ( 'NONE', *, *, #20394, .F. ) ;
#12247 = FACE_OUTER_BOUND ( 'NONE', #25596, .T. ) ;
#12248 = CARTESIAN_POINT ( 'NONE',  ( 0.2810212964504857913, 1.625182864229780533, -2.939398504922494215 ) ) ;
#12249 = EDGE_LOOP ( 'NONE', ( #24818, #22490, #42629, #40012 ) ) ;
#12250 = DIRECTION ( 'NONE',  ( -1.000000000000000000, 0.000000000000000000, 1.734723475976806848E-16 ) ) ;
#12251 = FACE_OUTER_BOUND ( 'NONE', #29595, .T. ) ;
#12252 = DIRECTION ( 'NONE',  ( 0.01601477604151182663, -0.9998717552508123996, 0.000000000000000000 ) ) ;
#12253 = DIRECTION ( 'NONE',  ( 0.000000000000000000, 1.000000000000000000, 0.000000000000000000 ) ) ;
#12254 = EDGE_CURVE ( 'NONE', #6843, #20840, #1920, .T. ) ;
#12255 = VECTOR ( 'NONE', #20519, 39.37007874015748143 ) ;
#12256 = EDGE_CURVE ( 'NONE', #27951, #42606, #11242, .T. ) ;
#12257 = EDGE_CURVE ( 'NONE', #38943, #41081, #41671, .T. ) ;
#12258 = ORIENTED_EDGE ( 'NONE', *, *, #41598, .T. ) ;
#12259 = VERTEX_POINT ( 'NONE', #9416 ) ;
#12260 = CARTESIAN_POINT ( 'NONE',  ( 1.556712866041120469, 1.205361022782829114E-17, 2.509548638715870084 ) ) ;
#12261 = B_SPLINE_CURVE_WITH_KNOTS ( 'NONE', 3,
 ( #3042, #49726, #38418, #34544 ),
 .UNSPECIFIED., .F., .F.,
 ( 4, 4 ),
 ( 0.01088822282284627151, 0.03073585682641423455 ),
 .UNSPECIFIED. ) ;
#12262 = DIRECTION ( 'NONE',  ( 0.000000000000000000, 0.000000000000000000, -1.000000000000000000 ) ) ;
#12263 = ORIENTED_EDGE ( 'NONE', *, *, #15016, .T. ) ;
#12264 = CARTESIAN_POINT ( 'NONE',  ( 1.810607833951273227, 0.05691986357332023266, -0.7203715021987137090 ) ) ;
#12265 = DIRECTION ( 'NONE',  ( -1.267583980596140612E-16, 1.000000000000000000, 2.300325776299552367E-17 ) ) ;
#12266 = DIRECTION ( 'NONE',  ( 1.000000000000000000, 0.000000000000000000, 0.000000000000000000 ) ) ;
#12267 = FACE_OUTER_BOUND ( 'NONE', #18013, .T. ) ;
#12268 = CIRCLE ( 'NONE', #41133, 2.106299212598425008 ) ;
#12269 = AXIS2_PLACEMENT_3D ( 'NONE', #22929, #38683, #35060 ) ;
#12270 = ORIENTED_EDGE ( 'NONE', *, *, #21384, .T. ) ;
#12271 = EDGE_LOOP ( 'NONE', ( #5084, #28437, #36916, #22743 ) ) ;
#12272 = B_SPLINE_CURVE_WITH_KNOTS ( 'NONE', 3,
 ( #31692, #38928, #7435, #3304 ),
 .UNSPECIFIED., .F., .F.,
 ( 4, 4 ),
 ( 0.1211873102087489551, 0.1625992483279400103 ),
 .UNSPECIFIED. ) ;
#12273 = LINE ( 'NONE', #8650, #40279 ) ;
#12274 = CARTESIAN_POINT ( 'NONE',  ( -2.044241703397525978, 5.905511811023623991, -0.7159595814952903758 ) ) ;
#12275 = DIRECTION ( 'NONE',  ( -1.000000000000000000, 0.000000000000000000, 1.734723475976806848E-16 ) ) ;
#12276 = COLOUR_RGB ( '',0.7921568627450980005, 0.8196078431372548767, 0.9333333333333333481 ) ;
#12277 = DIRECTION ( 'NONE',  ( -3.469446951953613696E-16, 0.000000000000000000, -1.000000000000000000 ) ) ;
#12278 = FACE_BOUND ( 'NONE', #7236, .T. ) ;
#12279 = ORIENTED_EDGE ( 'NONE', *, *, #14913, .F. ) ;
#12280 = LINE ( 'NONE', #15638, #49593 ) ;
#12281 = ORIENTED_EDGE ( 'NONE', *, *, #21643, .F. ) ;
#12282 = ORIENTED_EDGE ( 'NONE', *, *, #36420, .F. ) ;
#12283 = EDGE_CURVE ( 'NONE', #43980, #25798, #49120, .T. ) ;
#12284 = VECTOR ( 'NONE', #46989, 39.37007874015748143 ) ;
#12285 = LINE ( 'NONE', #32426, #27507 ) ;
#12286 = EDGE_CURVE ( 'NONE', #45498, #24717, #1663, .T. ) ;
#12287 = EDGE_LOOP ( 'NONE', ( #49488, #48853, #9894, #26991 ) ) ;
#12288 = ORIENTED_EDGE ( 'NONE', *, *, #13617, .T. ) ;
#12289 = CARTESIAN_POINT ( 'NONE',  ( 0.1968503937007878568, 0.000000000000000000, 1.574803149606291974 ) ) ;
#12290 = ADVANCED_FACE ( 'NONE', ( #45261 ), #5539, .T. ) ;
#12291 = EDGE_LOOP ( 'NONE', ( #33954, #2964, #12165, #33315 ) ) ;
#12292 = EDGE_CURVE ( 'NONE', #7345, #35180, #37810, .T. ) ;
#12293 = FACE_OUTER_BOUND ( 'NONE', #19503, .T. ) ;
#12294 = CARTESIAN_POINT ( 'NONE',  ( 2.134236802639954522, 5.905511811023623991, -2.040539317874580760 ) ) ;
#12295 = DIRECTION ( 'NONE',  ( -0.000000000000000000, 1.000000000000000000, -0.000000000000000000 ) ) ;
#12296 = AXIS2_PLACEMENT_3D ( 'NONE', #16068, #19169, #11436 ) ;
#12297 = DIRECTION ( 'NONE',  ( -1.000000000000000000, 0.000000000000000000, 0.000000000000000000 ) ) ;
#12298 = DIRECTION ( 'NONE',  ( -0.000000000000000000, 1.000000000000000000, -0.000000000000000000 ) ) ;
#12299 = CARTESIAN_POINT ( 'NONE',  ( -1.091055626815042645, 3.267716535433071279, -1.259842519685034690 ) ) ;
#12300 = VERTEX_POINT ( 'NONE', #9926 ) ;
#12301 = CARTESIAN_POINT ( 'NONE',  ( -1.909347346926324462, 3.267716535433071279, -0.03937007874015881204 ) ) ;
#12302 = FACE_OUTER_BOUND ( 'NONE', #37570, .T. ) ;
#12303 = PLANE ( 'NONE',  #24007 ) ;
#12304 = VECTOR ( 'NONE', #32883, 39.37007874015748143 ) ;
#12305 = EDGE_LOOP ( 'NONE', ( #27322, #24986, #27892, #42989 ) ) ;
#12306 = LINE ( 'NONE', #40448, #50358 ) ;
#12307 = CARTESIAN_POINT ( 'NONE',  ( 3.927031490892378253E-16, 3.346456692913386100, 2.007874015748021268 ) ) ;
#12308 = ORIENTED_EDGE ( 'NONE', *, *, #24812, .T. ) ;
#12309 = FACE_OUTER_BOUND ( 'NONE', #22995, .T. ) ;
#12310 = CARTESIAN_POINT ( 'NONE',  ( 1.919085105436704630, 0.01897331389017133801, -0.7667369131541573735 ) ) ;
#12311 = AXIS2_PLACEMENT_3D ( 'NONE', #13529, #17907, #45001 ) ;
#12312 = DIRECTION ( 'NONE',  ( 0.000000000000000000, 0.000000000000000000, -1.000000000000000000 ) ) ;
#12313 = CARTESIAN_POINT ( 'NONE',  ( -1.494044303739022972, 0.003989811691878806209, -0.9272426299426647089 ) ) ;
#12314 = VECTOR ( 'NONE', #48849, 39.37007874015748143 ) ;
#12315 = ORIENTED_EDGE ( 'NONE', *, *, #9329, .F. ) ;
#12316 = CARTESIAN_POINT ( 'NONE',  ( -1.909347346926324462, 3.346456692913386100, 1.102362204724404160 ) ) ;
#12317 = FACE_OUTER_BOUND ( 'NONE', #1832, .T. ) ;
#12318 = LINE ( 'NONE', #27794, #23458 ) ;
#12319 = DIRECTION ( 'NONE',  ( 1.734723475976806848E-16, -0.000000000000000000, 1.000000000000000000 ) ) ;
#12320 = EDGE_CURVE ( 'NONE', #37743, #27124, #25665, .T. ) ;
#12321 = ORIENTED_EDGE ( 'NONE', *, *, #6694, .F. ) ;
#12322 = ORIENTED_EDGE ( 'NONE', *, *, #9372, .F. ) ;
#12323 = EDGE_CURVE ( 'NONE', #39537, #5174, #22811, .T. ) ;
#12324 = LINE ( 'NONE', #16197, #19640 ) ;
#12325 = ORIENTED_EDGE ( 'NONE', *, *, #7438, .T. ) ;
#12326 = CARTESIAN_POINT ( 'NONE',  ( 2.165460538733997353, 0.000000000000000000, 0.04798874274655835076 ) ) ;
#12327 = VERTEX_POINT ( 'NONE', #42915 ) ;
#12328 = EDGE_CURVE ( 'NONE', #17781, #33327, #47011, .T. ) ;
#12329 = CARTESIAN_POINT ( 'NONE',  ( 0.7759887336347247588, 0.04034854520891290042, -1.724780676950718794 ) ) ;
#12330 = VECTOR ( 'NONE', #4134, 39.37007874015748143 ) ;
#12331 = ORIENTED_EDGE ( 'NONE', *, *, #12098, .F. ) ;
#12332 = DIRECTION ( 'NONE',  ( 1.734723475976806848E-16, -0.000000000000000000, 1.000000000000000000 ) ) ;
#12333 = B_SPLINE_CURVE_WITH_KNOTS ( 'NONE', 3,
 ( #35995, #40631, #43971, #39607 ),
 .UNSPECIFIED., .F., .F.,
 ( 4, 4 ),
 ( 0.01470896166604594366, 0.03075119253503404149 ),
 .UNSPECIFIED. ) ;
#12334 = LINE ( 'NONE', #34374, #38838 ) ;
#12335 = VERTEX_POINT ( 'NONE', #46024 ) ;
#12336 = DIRECTION ( 'NONE',  ( 1.734723475976806848E-16, -0.000000000000000000, 1.000000000000000000 ) ) ;
#12337 = ORIENTED_EDGE ( 'NONE', *, *, #23854, .F. ) ;
#12338 = VECTOR ( 'NONE', #2637, 39.37007874015748143 ) ;
#12339 = PLANE ( 'NONE',  #49294 ) ;
#12340 = EDGE_CURVE ( 'NONE', #24, #19538, #10684, .T. ) ;
#12341 = ORIENTED_EDGE ( 'NONE', *, *, #8590, .F. ) ;
#12342 = EDGE_LOOP ( 'NONE', ( #36452, #8552, #38031, #3432 ) ) ;
#12343 = PLANE ( 'NONE',  #4218 ) ;
#12344 = CARTESIAN_POINT ( 'NONE',  ( -1.843283979527560623, 1.678378384481335139, -1.157773721536293765 ) ) ;
#12345 = EDGE_CURVE ( 'NONE', #38409, #40420, #34936, .T. ) ;
#12346 = ORIENTED_EDGE ( 'NONE', *, *, #12547, .F. ) ;
#12347 = CIRCLE ( 'NONE', #16480, 2.106299212598425008 ) ;
#12348 = DIRECTION ( 'NONE',  ( -0.9998717552508122886, -0.01601477604151181275, 0.000000000000000000 ) ) ;
#12349 = VERTEX_POINT ( 'NONE', #18935 ) ;
#12350 = CARTESIAN_POINT ( 'NONE',  ( 2.592410251778310748, 1.661176152998282918, 1.413663899107065580 ) ) ;
#12351 = DIRECTION ( 'NONE',  ( -1.000000000000000000, 0.000000000000000000, -0.000000000000000000 ) ) ;
#12352 = CARTESIAN_POINT ( 'NONE',  ( 0.7423782071083092626, 3.267716535433071279, 1.889763779527550369 ) ) ;
#12353 = EDGE_LOOP ( 'NONE', ( #2815, #38020, #45920, #1815 ) ) ;
#12354 = ORIENTED_EDGE ( 'NONE', *, *, #24940, .F. ) ;
#12355 = DIRECTION ( 'NONE',  ( -3.469446951953613696E-16, 0.000000000000000000, -1.000000000000000000 ) ) ;
#12356 = CARTESIAN_POINT ( 'NONE',  ( -1.712496953225537188, 3.267716535433071279, 0.1574803149606286423 ) ) ;
#12357 = CARTESIAN_POINT ( 'NONE',  ( 1.979793062125284608, 1.750113821271474857, 2.191257344206569257 ) ) ;
#12358 = LINE ( 'NONE', #35095, #49032 ) ;
#12359 = CARTESIAN_POINT ( 'NONE',  ( -1.662150612268487704, 1.049866565877817237, -1.156143393213623360 ) ) ;
#12360 = DIRECTION ( 'NONE',  ( -0.9998717552508122886, -0.01601477604151180928, 0.000000000000000000 ) ) ;
#12361 = VECTOR ( 'NONE', #1673, 39.37007874015748143 ) ;
#12362 = ORIENTED_EDGE ( 'NONE', *, *, #26597, .T. ) ;
#12363 = PLANE ( 'NONE',  #11891 ) ;
#12364 = VERTEX_POINT ( 'NONE', #7567 ) ;
#12365 = FACE_OUTER_BOUND ( 'NONE', #26475, .T. ) ;
#12366 = EDGE_LOOP ( 'NONE', ( #34236, #35399, #16827, #8743 ) ) ;
#12367 = CARTESIAN_POINT ( 'NONE',  ( -1.684292108503797181, -1.610880632035666997E-16, 1.406123411605399998 ) ) ;
#12368 = AXIS2_PLACEMENT_3D ( 'NONE', #25750, #17254, #13373 ) ;
#12369 = DIRECTION ( 'NONE',  ( 0.01601477604151182663, -0.9998717552508123996, 0.000000000000000000 ) ) ;
#12370 = DIRECTION ( 'NONE',  ( 0.9998717552508121775, 0.01601477604151182663, 0.000000000000000000 ) ) ;
#12371 = ORIENTED_EDGE ( 'NONE', *, *, #42658, .F. ) ;
#12372 = LINE ( 'NONE', #28110, #44717 ) ;
#12373 = ADVANCED_FACE ( 'NONE', ( #11687 ), #26423, .F. ) ;
#12374 = DIRECTION ( 'NONE',  ( -1.000000000000000000, 0.000000000000000000, 1.734723475976806848E-16 ) ) ;
#12375 = EDGE_CURVE ( 'NONE', #25092, #20098, #47176, .T. ) ;
#12376 = ORIENTED_EDGE ( 'NONE', *, *, #41523, .T. ) ;
#12377 = DIRECTION ( 'NONE',  ( -0.000000000000000000, 0.000000000000000000, 1.000000000000000000 ) ) ;
#12378 = VECTOR ( 'NONE', #18167, 39.37007874015748143 ) ;
#12379 = ORIENTED_EDGE ( 'NONE', *, *, #7911, .T. ) ;
#12380 = ADVANCED_FACE ( 'NONE', ( #11440 ), #46767, .F. ) ;
#12381 = FACE_OUTER_BOUND ( 'NONE', #17450, .T. ) ;
#12382 = CARTESIAN_POINT ( 'NONE',  ( 2.867773316779195447, 1.449472587384593725, -0.7050287376752005786 ) ) ;
#12383 = EDGE_CURVE ( 'NONE', #20489, #28082, #19420, .T. ) ;
#12384 = EDGE_CURVE ( 'NONE', #40028, #11918, #15312, .T. ) ;
#12385 = PLANE ( 'NONE',  #43631 ) ;
#12386 = ORIENTED_EDGE ( 'NONE', *, *, #43057, .T. ) ;
#12387 = ORIENTED_EDGE ( 'NONE', *, *, #9344, .F. ) ;
#12388 = DIRECTION ( 'NONE',  ( 0.000000000000000000, 0.000000000000000000, 1.000000000000000000 ) ) ;
#12389 = LINE ( 'NONE', #35127, #14119 ) ;
#12390 = FACE_BOUND ( 'NONE', #9398, .T. ) ;
#12391 = CARTESIAN_POINT ( 'NONE',  ( 1.363819533518803251, 3.267716535433071279, 1.220472440944875281 ) ) ;
#12392 = EDGE_CURVE ( 'NONE', #31330, #11733, #38562, .T. ) ;
#12393 = DIRECTION ( 'NONE',  ( -1.000000000000000000, -0.000000000000000000, -0.000000000000000000 ) ) ;
#12394 = EDGE_LOOP ( 'NONE', ( #21395, #45726, #8065, #16723 ) ) ;
#12395 = DIRECTION ( 'NONE',  ( 1.000000000000000000, 0.000000000000000000, 0.000000000000000000 ) ) ;
#12396 = EDGE_CURVE ( 'NONE', #37702, #25844, #27174, .T. ) ;
#12397 = VERTEX_POINT ( 'NONE', #23303 ) ;
#12398 = VERTEX_POINT ( 'NONE', #2679 ) ;
#12399 = ITEM_DEFINED_TRANSFORMATION ( 'NONE', 'NONE', #11881,  #26741 ) ;
#12400 = ORIENTED_EDGE ( 'NONE', *, *, #35119, .T. ) ;
#12401 = LINE ( 'NONE', #16021, #18550 ) ;
#12402 = AXIS2_PLACEMENT_3D ( 'NONE', #32183, #15901, #11774 ) ;
#12403 = FACE_OUTER_BOUND ( 'NONE', #34330, .T. ) ;
#12404 = AXIS2_PLACEMENT_3D ( 'NONE', #7424, #30665, #7173 ) ;
#12405 = EDGE_CURVE ( 'NONE', #46197, #47793, #15852, .T. ) ;
#12406 = CARTESIAN_POINT ( 'NONE',  ( 0.8182917201112819283, 0.000000000000000000, -0.7874015748031473194 ) ) ;
#12407 = CARTESIAN_POINT ( 'NONE',  ( -0.6214413264104945434, 3.346456692913386100, 2.012537465693970962 ) ) ;
#12408 = ORIENTED_EDGE ( 'NONE', *, *, #11840, .T. ) ;
#12409 = ORIENTED_EDGE ( 'NONE', *, *, #12975, .T. ) ;
#12410 = CARTESIAN_POINT ( 'NONE',  ( -1.528806138047155150, 0.001175590193779177828, 0.8785712512199921331 ) ) ;
#12411 = FILL_AREA_STYLE ('',( #39523 ) ) ;
#12412 = DIRECTION ( 'NONE',  ( -0.000000000000000000, 1.000000000000000000, -0.000000000000000000 ) ) ;
#12413 = AXIS2_PLACEMENT_3D ( 'NONE', #40526, #5665, #29411 ) ;
#12414 = ORIENTED_EDGE ( 'NONE', *, *, #23383, .F. ) ;
#12415 = EDGE_CURVE ( 'NONE', #21582, #2475, #38063, .T. ) ;
#12416 = DIRECTION ( 'NONE',  ( -0.01601477604151182663, 0.9998717552508123996, -0.000000000000000000 ) ) ;
#12417 = CARTESIAN_POINT ( 'NONE',  ( -0.9914495361339012991, 5.905511811023623991, 2.781765111341808705 ) ) ;
#12418 = CARTESIAN_POINT ( 'NONE',  ( 1.909347346926324462, 3.346456692913386100, -1.102362204724406602 ) ) ;
#12419 = CARTESIAN_POINT ( 'NONE',  ( -1.363819533518803473, 3.267716535433071279, -1.929133858267710000 ) ) ;
#12420 = FACE_OUTER_BOUND ( 'NONE', #38415, .T. ) ;
#12421 = EDGE_LOOP ( 'NONE', ( #16844, #47666, #3264, #46319 ) ) ;
#12422 = CARTESIAN_POINT ( 'NONE',  ( -2.100227814008681637, 1.559371130916006543, -2.076109931251943319 ) ) ;
#12423 = CARTESIAN_POINT ( 'NONE',  ( -2.949782676795219771, 5.905511811023623991, -0.1324748927672787513 ) ) ;
#12424 = ORIENTED_EDGE ( 'NONE', *, *, #14378, .T. ) ;
#12425 = ORIENTED_EDGE ( 'NONE', *, *, #4619, .T. ) ;
#12426 = DIRECTION ( 'NONE',  ( -3.469446951953613696E-16, 0.000000000000000000, -1.000000000000000000 ) ) ;
#12427 = PLANE ( 'NONE',  #3084 ) ;
#12428 = CYLINDRICAL_SURFACE ( 'NONE', #13173, 2.165354330708661568 ) ;
#12429 = VERTEX_POINT ( 'NONE', #50369 ) ;
#12430 = ORIENTED_EDGE ( 'NONE', *, *, #3487, .T. ) ;
#12431 = FACE_OUTER_BOUND ( 'NONE', #35641, .T. ) ;
#12432 = VERTEX_POINT ( 'NONE', #15061 ) ;
#12433 = LINE ( 'NONE', #45381, #22944 ) ;
#12434 = ORIENTED_EDGE ( 'NONE', *, *, #49454, .T. ) ;
#12435 = ADVANCED_FACE ( 'NONE', ( #42671 ), #30808, .F. ) ;
#12436 = VECTOR ( 'NONE', #49020, 39.37007874015748143 ) ;
#12437 = DIRECTION ( 'NONE',  ( -0.01601477604151182663, 0.9998717552508123996, -0.000000000000000000 ) ) ;
#12438 = DIRECTION ( 'NONE',  ( -0.9998717552508122886, -0.01601477604151181275, 0.000000000000000000 ) ) ;
#12439 = DIRECTION ( 'NONE',  ( 0.000000000000000000, 1.000000000000000000, 0.000000000000000000 ) ) ;
#12440 = VECTOR ( 'NONE', #41740, 39.37007874015748143 ) ;
#12441 = EDGE_CURVE ( 'NONE', #45936, #16745, #7319, .T. ) ;
#12442 = ORIENTED_EDGE ( 'NONE', *, *, #17010, .F. ) ;
#12443 = ORIENTED_EDGE ( 'NONE', *, *, #41761, .T. ) ;
#12444 = VERTEX_POINT ( 'NONE', #38812 ) ;
#12445 = DIRECTION ( 'NONE',  ( 1.734723475976806848E-16, -0.000000000000000000, 1.000000000000000000 ) ) ;
#12446 = VERTEX_POINT ( 'NONE', #3440 ) ;
#12447 = ORIENTED_EDGE ( 'NONE', *, *, #6590, .F. ) ;
#12448 = CARTESIAN_POINT ( 'NONE',  ( 2.106197740627112402, 0.000000000000000000, 0.7874015748031456541 ) ) ;
#12449 = LINE ( 'NONE', #32343, #16174 ) ;
#12450 = AXIS2_PLACEMENT_3D ( 'NONE', #29613, #22617, #33753 ) ;
#12451 = LINE ( 'NONE', #24073, #551 ) ;
#12452 = AXIS2_PLACEMENT_3D ( 'NONE', #33974, #34978, #23095 ) ;
#12453 = ORIENTED_EDGE ( 'NONE', *, *, #9049, .T. ) ;
#12454 = DIRECTION ( 'NONE',  ( -3.986037398843765983E-20, -1.000000000000000000, -1.160734090543304660E-16 ) ) ;
#12455 = LINE ( 'NONE', #8842, #37381 ) ;
#12456 = LINE ( 'NONE', #20458, #44314 ) ;
#12457 = VERTEX_POINT ( 'NONE', #20188 ) ;
#12458 = CARTESIAN_POINT ( 'NONE',  ( -1.195183497228115035E-16, 3.346456692913386100, -0.3149606299212591165 ) ) ;
#12459 = PLANE ( 'NONE',  #15332 ) ;
#12460 = VERTEX_POINT ( 'NONE', #12711 ) ;
#12461 = LINE ( 'NONE', #43944, #6003 ) ;
#12462 = VERTEX_POINT ( 'NONE', #43427 ) ;
#12463 = ORIENTED_EDGE ( 'NONE', *, *, #43148, .F. ) ;
#12464 = PLANE ( 'NONE',  #6451 ) ;
#12465 =( LENGTH_UNIT ( ) NAMED_UNIT ( * ) SI_UNIT ( $, .METRE. ) );
#12466 = DIRECTION ( 'NONE',  ( -0.000000000000000000, 1.000000000000000000, -0.000000000000000000 ) ) ;
#12467 = EDGE_CURVE ( 'NONE', #13176, #18622, #835, .T. ) ;
#12468 = DIRECTION ( 'NONE',  ( 1.734723475976806848E-16, -0.000000000000000000, 1.000000000000000000 ) ) ;
#12469 = LINE ( 'NONE', #28210, #768 ) ;
#12470 = ORIENTED_EDGE ( 'NONE', *, *, #48415, .T. ) ;
#12471 = ORIENTED_EDGE ( 'NONE', *, *, #39068, .F. ) ;
#12472 = PRODUCT_DEFINITION_SHAPE ( 'NONE', 'NONE',  #51059 ) ;
#12473 = ORIENTED_EDGE ( 'NONE', *, *, #12286, .T. ) ;
#12474 = FACE_OUTER_BOUND ( 'NONE', #26682, .T. ) ;
#12475 = EDGE_CURVE ( 'NONE', #4264, #29976, #4961, .T. ) ;
#12476 = CARTESIAN_POINT ( 'NONE',  ( 0.000000000000000000, 2.755905511811023612, 0.000000000000000000 ) ) ;
#12477 = AXIS2_PLACEMENT_3D ( 'NONE', #46118, #38657, #3280 ) ;
#12478 = ADVANCED_FACE ( 'NONE', ( #24333 ), #20704, .F. ) ;
#12479 = LINE ( 'NONE', #46613, #32448 ) ;
#12480 = DIRECTION ( 'NONE',  ( -1.000000000000000000, 0.000000000000000000, -0.000000000000000000 ) ) ;
#12482 = CARTESIAN_POINT ( 'NONE',  ( -1.166969139818015755, 3.267716535433071279, 4.048737525165545662E-16 ) ) ;
#12481 = VECTOR ( 'NONE', #11745, 39.37007874015748143 ) ;
#12483 = ORIENTED_EDGE ( 'NONE', *, *, #14666, .F. ) ;
#12484 = DIRECTION ( 'NONE',  ( 1.734723475976806848E-16, 0.000000000000000000, 1.000000000000000000 ) ) ;
#12485 = ADVANCED_FACE ( 'NONE', ( #582 ), #39566, .F. ) ;
#12486 = VECTOR ( 'NONE', #1156, 39.37007874015748143 ) ;
#12487 = CARTESIAN_POINT ( 'NONE',  ( 0.07982360342473591996, 1.709180471932028711, 0.000000000000000000 ) ) ;
#12488 = EDGE_CURVE ( 'NONE', #46309, #5934, #48195, .T. ) ;
#12489 = ORIENTED_EDGE ( 'NONE', *, *, #47270, .T. ) ;
#12490 = AXIS2_PLACEMENT_3D ( 'NONE', #620, #43970, #8621 ) ;
#12491 = FACE_OUTER_BOUND ( 'NONE', #16245, .T. ) ;
#12492 = DIRECTION ( 'NONE',  ( -0.000000000000000000, 1.000000000000000000, -0.000000000000000000 ) ) ;
#12493 = LINE ( 'NONE', #28746, #29610 ) ;
#12494 = ORIENTED_EDGE ( 'NONE', *, *, #49137, .T. ) ;
#12495 = FACE_OUTER_BOUND ( 'NONE', #22618, .T. ) ;
#12496 = CARTESIAN_POINT ( 'NONE',  ( -1.062992125984251413, 0.000000000000000000, -1.181102362204724754 ) ) ;
#12497 = CARTESIAN_POINT ( 'NONE',  ( 2.378961647330872786, 3.346456692913386100, 0.4330708661417287386 ) ) ;
#12498 = ORIENTED_EDGE ( 'NONE', *, *, #34634, .F. ) ;
#12499 = DIRECTION ( 'NONE',  ( 1.000000000000000000, 0.000000000000000000, 0.000000000000000000 ) ) ;
#12500 = PLANE ( 'NONE',  #13047 ) ;
#12501 = EDGE_LOOP ( 'NONE', ( #7545, #44610, #44935, #25472 ) ) ;
#12502 = DIRECTION ( 'NONE',  ( 1.734723475976806848E-16, -0.000000000000000000, 1.000000000000000000 ) ) ;
#12503 = EDGE_CURVE ( 'NONE', #35629, #29992, #24589, .T. ) ;
#12504 = CARTESIAN_POINT ( 'NONE',  ( 1.068075307999460488, 1.574803149606302854, 1.883606783264653028 ) ) ;
#12505 = FACE_OUTER_BOUND ( 'NONE', #48165, .T. ) ;
#12506 = LINE ( 'NONE', #1399, #13648 ) ;
#12507 = EDGE_CURVE ( 'NONE', #36108, #810, #37638, .T. ) ;
#12508 = EDGE_CURVE ( 'NONE', #5087, #46382, #12449, .T. ) ;
#12509 = EDGE_LOOP ( 'NONE', ( #15075, #258, #48530, #26905, #16322, #28394, #1268, #43993, #44119, #25667, #41061 ) ) ;
#12510 = ORIENTED_EDGE ( 'NONE', *, *, #13139, .F. ) ;
#12511 = CARTESIAN_POINT ( 'NONE',  ( 0.000000000000000000, 0.000000000000000000, 0.000000000000000000 ) ) ;
#12512 = CARTESIAN_POINT ( 'NONE',  ( -2.277873973731453727, 1.585326468414270495, 1.879489153247635214 ) ) ;
#12513 = ORIENTED_EDGE ( 'NONE', *, *, #42500, .T. ) ;
#12514 = LINE ( 'NONE', #36275, #1136 ) ;
#12515 = DIRECTION ( 'NONE',  ( -3.469446951953613696E-16, 0.000000000000000000, -1.000000000000000000 ) ) ;
#12516 = CARTESIAN_POINT ( 'NONE',  ( 0.07982360342473591996, 1.709180471932028711, 0.000000000000000000 ) ) ;
#12517 = VECTOR ( 'NONE', #44734, 39.37007874015748143 ) ;
#12518 = DIRECTION ( 'NONE',  ( 0.000000000000000000, -1.000000000000000000, 0.000000000000000000 ) ) ;
#12519 = ORIENTED_EDGE ( 'NONE', *, *, #5102, .T. ) ;
#12520 = VECTOR ( 'NONE', #42925, 39.37007874015748143 ) ;
#12521 = ORIENTED_EDGE ( 'NONE', *, *, #36117, .T. ) ;
#12522 = CARTESIAN_POINT ( 'NONE',  ( -1.001904449526793695, 1.691854617476330036, -1.967052558704270426 ) ) ;
#12523 = CARTESIAN_POINT ( 'NONE',  ( 4.268512490100411402E-16, 3.346456692913386100, 1.259842519685033357 ) ) ;
#12524 = CARTESIAN_POINT ( 'NONE',  ( -2.010517631316633747, 1.205361022782829114E-17, 0.8058170502102087740 ) ) ;
#12525 = LINE ( 'NONE', #13555, #6738 ) ;
#12526 = AXIS2_PLACEMENT_3D ( 'NONE', #42666, #34682, #18930 ) ;
#12527 = FACE_BOUND ( 'NONE', #11376, .T. ) ;
#12528 = ORIENTED_EDGE ( 'NONE', *, *, #13076, .F. ) ;
#12529 = DIRECTION ( 'NONE',  ( 0.000000000000000000, 1.000000000000000000, 0.000000000000000000 ) ) ;
#12530 = ORIENTED_EDGE ( 'NONE', *, *, #39249, .F. ) ;
#12531 = VECTOR ( 'NONE', #50496, 39.37007874015748143 ) ;
#12532 = ORIENTED_EDGE ( 'NONE', *, *, #12741, .T. ) ;
#12533 = DIRECTION ( 'NONE',  ( -1.000000000000000000, 0.000000000000000000, -0.000000000000000000 ) ) ;
#12534 = VECTOR ( 'NONE', #21339, 39.37007874015748143 ) ;
#12535 = EDGE_LOOP ( 'NONE', ( #29432, #21468, #44168, #9414 ) ) ;
#12537 = ORIENTED_EDGE ( 'NONE', *, *, #16310, .F. ) ;
#12536 = EDGE_CURVE ( 'NONE', #5596, #18938, #1084, .T. ) ;
#12538 = DIRECTION ( 'NONE',  ( -1.000000000000000000, 0.000000000000000000, 0.000000000000000000 ) ) ;
#12539 = ORIENTED_EDGE ( 'NONE', *, *, #15237, .F. ) ;
#12540 = LINE ( 'NONE', #28281, #32854 ) ;
#12541 = DIRECTION ( 'NONE',  ( 0.000000000000000000, -0.000000000000000000, 1.000000000000000000 ) ) ;
#12542 = EDGE_CURVE ( 'NONE', #31043, #2822, #1359, .T. ) ;
#12543 = DIRECTION ( 'NONE',  ( -0.5407162030609375947, -0.6444004775717706579, 0.5407162030609372616 ) ) ;
#12544 = EDGE_CURVE ( 'NONE', #22163, #37684, #16848, .T. ) ;
#12545 = EDGE_CURVE ( 'NONE', #41777, #7739, #8579, .T. ) ;
#12546 = PLANE ( 'NONE',  #48635 ) ;
#12547 = EDGE_CURVE ( 'NONE', #850, #10535, #8836, .T. ) ;
#12548 = CARTESIAN_POINT ( 'NONE',  ( -1.536664496436148184E-16, 0.000000000000000000, -1.771653543307081025 ) ) ;
#12549 = DIRECTION ( 'NONE',  ( 0.000000000000000000, 0.000000000000000000, -1.000000000000000000 ) ) ;
#12550 = ORIENTED_EDGE ( 'NONE', *, *, #10175, .T. ) ;
#12551 = PLANE ( 'NONE',  #24188 ) ;
#12552 = DIRECTION ( 'NONE',  ( -1.000000000000000000, -0.000000000000000000, -0.000000000000000000 ) ) ;
#12553 = CARTESIAN_POINT ( 'NONE',  ( -1.788632549858358844, 3.267716535433071279, 1.220472440944875059 ) ) ;
#12554 = ORIENTED_EDGE ( 'NONE', *, *, #46467, .F. ) ;
#12555 = VECTOR ( 'NONE', #15257, 39.37007874015748143 ) ;
#12556 = CARTESIAN_POINT ( 'NONE',  ( -0.8942052331142552601, 3.346456692913386100, 2.007874015748021268 ) ) ;
#12557 = CARTESIAN_POINT ( 'NONE',  ( -0.1516866087075746383, 1.607047215343822222, -2.234383150555500297 ) ) ;
#12558 = ORIENTED_EDGE ( 'NONE', *, *, #2216, .F. ) ;
#12559 = DIRECTION ( 'NONE',  ( -0.000000000000000000, 0.000000000000000000, 1.000000000000000000 ) ) ;
#12560 = ADVANCED_FACE ( 'NONE', ( #24072 ), #27678, .F. ) ;
#12561 = CARTESIAN_POINT ( 'NONE',  ( 1.109524193798303804, 0.000000000000000000, 1.344750771968474590 ) ) ;
#12562 = FACE_OUTER_BOUND ( 'NONE', #50828, .T. ) ;
#12563 = VECTOR ( 'NONE', #39381, 39.37007874015748143 ) ;
#12564 = ORIENTED_EDGE ( 'NONE', *, *, #10302, .F. ) ;
#12565 = CIRCLE ( 'NONE', #47120, 2.106299212598425008 ) ;
#12566 = CARTESIAN_POINT ( 'NONE',  ( 0.000000000000000000, 6.692913385826772199, 0.000000000000000000 ) ) ;
#12567 = EDGE_CURVE ( 'NONE', #31313, #32010, #23555, .T. ) ;
#12568 = ORIENTED_EDGE ( 'NONE', *, *, #4616, .F. ) ;
#12569 = DIRECTION ( 'NONE',  ( -0.000000000000000000, 1.000000000000000000, -0.000000000000000000 ) ) ;
#12570 = CARTESIAN_POINT ( 'NONE',  ( 1.695772546416037363, 1.647224322255602891, -2.417756147381349141 ) ) ;
#12571 = CIRCLE ( 'NONE', #35634, 2.106299212598425008 ) ;
#12572 = EDGE_CURVE ( 'NONE', #14807, #36871, #3947, .T. ) ;
#12573 = CARTESIAN_POINT ( 'NONE',  ( 0.07982360342473591996, 1.709180471932028711, 0.000000000000000000 ) ) ;
#12574 = CARTESIAN_POINT ( 'NONE',  ( -1.091055626815042423, 3.267716535433071279, 1.892679809432644143E-16 ) ) ;
#12575 = EDGE_CURVE ( 'NONE', #17653, #15706, #15808, .T. ) ;
#12576 = VERTEX_POINT ( 'NONE', #35955 ) ;
#12577 = ORIENTED_EDGE ( 'NONE', *, *, #49487, .T. ) ;
#12578 = CARTESIAN_POINT ( 'NONE',  ( 1.560669927219590303, 3.346456692913386100, -1.102362204724405714 ) ) ;
#12579 = ADVANCED_FACE ( 'NONE', ( #47777 ), #31568, .T. ) ;
#12580 = VERTEX_POINT ( 'NONE', #2110 ) ;
#12581 = CARTESIAN_POINT ( 'NONE',  ( 1.833433833923351353, 3.346456692913386100, -1.161035397307311917E-15 ) ) ;
#12582 = B_SPLINE_CURVE_WITH_KNOTS ( 'NONE', 3,
 ( #15455, #27060, #6950, #34075 ),
 .UNSPECIFIED., .F., .F.,
 ( 4, 4 ),
 ( 2.655830299951649833E-07, 0.01930353374404481653 ),
 .UNSPECIFIED. ) ;
#12583 = VERTEX_POINT ( 'NONE', #40847 ) ;
#12584 = DIRECTION ( 'NONE',  ( -3.469446951953613696E-16, 0.000000000000000000, -1.000000000000000000 ) ) ;
#12585 = ORIENTED_EDGE ( 'NONE', *, *, #39213, .F. ) ;
#12586 = CARTESIAN_POINT ( 'NONE',  ( -0.8942052331142547050, 0.000000000000000000, 1.062992125984246083 ) ) ;
#12587 = DIRECTION ( 'NONE',  ( -0.7071067811865483499, -1.442222014787672788E-15, -0.7071067811865465735 ) ) ;
#12588 = ORIENTED_EDGE ( 'NONE', *, *, #9203, .T. ) ;
#12589 = CARTESIAN_POINT ( 'NONE',  ( 0.8182917201112819283, 3.346456692913386100, 0.5905511811023579360 ) ) ;
#12590 = VERTEX_POINT ( 'NONE', #9346 ) ;
#12591 = AXIS2_PLACEMENT_3D ( 'NONE', #7958, #204, #15954 ) ;
#12592 = LINE ( 'NONE', #16732, #32025 ) ;
#12593 = VERTEX_POINT ( 'NONE', #1601 ) ;
#12594 = ORIENTED_EDGE ( 'NONE', *, *, #2268, .T. ) ;
#12595 = CARTESIAN_POINT ( 'NONE',  ( 2.151809081513405442, 6.692913385826772199, 0.2418202932658665705 ) ) ;
#12596 = VECTOR ( 'NONE', #16854, 39.37007874015748143 ) ;
#12597 = VERTEX_POINT ( 'NONE', #1855 ) ;
#12598 = VECTOR ( 'NONE', #39830, 39.37007874015748143 ) ;
#12599 = LINE ( 'NONE', #27826, #8101 ) ;
#12600 = VERTEX_POINT ( 'NONE', #5731 ) ;
#12601 = LINE ( 'NONE', #32235, #10427 ) ;
#12602 = VECTOR ( 'NONE', #18141, 39.37007874015748143 ) ;
#12603 = VECTOR ( 'NONE', #33161, 39.37007874015748143 ) ;
#12604 = CARTESIAN_POINT ( 'NONE',  ( 1.670330979180827180, 3.267716535433071279, 1.377952755905504256 ) ) ;
#12605 = EDGE_CURVE ( 'NONE', #21303, #209, #50244, .T. ) ;
#12606 = DIRECTION ( 'NONE',  ( 0.5508969814521065267, 0.000000000000000000, -0.8345732537212999791 ) ) ;
#12607 = VERTEX_POINT ( 'NONE', #41608 ) ;
#12608 = ORIENTED_EDGE ( 'NONE', *, *, #32146, .F. ) ;
#12609 = EDGE_CURVE ( 'NONE', #17641, #35680, #44451, .T. ) ;
#12610 = CARTESIAN_POINT ( 'NONE',  ( -0.5455278134075214336, 3.346456692913386100, -0.3149606299212593941 ) ) ;
#12611 = CARTESIAN_POINT ( 'NONE',  ( 2.009025172380753066, 0.000000000000000000, 0.7045170369349440520 ) ) ;
#12612 = VECTOR ( 'NONE', #46805, 39.37007874015748143 ) ;
#12613 = ADVANCED_FACE ( 'NONE', ( #49555 ), #37746, .T. ) ;
#12614 = LINE ( 'NONE', #16749, #31542 ) ;
#12615 = DIRECTION ( 'NONE',  ( -1.000000000000000000, 0.000000000000000000, -0.000000000000000000 ) ) ;
#12616 = DIRECTION ( 'NONE',  ( -0.000000000000000000, 1.000000000000000000, -0.000000000000000000 ) ) ;
#12617 = DIRECTION ( 'NONE',  ( -3.469446951953613696E-16, 0.000000000000000000, -1.000000000000000000 ) ) ;
#12618 = CARTESIAN_POINT ( 'NONE',  ( 0.4696143004045478797, 3.346456692913386100, -0.3543307086614173040 ) ) ;
#12619 = EDGE_LOOP ( 'NONE', ( #4486, #19424, #33652, #32685 ) ) ;
#12620 = DIRECTION ( 'NONE',  ( -0.000000000000000000, -1.000000000000000000, -0.000000000000000000 ) ) ;
#12621 = VERTEX_POINT ( 'NONE', #33621 ) ;
#12622 = CARTESIAN_POINT ( 'NONE',  ( -1.062992125984252079, 0.5905511811023621549, -1.181102362204724754 ) ) ;
#12623 = EDGE_CURVE ( 'NONE', #43507, #44778, #5474, .T. ) ;
#12624 = VERTEX_POINT ( 'NONE', #21990 ) ;
#12625 = PLANE ( 'NONE',  #24248 ) ;
#12626 = CARTESIAN_POINT ( 'NONE',  ( 1.909347346926324684, 0.000000000000000000, 0.7874015748031456541 ) ) ;
#12627 = EDGE_CURVE ( 'NONE', #15792, #17531, #28703, .T. ) ;
#12628 = LINE ( 'NONE', #32524, #16883 ) ;
#12629 = DIRECTION ( 'NONE',  ( 0.9749279121818259508, 0.000000000000000000, -0.2225209339563041788 ) ) ;
#12630 = ORIENTED_EDGE ( 'NONE', *, *, #33603, .F. ) ;
#12631 = PLANE ( 'NONE',  #7627 ) ;
#12632 = AXIS2_PLACEMENT_3D ( 'NONE', #24274, #4654, #32030 ) ;
#12633 = FACE_BOUND ( 'NONE', #4056, .T. ) ;
#12634 = ADVANCED_FACE ( 'NONE', ( #18114 ), #29216, .F. ) ;
#12635 = ORIENTED_EDGE ( 'NONE', *, *, #24287, .T. ) ;
#12636 = DIRECTION ( 'NONE',  ( -1.000000000000000000, 0.000000000000000000, 0.000000000000000000 ) ) ;
#12637 = VECTOR ( 'NONE', #17965, 39.37007874015748143 ) ;
#12638 = EDGE_CURVE ( 'NONE', #48286, #36377, #6309, .T. ) ;
#12639 = ORIENTED_EDGE ( 'NONE', *, *, #41193, .F. ) ;
#12640 = VECTOR ( 'NONE', #45213, 39.37007874015748143 ) ;
#12641 = VECTOR ( 'NONE', #4672, 39.37007874015748143 ) ;
#12642 = CARTESIAN_POINT ( 'NONE',  ( 1.604245399104406111, 0.5221609200332525402, -1.601902187605692918 ) ) ;
#12643 = CARTESIAN_POINT ( 'NONE',  ( 2.182111253630085290, 0.000000000000000000, -0.5118110236220471121 ) ) ;
#12644 = VECTOR ( 'NONE', #30845, 39.37007874015748143 ) ;
#12645 = DIRECTION ( 'NONE',  ( -0.9839295885986295565, 0.000000000000000000, -0.1785568947986370392 ) ) ;
#12646 = ORIENTED_EDGE ( 'NONE', *, *, #19116, .F. ) ;
#12647 = VERTEX_POINT ( 'NONE', #10112 ) ;
#12648 = CARTESIAN_POINT ( 'NONE',  ( 1.753307453716355324, 0.9966445008960358454, 1.932023706743397184 ) ) ;
#12649 = CARTESIAN_POINT ( 'NONE',  ( 1.833433833923351353, 3.346456692913386100, 1.574803149606291974 ) ) ;
#12650 = DIRECTION ( 'NONE',  ( 8.902872254219889125E-17, 1.000000000000000000, 9.311674343991287120E-17 ) ) ;
#12651 = DIRECTION ( 'NONE',  ( 1.734723475976806848E-16, -0.000000000000000000, 1.000000000000000000 ) ) ;
#12652 = DIRECTION ( 'NONE',  ( -1.598721155460225418E-14, 0.000000000000000000, 1.000000000000000000 ) ) ;
#12653 = ORIENTED_EDGE ( 'NONE', *, *, #31347, .T. ) ;
#12654 = CARTESIAN_POINT ( 'NONE',  ( -2.623503965249869729, 5.905511811023623991, 1.355882097269834663 ) ) ;
#12655 = ORIENTED_EDGE ( 'NONE', *, *, #12542, .T. ) ;
#12656 = ORIENTED_EDGE ( 'NONE', *, *, #45189, .F. ) ;
#12657 = EDGE_LOOP ( 'NONE', ( #2093, #9977, #1952, #28859 ) ) ;
#12658 = CARTESIAN_POINT ( 'NONE',  ( 2.170993901765784440, 1.749570721460282696, 1.668364588115243130 ) ) ;
#12659 = CARTESIAN_POINT ( 'NONE',  ( 1.636583440222563857, 0.000000000000000000, 1.259842519685033135 ) ) ;
#12660 = PLANE ( 'NONE',  #25058 ) ;
#12661 = CARTESIAN_POINT ( 'NONE',  ( 0.4349608091550758449, 6.692913385826772199, 2.121218629000301004 ) ) ;
#12662 = ORIENTED_EDGE ( 'NONE', *, *, #27640, .T. ) ;
#12663 = ORIENTED_EDGE ( 'NONE', *, *, #42008, .T. ) ;
#12664 = CIRCLE ( 'NONE', #274, 2.165354330708661568 ) ;
#12665 = ADVANCED_FACE ( 'NONE', ( #45198 ), #25854, .F. ) ;
#12666 = CARTESIAN_POINT ( 'NONE',  ( -0.5455278134075214336, 3.346456692913386100, -1.574803149606293529 ) ) ;
#12667 = EDGE_CURVE ( 'NONE', #34486, #23961, #45020, .T. ) ;
#12668 = DIRECTION ( 'NONE',  ( 0.000000000000000000, -0.000000000000000000, 1.000000000000000000 ) ) ;
#12669 = AXIS2_PLACEMENT_3D ( 'NONE', #17777, #11299, #47125 ) ;
#12670 = ADVANCED_FACE ( 'NONE', ( #44951 ), #41107, .T. ) ;
#12671 = FACE_OUTER_BOUND ( 'NONE', #12028, .T. ) ;
#12672 = ADVANCED_FACE ( 'NONE', ( #9605 ), #25349, .F. ) ;
#12673 = AXIS2_PLACEMENT_3D ( 'NONE', #10995, #123, #15870 ) ;
#12674 = FACE_OUTER_BOUND ( 'NONE', #851, .T. ) ;
#12675 = VECTOR ( 'NONE', #13255, 39.37007874015748143 ) ;
#12676 = CARTESIAN_POINT ( 'NONE',  ( 1.015142113812069313, 0.000000000000000000, 0.4724409448818868706 ) ) ;
#12677 = ADVANCED_FACE ( 'NONE', ( #5978 ), #25598, .T. ) ;
#12678 = DIRECTION ( 'NONE',  ( 0.000000000000000000, 0.000000000000000000, 1.000000000000000000 ) ) ;
#12679 = DIRECTION ( 'NONE',  ( -0.000000000000000000, 1.000000000000000000, -0.000000000000000000 ) ) ;
#12680 = VECTOR ( 'NONE', #2593, 39.37007874015748143 ) ;
#12681 = VERTEX_POINT ( 'NONE', #48544 ) ;
#12682 = FACE_OUTER_BOUND ( 'NONE', #26018, .T. ) ;
#12683 = CARTESIAN_POINT ( 'NONE',  ( -1.004926760980926259, 2.755905511811024056, -0.6205843980233154422 ) ) ;
#12684 = ORIENTED_EDGE ( 'NONE', *, *, #24119, .F. ) ;
#12685 = ORIENTED_EDGE ( 'NONE', *, *, #28011, .F. ) ;
#12686 = DIRECTION ( 'NONE',  ( 0.8805955318567391110, 5.496845023002422681E-17, -0.4738686624729965269 ) ) ;
#12687 = DIRECTION ( 'NONE',  ( -3.469446951953613696E-16, 0.000000000000000000, -1.000000000000000000 ) ) ;
#12688 = EDGE_CURVE ( 'NONE', #13074, #18617, #32709, .T. ) ;
#12689 = CARTESIAN_POINT ( 'NONE',  ( 0.000000000000000000, 3.346456692913386100, 0.000000000000000000 ) ) ;
#12690 = EDGE_LOOP ( 'NONE', ( #44395, #35458, #39117, #308 ) ) ;
#12691 = B_SPLINE_CURVE_WITH_KNOTS ( 'NONE', 3,
 ( #24310, #36191, #36445, #39799 ),
 .UNSPECIFIED., .F., .F.,
 ( 4, 4 ),
 ( 0.1211873102087489551, 0.1625992483279400380 ),
 .UNSPECIFIED. ) ;
#12692 = EDGE_CURVE ( 'NONE', #19583, #47436, #19109, .T. ) ;
#12693 = ORIENTED_EDGE ( 'NONE', *, *, #32991, .T. ) ;
#12694 = LINE ( 'NONE', #12178, #50101 ) ;
#12695 = VERTEX_POINT ( 'NONE', #46456 ) ;
#12696 = DIRECTION ( 'NONE',  ( 1.734723475976806848E-16, -0.000000000000000000, 1.000000000000000000 ) ) ;
#12697 = VERTEX_POINT ( 'NONE', #29984 ) ;
#12698 = CARTESIAN_POINT ( 'NONE',  ( 0.8318848978143555950, 1.626432784511790963, 2.356606652973837424 ) ) ;
#12699 = DIRECTION ( 'NONE',  ( -1.000000000000000000, 0.000000000000000000, 1.734723475976806848E-16 ) ) ;
#12700 = DIRECTION ( 'NONE',  ( 1.734723475976806848E-16, -0.000000000000000000, 1.000000000000000000 ) ) ;
#12701 = ORIENTED_EDGE ( 'NONE', *, *, #14671, .T. ) ;
#12702 = CIRCLE ( 'NONE', #309, 2.106299212598425008 ) ;
#12703 = ORIENTED_EDGE ( 'NONE', *, *, #36607, .T. ) ;
#12704 = ORIENTED_EDGE ( 'NONE', *, *, #30531, .T. ) ;
#12705 = CARTESIAN_POINT ( 'NONE',  ( -2.047277537895663801, 1.675111054312220515, 0.7169459839182066307 ) ) ;
#12706 = AXIS2_PLACEMENT_3D ( 'NONE', #32820, #9820, #25559 ) ;
#12707 = ORIENTED_EDGE ( 'NONE', *, *, #2186, .F. ) ;
#12708 = ORIENTED_EDGE ( 'NONE', *, *, #21854, .F. ) ;
#12709 = AXIS2_PLACEMENT_3D ( 'NONE', #28727, #20991, #48571 ) ;
#12710 = CARTESIAN_POINT ( 'NONE',  ( -1.325491792074585451, 1.543512378121542961, -2.638988599164751925 ) ) ;
#12711 = CARTESIAN_POINT ( 'NONE',  ( -0.2727639067037607723, 3.346456692913386100, -0.1574803149606301411 ) ) ;
#12712 = CARTESIAN_POINT ( 'NONE',  ( 2.932638728931774352, 1.666481914436860334, 0.3475908556738225297 ) ) ;
#12713 = ADVANCED_FACE ( 'NONE', ( #22494 ), #38990, .F. ) ;
#12714 = VECTOR ( 'NONE', #48841, 39.37007874015748143 ) ;
#12715 = VECTOR ( 'NONE', #36180, 39.37007874015748854 ) ;
#12716 = VERTEX_POINT ( 'NONE', #19358 ) ;
#12717 = CARTESIAN_POINT ( 'NONE',  ( 0.7423782071083082634, 3.267716535433071279, -2.086614173228340086 ) ) ;
#12718 = DIRECTION ( 'NONE',  ( -0.000000000000000000, 1.000000000000000000, -0.000000000000000000 ) ) ;
#12719 = DIRECTION ( 'NONE',  ( -0.9998717552508122886, -0.01601477604151182316, 0.000000000000000000 ) ) ;
#12720 = ORIENTED_EDGE ( 'NONE', *, *, #16570, .F. ) ;
#12721 = CARTESIAN_POINT ( 'NONE',  ( -2.734482843737247038, 1.676638068352269029, -1.115254632218712016 ) ) ;
#12722 = FACE_OUTER_BOUND ( 'NONE', #48120, .T. ) ;
#12723 = AXIS2_PLACEMENT_3D ( 'NONE', #5387, #28359, #8747 ) ;
#12724 = ORIENTED_EDGE ( 'NONE', *, *, #48040, .F. ) ;
#12725 = CARTESIAN_POINT ( 'NONE',  ( -2.633954527054724437, 1.575688309503748830, -0.5507047405504611470 ) ) ;
#12726 = ORIENTED_EDGE ( 'NONE', *, *, #8777, .F. ) ;
#12727 = ORIENTED_EDGE ( 'NONE', *, *, #15052, .F. ) ;
#12728 = CARTESIAN_POINT ( 'NONE',  ( -2.339241080213612101, 1.584370211609867685, 1.802537235681884065 ) ) ;
#12729 = FACE_OUTER_BOUND ( 'NONE', #1447, .T. ) ;
#12730 = DIRECTION ( 'NONE',  ( -0.01601477604151182663, 0.9998717552508123996, -0.000000000000000000 ) ) ;
#12731 = LINE ( 'NONE', #16353, #17253 ) ;
#12732 = ORIENTED_EDGE ( 'NONE', *, *, #13146, .T. ) ;
#12733 = ORIENTED_EDGE ( 'NONE', *, *, #30115, .T. ) ;
#12734 = EDGE_CURVE ( 'NONE', #39780, #904, #46704, .T. ) ;
#12735 = CARTESIAN_POINT ( 'NONE',  ( 2.182111253630085290, 0.000000000000000000, -0.5118110236220471121 ) ) ;
#12736 = VERTEX_POINT ( 'NONE', #45701 ) ;
#12737 = PLANE ( 'NONE',  #13748 ) ;
#12738 = LINE ( 'NONE', #11971, #40796 ) ;
#12739 = EDGE_CURVE ( 'NONE', #26290, #22720, #26111, .T. ) ;
#12740 = B_SPLINE_CURVE_WITH_KNOTS ( 'NONE', 3,
 ( #2142, #32374, #22274, #42638 ),
 .UNSPECIFIED., .F., .F.,
 ( 4, 4 ),
 ( 6.194644966465025756E-07, 0.001846361613927027844 ),
 .UNSPECIFIED. ) ;
#12741 = EDGE_CURVE ( 'NONE', #5207, #5416, #35126, .T. ) ;
#12742 = ADVANCED_FACE ( 'NONE', ( #38250 ), #22244, .F. ) ;
#12743 = CARTESIAN_POINT ( 'NONE',  ( -1.794796351285542491, 3.346456692913386100, 1.102362204724404160 ) ) ;
#12744 = CIRCLE ( 'NONE', #42399, 2.244934639244525076 ) ;
#12745 = PLANE ( 'NONE',  #35961 ) ;
#12746 = CARTESIAN_POINT ( 'NONE',  ( 2.182111253630085290, 3.346456692913386100, -0.1968503937007886062 ) ) ;
#12747 = VERTEX_POINT ( 'NONE', #34119 ) ;
#12748 = VECTOR ( 'NONE', #20995, 39.37007874015748143 ) ;
#12749 = DIRECTION ( 'NONE',  ( -0.000000000000000000, 1.000000000000000000, -0.000000000000000000 ) ) ;
#12750 = VECTOR ( 'NONE', #7523, 39.37007874015748143 ) ;
#12751 = CARTESIAN_POINT ( 'NONE',  ( 1.015142113812069313, 3.267716535433071279, -0.9842519685039348154 ) ) ;
#12752 = AXIS2_PLACEMENT_3D ( 'NONE', #27030, #7675, #23672 ) ;
#12753 = AXIS2_PLACEMENT_3D ( 'NONE', #36120, #750, #16500 ) ;
#12754 = VERTEX_POINT ( 'NONE', #46208 ) ;
#12755 = DIRECTION ( 'NONE',  ( 0.000000000000000000, -1.000000000000000000, 0.000000000000000000 ) ) ;
#12756 = DIRECTION ( 'NONE',  ( 1.000000000000000000, 0.000000000000000000, 0.000000000000000000 ) ) ;
#12757 = EDGE_CURVE ( 'NONE', #29976, #8862, #14998, .T. ) ;
#12758 = LINE ( 'NONE', #13013, #18878 ) ;
#12759 = ORIENTED_EDGE ( 'NONE', *, *, #31958, .F. ) ;
#12760 = CARTESIAN_POINT ( 'NONE',  ( -0.07591351300297362326, 3.267716535433071279, -2.104930761696520491 ) ) ;
#12761 = CARTESIAN_POINT ( 'NONE',  ( -1.353122744573580727, 3.267716535433071279, -1.614173228346451605 ) ) ;
#12762 = CARTESIAN_POINT ( 'NONE',  ( -2.426831398316064980, 1.574814413673615521, -0.05972692158529400303 ) ) ;
#12763 = VECTOR ( 'NONE', #15516, 39.37007874015748143 ) ;
#12764 = ADVANCED_FACE ( 'NONE', ( #49808 ), #14493, .F. ) ;
#12765 = ORIENTED_EDGE ( 'NONE', *, *, #30133, .F. ) ;
#12766 = LINE ( 'NONE', #19975, #21380 ) ;
#12767 = CARTESIAN_POINT ( 'NONE',  ( 2.193564619503452828, 1.644610705845120258, 0.7644775380370429918 ) ) ;
#12768 = ORIENTED_EDGE ( 'NONE', *, *, #32795, .F. ) ;
#12769 = CARTESIAN_POINT ( 'NONE',  ( 0.07982360342473591996, 1.709180471932028711, 0.000000000000000000 ) ) ;
#12770 = CARTESIAN_POINT ( 'NONE',  ( -0.8942052331142552601, 3.346456692913386100, -0.6299212598425177889 ) ) ;
#12771 = PLANE ( 'NONE',  #42018 ) ;
#12772 = CARTESIAN_POINT ( 'NONE',  ( -1.985260859929297572, 3.346456692913386100, -0.3149606299212589500 ) ) ;
#12773 = EDGE_CURVE ( 'NONE', #36153, #18093, #36127, .T. ) ;
#12774 = VERTEX_POINT ( 'NONE', #30243 ) ;
#12775 = VERTEX_POINT ( 'NONE', #42105 ) ;
#12776 = DIRECTION ( 'NONE',  ( 0.000000000000000000, 0.000000000000000000, -1.000000000000000000 ) ) ;
#12777 = PLANE ( 'NONE',  #6518 ) ;
#12778 = VERTEX_POINT ( 'NONE', #34872 ) ;
#12779 = DIRECTION ( 'NONE',  ( -0.000000000000000000, 1.000000000000000000, -0.000000000000000000 ) ) ;
#12780 = FACE_OUTER_BOUND ( 'NONE', #16962, .T. ) ;
#12781 = CARTESIAN_POINT ( 'NONE',  ( 2.255357468390372322, 1.645600431408117847, -0.5652488166673508285 ) ) ;
#12782 = EDGE_CURVE ( 'NONE', #32538, #3117, #19392, .T. ) ;
#12783 = DIRECTION ( 'NONE',  ( -0.9998717552508122886, -0.01601477604151185785, 0.000000000000000000 ) ) ;
#12784 = ORIENTED_EDGE ( 'NONE', *, *, #46327, .F. ) ;
#12785 = EDGE_LOOP ( 'NONE', ( #1489, #35837, #10445, #4855, #35524, #5834, #33685, #13685, #43164, #7437, #1077 ) ) ;
#12786 = PLANE ( 'NONE',  #6487 ) ;
#12787 = DIRECTION ( 'NONE',  ( -0.000000000000000000, 1.000000000000000000, -0.000000000000000000 ) ) ;
#12788 = CARTESIAN_POINT ( 'NONE',  ( 2.088343298084792021, 6.692913385826772199, 0.6267986818430609786 ) ) ;
#12789 = B_SPLINE_CURVE_WITH_KNOTS ( 'NONE', 3,
 ( #32562, #4668, #16549, #28922 ),
 .UNSPECIFIED., .F., .F.,
 ( 4, 4 ),
 ( 0.0003468416213337044527, 0.002847000924371759830 ),
 .UNSPECIFIED. ) ;
#12790 = CARTESIAN_POINT ( 'NONE',  ( 1.386843392441768241, 1.730114785850798587, -1.825100698618727257 ) ) ;
#12791 = FACE_BOUND ( 'NONE', #43079, .T. ) ;
#12792 = VECTOR ( 'NONE', #16807, 39.37007874015748143 ) ;
#12793 = ORIENTED_EDGE ( 'NONE', *, *, #45834, .F. ) ;
#12794 = EDGE_CURVE ( 'NONE', #17583, #15817, #11125, .T. ) ;
#12795 = CARTESIAN_POINT ( 'NONE',  ( 0.1499993486716910962, 0.5230385143951955529, -2.215636156144062063 ) ) ;
#12796 = VECTOR ( 'NONE', #39474, 39.37007874015748143 ) ;
#12797 = ORIENTED_EDGE ( 'NONE', *, *, #42804, .T. ) ;
#12798 = ORIENTED_EDGE ( 'NONE', *, *, #22601, .F. ) ;
#12799 = DIRECTION ( 'NONE',  ( 0.9797780297642104674, 0.000000000000000000, 0.2000875118326023161 ) ) ;
#12800 = VECTOR ( 'NONE', #34989, 39.37007874015748143 ) ;
#12801 = ADVANCED_FACE ( 'NONE', ( #50304 ), #30745, .T. ) ;
#12802 = ORIENTED_EDGE ( 'NONE', *, *, #49462, .F. ) ;
#12803 = ORIENTED_EDGE ( 'NONE', *, *, #48328, .F. ) ;
#12804 = CARTESIAN_POINT ( 'NONE',  ( -0.7874015748031498729, 0.000000000000000000, -1.138269997360109921E-16 ) ) ;
#12805 = ORIENTED_EDGE ( 'NONE', *, *, #50588, .F. ) ;
#12806 = VECTOR ( 'NONE', #42967, 39.37007874015748143 ) ;
#12807 = CARTESIAN_POINT ( 'NONE',  ( -1.083598637574820334, 1.603934357758587614, 2.747180975113330259 ) ) ;
#12808 = CARTESIAN_POINT ( 'NONE',  ( 0.7381027496705270252, 1.632310643118564997, -2.859439394060913298 ) ) ;
#12809 = CARTESIAN_POINT ( 'NONE',  ( 1.560669927219590525, 0.000000000000000000, -0.9842519685039348154 ) ) ;
#12810 = EDGE_CURVE ( 'NONE', #39003, #16783, #50811, .T. ) ;
#12811 = CARTESIAN_POINT ( 'NONE',  ( 0.7423782071083087075, 0.000000000000000000, 0.9448818897637746295 ) ) ;
#12812 = EDGE_CURVE ( 'NONE', #24660, #48339, #11473, .T. ) ;
#12813 = DIRECTION ( 'NONE',  ( 0.000000000000000000, 0.000000000000000000, 1.000000000000000000 ) ) ;
#12814 = CARTESIAN_POINT ( 'NONE',  ( -0.8182917201112823724, 3.267716535433071279, 1.419509857074484278E-16 ) ) ;
#12815 = VERTEX_POINT ( 'NONE', #18875 ) ;
#12816 = FACE_OUTER_BOUND ( 'NONE', #25241, .T. ) ;
#12817 = DIRECTION ( 'NONE',  ( -2.200518442539857142E-16, 0.7071067811865483499, 0.7071067811865465735 ) ) ;
#12818 = LINE ( 'NONE', #680, #89 ) ;
#12819 = ORIENTED_EDGE ( 'NONE', *, *, #8818, .F. ) ;
#12820 = CARTESIAN_POINT ( 'NONE',  ( -0.1198125010151041281, 0.5249316497054294928, -1.880232808544963108 ) ) ;
#12821 = DIRECTION ( 'NONE',  ( 9.964307797194671432E-17, -1.000000000000000000, -5.953396763000495864E-17 ) ) ;
#12822 = VERTEX_POINT ( 'NONE', #28382 ) ;
#12823 = CARTESIAN_POINT ( 'NONE',  ( -0.6214413264104939882, 0.000000000000000000, 1.535433070866133898 ) ) ;
#12824 = FACE_OUTER_BOUND ( 'NONE', #16501, .T. ) ;
#12825 = CARTESIAN_POINT ( 'NONE',  ( 2.308557526972506047, 0.000000000000000000, 1.841013194464792724 ) ) ;
#12826 = VECTOR ( 'NONE', #19330, 39.37007874015748143 ) ;
#12827 = VECTOR ( 'NONE', #22996, 39.37007874015748143 ) ;
#12828 = ORIENTED_EDGE ( 'NONE', *, *, #39829, .T. ) ;
#12829 = LINE ( 'NONE', #40458, #10908 ) ;
#12830 = VERTEX_POINT ( 'NONE', #19860 ) ;
#12831 = FACE_BOUND ( 'NONE', #9078, .T. ) ;
#12832 = VECTOR ( 'NONE', #26411, 39.37007874015748143 ) ;
#12833 = CARTESIAN_POINT ( 'NONE',  ( 3.927031490892378253E-16, 0.000000000000000000, 1.692913385826762873 ) ) ;
#12834 = CARTESIAN_POINT ( 'NONE',  ( -1.536664496436148184E-16, 3.346456692913386100, -1.456692913385822630 ) ) ;
#12835 = CARTESIAN_POINT ( 'NONE',  ( 1.091055626815042645, 3.346456692913386100, -0.5118110236220471121 ) ) ;
#12836 = AXIS2_PLACEMENT_3D ( 'NONE', #2944, #34196, #18700 ) ;
#12837 = ADVANCED_FACE ( 'NONE', ( #23491 ), #35631, .F. ) ;
#12838 = VECTOR ( 'NONE', #19799, 39.37007874015748143 ) ;
#12839 = ORIENTED_EDGE ( 'NONE', *, *, #1032, .T. ) ;
#12840 = ORIENTED_EDGE ( 'NONE', *, *, #32092, .F. ) ;
#12841 = DIRECTION ( 'NONE',  ( 1.734723475976806848E-16, -0.000000000000000000, 1.000000000000000000 ) ) ;
#12842 = ORIENTED_EDGE ( 'NONE', *, *, #36577, .F. ) ;
#12843 = DIRECTION ( 'NONE',  ( 1.000000000000000000, -0.000000000000000000, 0.000000000000000000 ) ) ;
#12844 = ORIENTED_EDGE ( 'NONE', *, *, #18615, .F. ) ;
#12845 = EDGE_CURVE ( 'NONE', #42204, #7511, #15501, .T. ) ;
#12846 = CARTESIAN_POINT ( 'NONE',  ( 0.9297740550868999199, 0.5225294794730628301, -2.044119187424908279 ) ) ;
#12847 = EDGE_CURVE ( 'NONE', #31828, #48695, #28123, .T. ) ;
#12848 = VERTEX_POINT ( 'NONE', #27360 ) ;
#12849 = DIRECTION ( 'NONE',  ( 1.000000000000000000, 0.000000000000000000, 0.000000000000000000 ) ) ;
#12850 = EDGE_CURVE ( 'NONE', #30403, #3143, #10883, .T. ) ;
#12851 = DIRECTION ( 'NONE',  ( 0.08963930890342654279, 0.000000000000000000, 0.9959742939952397345 ) ) ;
#12852 = ORIENTED_EDGE ( 'NONE', *, *, #27819, .F. ) ;
#12853 = CARTESIAN_POINT ( 'NONE',  ( 0.000000000000000000, 3.346456692913386100, 0.000000000000000000 ) ) ;
#12854 = ORIENTED_EDGE ( 'NONE', *, *, #49452, .F. ) ;
#12855 = CARTESIAN_POINT ( 'NONE',  ( -0.2727639067037608278, 3.267716535433071279, -0.3543307086614175816 ) ) ;
#12856 = ORIENTED_EDGE ( 'NONE', *, *, #29863, .F. ) ;
#12857 = VERTEX_POINT ( 'NONE', #8518 ) ;
#12858 = EDGE_CURVE ( 'NONE', #10544, #14916, #24269, .T. ) ;
#12859 = CARTESIAN_POINT ( 'NONE',  ( 2.793030215715258446, 1.451280567205322836, 0.9592557174602683867 ) ) ;
#12860 = VECTOR ( 'NONE', #13712, 39.37007874015748143 ) ;
#12861 = CONICAL_SURFACE ( 'NONE', #15324, 2.246510896728926010, 0.01601546068027819014 ) ;
#12862 = ORIENTED_EDGE ( 'NONE', *, *, #7469, .T. ) ;
#12863 = DIRECTION ( 'NONE',  ( -1.156061316345072978E-16, -1.000000000000000000, -1.040474016969658122E-17 ) ) ;
#12864 = VECTOR ( 'NONE', #27860, 39.37007874015748143 ) ;
#12865 = EDGE_LOOP ( 'NONE', ( #15645, #23375, #8493, #50063 ) ) ;
#12866 = DIRECTION ( 'NONE',  ( -3.469446951953613696E-16, 0.000000000000000000, -1.000000000000000000 ) ) ;
#12867 = EDGE_CURVE ( 'NONE', #9567, #32706, #44104, .T. ) ;
#12868 = CARTESIAN_POINT ( 'NONE',  ( 2.164658444855302122, 5.905511811023623991, -0.04795272066889885720 ) ) ;
#12869 = VECTOR ( 'NONE', #13489, 39.37007874015748143 ) ;
#12870 = DIRECTION ( 'NONE',  ( -3.986037398843765983E-20, -1.000000000000000000, -1.160734090543304660E-16 ) ) ;
#12871 = EDGE_CURVE ( 'NONE', #16212, #39823, #431, .T. ) ;
#12872 = ORIENTED_EDGE ( 'NONE', *, *, #18724, .F. ) ;
#12873 = VECTOR ( 'NONE', #30170, 39.37007874015748143 ) ;
#12874 = CARTESIAN_POINT ( 'NONE',  ( 1.395323331571632020, 0.5249316497054298258, -1.265979166534827449 ) ) ;
#12875 = CARTESIAN_POINT ( 'NONE',  ( -1.091055626815042201, 3.346456692913386100, 0.9448818897637749625 ) ) ;
#12876 = CARTESIAN_POINT ( 'NONE',  ( 2.685792526206067343, 1.659196497464942022, -0.5625364255821559967 ) ) ;
#12877 = DIRECTION ( 'NONE',  ( -1.000000000000000000, -0.000000000000000000, -0.000000000000000000 ) ) ;
#12878 = DIRECTION ( 'NONE',  ( 1.000000000000000000, 0.000000000000000000, 0.000000000000000000 ) ) ;
#12879 = CARTESIAN_POINT ( 'NONE',  ( -1.834323595590334977, 1.205361022782829114E-17, 1.151859023884900690 ) ) ;
#12880 = DIRECTION ( 'NONE',  ( 7.237058681235334921E-17, -1.000000000000000000, -9.074984547606431700E-17 ) ) ;
#12881 = ORIENTED_EDGE ( 'NONE', *, *, #27184, .T. ) ;
#12882 = LINE ( 'NONE', #30, #2336 ) ;
#12883 = CARTESIAN_POINT ( 'NONE',  ( 0.000000000000000000, 0.000000000000000000, 0.000000000000000000 ) ) ;
#12884 = ORIENTED_EDGE ( 'NONE', *, *, #42863, .F. ) ;
#12885 = CARTESIAN_POINT ( 'NONE',  ( 1.325491792074624087, 1.641458297549746037, -2.638988599164732385 ) ) ;
#12886 = ORIENTED_EDGE ( 'NONE', *, *, #22380, .T. ) ;
#12887 = PLANE ( 'NONE',  #48670 ) ;
#12888 = CARTESIAN_POINT ( 'NONE',  ( 1.997134316236881091, 3.346456692913386100, -0.6692913385826764205 ) ) ;
#12889 = LINE ( 'NONE', #9014, #3966 ) ;
#12890 = DIRECTION ( 'NONE',  ( -0.000000000000000000, 0.000000000000000000, 1.000000000000000000 ) ) ;
#12891 = CARTESIAN_POINT ( 'NONE',  ( 0.000000000000000000, 3.267716535433071279, 0.000000000000000000 ) ) ;
#12892 = VERTEX_POINT ( 'NONE', #40014 ) ;
#12893 = AXIS2_PLACEMENT_3D ( 'NONE', #24105, #39851, #4484 ) ;
#12894 = DIRECTION ( 'NONE',  ( -1.000000000000000000, 0.000000000000000000, 0.000000000000000000 ) ) ;
#12895 = VECTOR ( 'NONE', #50286, 39.37007874015748143 ) ;
#12896 = FACE_BOUND ( 'NONE', #45610, .T. ) ;
#12897 = VECTOR ( 'NONE', #39973, 39.37007874015748143 ) ;
#12898 = ORIENTED_EDGE ( 'NONE', *, *, #22316, .F. ) ;
#12899 = CARTESIAN_POINT ( 'NONE',  ( 0.8182917201112819283, 0.000000000000000000, -1.102362204724405714 ) ) ;
#12900 = AXIS2_PLACEMENT_3D ( 'NONE', #11943, #13988, #33874 ) ;
#12901 = ORIENTED_EDGE ( 'NONE', *, *, #4250, .F. ) ;
#12902 = CARTESIAN_POINT ( 'NONE',  ( 1.355960331127249452, 0.04963785175798203497, -1.364517356352728861 ) ) ;
#12903 = LINE ( 'NONE', #32272, #36312 ) ;
#12904 = EDGE_CURVE ( 'NONE', #33946, #1872, #8262, .T. ) ;
#12905 = AXIS2_PLACEMENT_3D ( 'NONE', #25944, #25686, #25183 ) ;
#12906 = EDGE_CURVE ( 'NONE', #36716, #45331, #39242, .T. ) ;
#12907 = EDGE_CURVE ( 'NONE', #23085, #3720, #2907, .T. ) ;
#12908 = VECTOR ( 'NONE', #13101, 39.37007874015748143 ) ;
#12909 = CARTESIAN_POINT ( 'NONE',  ( -0.8067290215918269114, 6.692913385826772199, 2.009464521518169899 ) ) ;
#12910 = ORIENTED_EDGE ( 'NONE', *, *, #10007, .T. ) ;
#12911 = EDGE_LOOP ( 'NONE', ( #16536, #13348, #202, #22857 ) ) ;
#12912 = PRODUCT_DEFINITION_SHAPE ( 'NONE', 'NONE',  #24694 ) ;
#12913 = CARTESIAN_POINT ( 'NONE',  ( 0.2727639067037604392, 3.346456692913386100, -1.614173228346451605 ) ) ;
#12914 = LINE ( 'NONE', #17544, #50354 ) ;
#12915 = FACE_BOUND ( 'NONE', #15098, .T. ) ;
#12916 = EDGE_CURVE ( 'NONE', #35907, #9339, #39755, .T. ) ;
#12917 = CARTESIAN_POINT ( 'NONE',  ( 0.1155636338427008941, -0.5222242541845523167, 0.000000000000000000 ) ) ;
#12918 = PLANE ( 'NONE',  #48083 ) ;
#12919 = VERTEX_POINT ( 'NONE', #47202 ) ;
#12920 = LINE ( 'NONE', #28132, #43896 ) ;
#12921 = ORIENTED_EDGE ( 'NONE', *, *, #47694, .T. ) ;
#12922 = ORIENTED_EDGE ( 'NONE', *, *, #30719, .T. ) ;
#12923 = ADVANCED_FACE ( 'NONE', ( #3882 ), #44130, .F. ) ;
#12924 = VERTEX_POINT ( 'NONE', #8774 ) ;
#12925 = CARTESIAN_POINT ( 'NONE',  ( -0.03497847339001228933, 2.755905511811024056, 1.180584302963952448 ) ) ;
#12926 = CARTESIAN_POINT ( 'NONE',  ( 0.4696143004045476577, 3.346456692913386100, -2.047244094488182231 ) ) ;
#12927 = EDGE_CURVE ( 'NONE', #25574, #17583, #4565, .T. ) ;
#12929 = CARTESIAN_POINT ( 'NONE',  ( 2.932638728931774352, 1.666481914436860334, 0.3475908556738225297 ) ) ;
#12928 = VECTOR ( 'NONE', #43647, 39.37007874015748143 ) ;
#12930 = CARTESIAN_POINT ( 'NONE',  ( -1.775400203342670569, 1.205361022782829114E-17, -2.359903268218729089 ) ) ;
#12931 = EDGE_CURVE ( 'NONE', #40451, #11955, #36144, .T. ) ;
#12932 = ORIENTED_EDGE ( 'NONE', *, *, #3869, .F. ) ;
#12933 = VERTEX_POINT ( 'NONE', #32277 ) ;
#12935 = VECTOR ( 'NONE', #46110, 39.37007874015748143 ) ;
#12934 = DIRECTION ( 'NONE',  ( -1.000000000000000000, 0.000000000000000000, 1.734723475976806848E-16 ) ) ;
#12936 = LINE ( 'NONE', #13192, #27917 ) ;
#12937 = EDGE_CURVE ( 'NONE', #18734, #11675, #45972, .T. ) ;
#12938 = LINE ( 'NONE', #5178, #1880 ) ;
#12939 = B_SPLINE_CURVE_WITH_KNOTS ( 'NONE', 3,
 ( #14647, #37901, #10768, #45352 ),
 .UNSPECIFIED., .F., .F.,
 ( 4, 4 ),
 ( 0.1211775127643062444, 0.1625894504277921315 ),
 .UNSPECIFIED. ) ;
#12940 = ADVANCED_FACE ( 'NONE', ( #47972 ), #35381, .F. ) ;
#12941 = PLANE ( 'NONE',  #17727 ) ;
#12942 = LINE ( 'NONE', #24035, #41277 ) ;
#12943 = CARTESIAN_POINT ( 'NONE',  ( 0.1968503937007872462, 0.000000000000000000, -1.141732283464564013 ) ) ;
#12944 = AXIS2_PLACEMENT_3D ( 'NONE', #39331, #12730, #16351 ) ;
#12945 = CARTESIAN_POINT ( 'NONE',  ( 1.909347346926324462, 3.346456692913386100, -1.102362204724406602 ) ) ;
#12946 = AXIS2_PLACEMENT_3D ( 'NONE', #3694, #11688, #27679 ) ;
#12947 = ORIENTED_EDGE ( 'NONE', *, *, #19103, .F. ) ;
#12948 = DIRECTION ( 'NONE',  ( -0.01601477604151182663, 0.9998717552508123996, -0.000000000000000000 ) ) ;
#12949 = DIRECTION ( 'NONE',  ( -1.000000000000000000, 0.000000000000000000, 0.000000000000000000 ) ) ;
#12950 = ORIENTED_EDGE ( 'NONE', *, *, #6255, .F. ) ;
#12951 = ORIENTED_EDGE ( 'NONE', *, *, #48141, .T. ) ;
#12952 = DIRECTION ( 'NONE',  ( -0.000000000000000000, 1.000000000000000000, -0.000000000000000000 ) ) ;
#12953 = CARTESIAN_POINT ( 'NONE',  ( -1.363819533518803473, 3.244427737985139171, 2.040716226787704368 ) ) ;
#12954 = ORIENTED_EDGE ( 'NONE', *, *, #1995, .T. ) ;
#12955 = ORIENTED_EDGE ( 'NONE', *, *, #43513, .F. ) ;
#12956 = PLANE ( 'NONE',  #16361 ) ;
#12957 = ORIENTED_EDGE ( 'NONE', *, *, #16310, .T. ) ;
#12958 = VERTEX_POINT ( 'NONE', #48992 ) ;
#12959 = CARTESIAN_POINT ( 'NONE',  ( 0.3820226255272446414, 0.03403845698394380309, 1.829505193364920679 ) ) ;
#12960 = PLANE ( 'NONE',  #9883 ) ;
#12961 = AXIS2_PLACEMENT_3D ( 'NONE', #40084, #23561, #47019 ) ;
#12962 = AXIS2_PLACEMENT_3D ( 'NONE', #14536, #18665, #26400 ) ;
#12963 = ORIENTED_EDGE ( 'NONE', *, *, #20191, .F. ) ;
#12964 = EDGE_CURVE ( 'NONE', #18779, #45470, #32800, .T. ) ;
#12965 = ORIENTED_EDGE ( 'NONE', *, *, #9861, .T. ) ;
#12966 = VERTEX_POINT ( 'NONE', #48733 ) ;
#12967 = CONICAL_SURFACE ( 'NONE', #33589, 3.033577403570480779, 1.554780866114618743 ) ;
#12968 = LINE ( 'NONE', #43928, #2427 ) ;
#12969 = ADVANCED_FACE ( 'NONE', ( #33055 ), #40787, .T. ) ;
#12970 = ORIENTED_EDGE ( 'NONE', *, *, #19003, .F. ) ;
#12971 = ORIENTED_EDGE ( 'NONE', *, *, #47119, .F. ) ;
#12972 = CARTESIAN_POINT ( 'NONE',  ( 1.833433833923351353, 3.346456692913386100, 0.6299212598425164567 ) ) ;
#12973 = DIRECTION ( 'NONE',  ( -0.000000000000000000, 0.000000000000000000, 1.000000000000000000 ) ) ;
#12974 = DIRECTION ( 'NONE',  ( 0.9998717552508121775, 0.01601477604151182663, 0.000000000000000000 ) ) ;
#12975 = EDGE_CURVE ( 'NONE', #10793, #40287, #44632, .T. ) ;
#12976 = ORIENTED_EDGE ( 'NONE', *, *, #4225, .F. ) ;
#12977 = LINE ( 'NONE', #48038, #13935 ) ;
#12978 = DIRECTION ( 'NONE',  ( -0.01601477604151182663, 0.9998717552508123996, -0.000000000000000000 ) ) ;
#12979 = LINE ( 'NONE', #21232, #24530 ) ;
#12980 = ORIENTED_EDGE ( 'NONE', *, *, #21146, .T. ) ;
#12981 = DIRECTION ( 'NONE',  ( -0.000000000000000000, 0.000000000000000000, 1.000000000000000000 ) ) ;
#12982 = FACE_OUTER_BOUND ( 'NONE', #12509, .T. ) ;
#12983 = LINE ( 'NONE', #16603, #34025 ) ;
#12984 = ORIENTED_EDGE ( 'NONE', *, *, #3811, .F. ) ;
#12985 = ORIENTED_EDGE ( 'NONE', *, *, #41961, .F. ) ;
#12986 = DIRECTION ( 'NONE',  ( 0.000000000000000000, 1.000000000000000000, 0.000000000000000000 ) ) ;
#12987 = LINE ( 'NONE', #8087, #35006 ) ;
#12988 = VECTOR ( 'NONE', #19325, 39.37007874015748143 ) ;
#12989 = DIRECTION ( 'NONE',  ( -3.986037398843765983E-20, -1.000000000000000000, -1.160734090543304660E-16 ) ) ;
#12990 = EDGE_CURVE ( 'NONE', #44874, #17837, #13674, .T. ) ;
#12991 = CARTESIAN_POINT ( 'NONE',  ( 0.000000000000000000, 3.267716535433071279, -1.102362204724406602 ) ) ;
#12992 = CARTESIAN_POINT ( 'NONE',  ( -1.439733046521776361, 3.346456692913386100, 1.062992125984246083 ) ) ;
#12993 = ORIENTED_EDGE ( 'NONE', *, *, #35879, .F. ) ;
#12994 = ORIENTED_EDGE ( 'NONE', *, *, #43663, .T. ) ;
#12995 = ADVANCED_FACE ( 'NONE', ( #36400 ), #35079, .T. ) ;
#12996 = ADVANCED_FACE ( 'NONE', ( #21169 ), #16786, .T. ) ;
#12997 = CARTESIAN_POINT ( 'NONE',  ( 0.3530705266098149719, 0.000000000000000000, -0.1234057657284600290 ) ) ;
#12998 = ORIENTED_EDGE ( 'NONE', *, *, #48589, .F. ) ;
#12999 = CARTESIAN_POINT ( 'NONE',  ( 0.000000000000000000, 0.000000000000000000, 0.000000000000000000 ) ) ;
#13000 = CARTESIAN_POINT ( 'NONE',  ( 2.010517631316622644, 0.000000000000000000, 0.8058170502102376398 ) ) ;
#13001 = VECTOR ( 'NONE', #46753, 39.37007874015748143 ) ;
#13002 = AXIS2_PLACEMENT_3D ( 'NONE', #28680, #41087, #25077 ) ;
#13003 = CARTESIAN_POINT ( 'NONE',  ( 2.928234753086316644, 1.666404349079314562, 0.3801023109252803511 ) ) ;
#13004 = LINE ( 'NONE', #5245, #33509 ) ;
#13005 = CARTESIAN_POINT ( 'NONE',  ( 1.560669927219590303, 3.267716535433071279, -1.880327210325009046 ) ) ;
#13006 = ORIENTED_EDGE ( 'NONE', *, *, #46550, .F. ) ;
#13007 = LINE ( 'NONE', #28739, #36579 ) ;
#13008 = CONICAL_SURFACE ( 'NONE', #41861, 3.483074324928249421, 1.244861948955335196 ) ;
#13009 = LINE ( 'NONE', #6016, #6735 ) ;
#13010 = EDGE_LOOP ( 'NONE', ( #14428, #574, #35620, #27438 ) ) ;
#13011 = CARTESIAN_POINT ( 'NONE',  ( 0.000000000000000000, 3.267716535433071279, -0.6299212598425177889 ) ) ;
#13012 = CARTESIAN_POINT ( 'NONE',  ( 1.628466770324754176, 1.733984826446373750, -1.625060189682509870 ) ) ;
#13013 = CARTESIAN_POINT ( 'NONE',  ( 0.000000000000000000, 3.267716535433071279, 1.889763779527550369 ) ) ;
#13014 = ORIENTED_EDGE ( 'NONE', *, *, #2980, .F. ) ;
#13015 = DIRECTION ( 'NONE',  ( -0.000000000000000000, -1.000000000000000000, -0.000000000000000000 ) ) ;
#13016 = CIRCLE ( 'NONE', #33666, 1.850107469027523432 ) ;
#13017 = CARTESIAN_POINT ( 'NONE',  ( 2.437180031585944207, 1.459818316683583639, -1.667735833703099191 ) ) ;
#13018 = VERTEX_POINT ( 'NONE', #29155 ) ;
#13019 = FACE_OUTER_BOUND ( 'NONE', #27370, .T. ) ;
#13020 = CARTESIAN_POINT ( 'NONE',  ( 0.000000000000000000, 2.755905511811027164, 0.000000000000000000 ) ) ;
#13021 = ORIENTED_EDGE ( 'NONE', *, *, #39704, .F. ) ;
#13022 = VECTOR ( 'NONE', #27207, 39.37007874015748143 ) ;
#13023 = CARTESIAN_POINT ( 'NONE',  ( -0.2727639067037607723, 0.000000000000000000, -1.417322834645664331 ) ) ;
#13024 = DIRECTION ( 'NONE',  ( -0.000000000000000000, 1.000000000000000000, -0.000000000000000000 ) ) ;
#13025 = B_SPLINE_CURVE_WITH_KNOTS ( 'NONE', 3,
 ( #13660, #32786, #17529, #8760 ),
 .UNSPECIFIED., .F., .F.,
 ( 4, 4 ),
 ( 2.075195358405174660E-07, 0.01744788363431542047 ),
 .UNSPECIFIED. ) ;
#13026 = DIRECTION ( 'NONE',  ( 0.000000000000000000, 1.000000000000000000, 0.000000000000000000 ) ) ;
#13027 = DIRECTION ( 'NONE',  ( -3.469446951953613696E-16, 0.000000000000000000, -1.000000000000000000 ) ) ;
#13028 = DIRECTION ( 'NONE',  ( -1.000000000000000000, -0.000000000000000000, -0.000000000000000000 ) ) ;
#13029 = EDGE_CURVE ( 'NONE', #48909, #34275, #44888, .T. ) ;
#13030 = VERTEX_POINT ( 'NONE', #44388 ) ;
#13031 = VERTEX_POINT ( 'NONE', #24781 ) ;
#13032 = CARTESIAN_POINT ( 'NONE',  ( 0.000000000000000000, 3.267716535433071279, 0.1181102362204704270 ) ) ;
#13033 = CARTESIAN_POINT ( 'NONE',  ( -0.8182917201112819283, 0.000000000000000000, -1.102362204724405492 ) ) ;
#13034 = EDGE_CURVE ( 'NONE', #39521, #30165, #36918, .T. ) ;
#13035 = VERTEX_POINT ( 'NONE', #1792 ) ;
#13036 = CARTESIAN_POINT ( 'NONE',  ( -0.5455278134075216556, 0.000000000000000000, -2.401574803149598036 ) ) ;
#13037 = CARTESIAN_POINT ( 'NONE',  ( -2.491402175429631605, 1.581999109372839385, -1.585592796919542025 ) ) ;
#13038 = LINE ( 'NONE', #40413, #7157 ) ;
#13039 = EDGE_CURVE ( 'NONE', #4194, #3720, #10828, .T. ) ;
#13040 = FACE_OUTER_BOUND ( 'NONE', #35022, .T. ) ;
#13041 = ORIENTED_EDGE ( 'NONE', *, *, #27524, .T. ) ;
#13042 = EDGE_LOOP ( 'NONE', ( #46697, #42785, #14551, #20817, #23522 ) ) ;
#13043 = EDGE_CURVE ( 'NONE', #24046, #43573, #28897, .T. ) ;
#13044 = CARTESIAN_POINT ( 'NONE',  ( 0.000000000000000000, 3.267716535433071279, -0.6692913385826764205 ) ) ;
#13045 = DIRECTION ( 'NONE',  ( -0.000000000000000000, 1.000000000000000000, -0.000000000000000000 ) ) ;
#13046 = VECTOR ( 'NONE', #29532, 39.37007874015748143 ) ;
#13047 = AXIS2_PLACEMENT_3D ( 'NONE', #19976, #40134, #28496 ) ;
#13048 = CARTESIAN_POINT ( 'NONE',  ( 0.01640433696702632560, 1.621061233670012758, 2.952755905511811108 ) ) ;
#13049 = EDGE_CURVE ( 'NONE', #8816, #47610, #9032, .T. ) ;
#13050 = ORIENTED_EDGE ( 'NONE', *, *, #34206, .T. ) ;
#13051 = DIRECTION ( 'NONE',  ( 0.9998717552508121775, 0.01601477604151182663, 0.000000000000000000 ) ) ;
#13052 = FACE_BOUND ( 'NONE', #41047, .T. ) ;
#13053 = ORIENTED_EDGE ( 'NONE', *, *, #13034, .F. ) ;
#13054 = CARTESIAN_POINT ( 'NONE',  ( 1.091055626815042645, 3.267716535433071279, -0.5118110236220471121 ) ) ;
#13055 = EDGE_LOOP ( 'NONE', ( #32488, #21428, #50151, #36205 ) ) ;
#13057 = VERTEX_POINT ( 'NONE', #28559 ) ;
#13056 = AXIS2_PLACEMENT_3D ( 'NONE', #39703, #44333, #51005 ) ;
#13058 = CARTESIAN_POINT ( 'NONE',  ( 0.002207914879453961535, -5.712274067634378313E-18, 0.04916304461325374242 ) ) ;
#13059 = VECTOR ( 'NONE', #4693, 39.37007874015748143 ) ;
#13060 = EDGE_CURVE ( 'NONE', #28852, #16144, #30952, .T. ) ;
#13061 = ORIENTED_EDGE ( 'NONE', *, *, #9758, .T. ) ;
#13062 = DIRECTION ( 'NONE',  ( 1.000000000000000000, 0.000000000000000000, 0.000000000000000000 ) ) ;
#13063 = AXIS2_PLACEMENT_3D ( 'NONE', #28027, #20015, #43763 ) ;
#13064 = ORIENTED_EDGE ( 'NONE', *, *, #47248, .F. ) ;
#13065 = ADVANCED_FACE ( 'NONE', ( #12053 ), #26014, .T. ) ;
#13067 = LINE ( 'NONE', #12031, #26243 ) ;
#13066 = CIRCLE ( 'NONE', #3985, 2.165354330708661568 ) ;
#13068 = DIRECTION ( 'NONE',  ( 3.986037398843765983E-20, 1.000000000000000000, 1.160734090543304660E-16 ) ) ;
#13069 = DIRECTION ( 'NONE',  ( 9.964307797194671432E-17, -1.000000000000000000, -5.953396763000495864E-17 ) ) ;
#13070 = EDGE_CURVE ( 'NONE', #17742, #782, #33448, .T. ) ;
#13071 = FACE_OUTER_BOUND ( 'NONE', #45244, .T. ) ;
#13072 = LINE ( 'NONE', #31929, #27799 ) ;
#13073 = CARTESIAN_POINT ( 'NONE',  ( -0.8182917201112819283, 0.000000000000000000, -0.3543307086614175816 ) ) ;
#13074 = VERTEX_POINT ( 'NONE', #4563 ) ;
#13075 = DIRECTION ( 'NONE',  ( -0.01601477604151182663, 0.9998717552508123996, -0.000000000000000000 ) ) ;
#13076 = EDGE_CURVE ( 'NONE', #30686, #25226, #5073, .T. ) ;
#13077 = CARTESIAN_POINT ( 'NONE',  ( 0.1155636338427008941, -0.5222242541845523167, 0.000000000000000000 ) ) ;
#13078 = EDGE_LOOP ( 'NONE', ( #34185, #10480, #45079, #17835 ) ) ;
#13079 = LINE ( 'NONE', #29837, #14970 ) ;
#13080 = LINE ( 'NONE', #8433, #39300 ) ;
#13081 = ORIENTED_EDGE ( 'NONE', *, *, #15344, .T. ) ;
#13082 = DIRECTION ( 'NONE',  ( -1.000000000000000000, 0.000000000000000000, 0.000000000000000000 ) ) ;
#13083 = VECTOR ( 'NONE', #15178, 39.37007874015748143 ) ;
#13084 = DIRECTION ( 'NONE',  ( -1.000000000000000000, 0.000000000000000000, -0.000000000000000000 ) ) ;
#13085 = CARTESIAN_POINT ( 'NONE',  ( 2.138597145901430352, 6.692913385826772199, 0.3393547186367261159 ) ) ;
#13086 = ORIENTED_EDGE ( 'NONE', *, *, #17981, .F. ) ;
#13087 = VECTOR ( 'NONE', #3614, 39.37007874015748143 ) ;
#13088 = LINE ( 'NONE', #8186, #14193 ) ;
#13089 = ORIENTED_EDGE ( 'NONE', *, *, #19206, .F. ) ;
#13090 = FACE_BOUND ( 'NONE', #6563, .T. ) ;
#13091 = DIRECTION ( 'NONE',  ( 1.734723475976806848E-16, 0.000000000000000000, 1.000000000000000000 ) ) ;
#13092 = VECTOR ( 'NONE', #1145, 39.37007874015748143 ) ;
#13093 = CARTESIAN_POINT ( 'NONE',  ( -1.741553095960963734E-16, 3.267716535433071279, 3.021113040223572790E-32 ) ) ;
#13094 = DIRECTION ( 'NONE',  ( 0.000000000000000000, -1.000000000000000000, 0.000000000000000000 ) ) ;
#13095 = AXIS2_PLACEMENT_3D ( 'NONE', #40434, #31923, #28797 ) ;
#13096 = EDGE_LOOP ( 'NONE', ( #5186, #30353, #11522, #7124 ) ) ;
#13097 = ORIENTED_EDGE ( 'NONE', *, *, #4067, .F. ) ;
#13098 = CARTESIAN_POINT ( 'NONE',  ( -0.5455278134075214336, 0.000000000000000000, 2.204724409448808764 ) ) ;
#13099 = ORIENTED_EDGE ( 'NONE', *, *, #15765, .F. ) ;
#13100 = VECTOR ( 'NONE', #15916, 39.37007874015748143 ) ;
#13101 = DIRECTION ( 'NONE',  ( 1.000000000000000000, -0.000000000000000000, 0.000000000000000000 ) ) ;
#13102 = VERTEX_POINT ( 'NONE', #44306 ) ;
#13103 = EDGE_CURVE ( 'NONE', #25678, #32755, #39674, .T. ) ;
#13104 = LINE ( 'NONE', #44324, #33888 ) ;
#13105 = ORIENTED_EDGE ( 'NONE', *, *, #17426, .T. ) ;
#13106 = FACE_OUTER_BOUND ( 'NONE', #35498, .T. ) ;
#13107 = ADVANCED_FACE ( 'NONE', ( #31418 ), #47376, .T. ) ;
#13108 = DIRECTION ( 'NONE',  ( 1.734723475976806848E-16, -0.000000000000000000, 1.000000000000000000 ) ) ;
#13109 = ORIENTED_EDGE ( 'NONE', *, *, #21026, .T. ) ;
#13110 = CARTESIAN_POINT ( 'NONE',  ( 2.695799277629594037, 1.662794757381320654, -1.205759334241453651 ) ) ;
#13111 = VERTEX_POINT ( 'NONE', #20820 ) ;
#13112 = VERTEX_POINT ( 'NONE', #8185 ) ;
#13113 = B_SPLINE_CURVE_WITH_KNOTS ( 'NONE', 3,
 ( #42464, #6152, #46812, #15609 ),
 .UNSPECIFIED., .F., .F.,
 ( 4, 4 ),
 ( 0.01129884938030837997, 0.03073620617781123304 ),
 .UNSPECIFIED. ) ;
#13114 = AXIS2_PLACEMENT_3D ( 'NONE', #16974, #32731, #48409 ) ;
#13115 = ORIENTED_EDGE ( 'NONE', *, *, #5710, .F. ) ;
#13116 = ORIENTED_EDGE ( 'NONE', *, *, #47431, .F. ) ;
#13117 = CARTESIAN_POINT ( 'NONE',  ( -1.748867201173968100, 1.551518886663849628, -2.379180622689949676 ) ) ;
#13118 = ORIENTED_EDGE ( 'NONE', *, *, #43000, .F. ) ;
#13119 = DIRECTION ( 'NONE',  ( -1.000000000000000000, -0.000000000000000000, -0.000000000000000000 ) ) ;
#13120 = ORIENTED_EDGE ( 'NONE', *, *, #46694, .T. ) ;
#13121 = CARTESIAN_POINT ( 'NONE',  ( 0.1067246931122726866, 0.02962905676920215767, 0.000000000000000000 ) ) ;
#13122 = VECTOR ( 'NONE', #18370, 39.37007874015748143 ) ;
#13123 = VECTOR ( 'NONE', #6591, 39.37007874015748143 ) ;
#13124 = EDGE_CURVE ( 'NONE', #37873, #24076, #47118, .T. ) ;
#13125 = DIRECTION ( 'NONE',  ( -0.000000000000000000, 1.000000000000000000, -0.000000000000000000 ) ) ;
#13126 = MECHANICAL_DESIGN_GEOMETRIC_PRESENTATION_REPRESENTATION (  '', ( #46045 ), #42776 ) ;
#13127 = VERTEX_POINT ( 'NONE', #11790 ) ;
#13128 = CARTESIAN_POINT ( 'NONE',  ( 1.363819533518803251, 3.267716535433071279, -2.365849761790805487E-16 ) ) ;
#13129 = CARTESIAN_POINT ( 'NONE',  ( -1.798309077365525477, 1.584767851350155743, -1.651272990452771872 ) ) ;
#13130 = CARTESIAN_POINT ( 'NONE',  ( 0.000000000000000000, 1.574803149606302854, 0.000000000000000000 ) ) ;
#13131 = DIRECTION ( 'NONE',  ( -1.000000000000000000, 0.000000000000000000, -0.000000000000000000 ) ) ;
#13132 = VECTOR ( 'NONE', #22286, 39.37007874015748143 ) ;
#13133 = DIRECTION ( 'NONE',  ( 0.000000000000000000, 0.000000000000000000, -1.000000000000000000 ) ) ;
#13134 = EDGE_CURVE ( 'NONE', #46917, #33096, #23927, .T. ) ;
#13135 = DIRECTION ( 'NONE',  ( 1.000000000000000000, -0.000000000000000000, 0.000000000000000000 ) ) ;
#13136 = CARTESIAN_POINT ( 'NONE',  ( -2.600183657057300923, 0.000000000000000000, 1.399218491554123700 ) ) ;
#13137 = EDGE_LOOP ( 'NONE', ( #49535, #37804, #38985, #50264 ) ) ;
#13138 = LINE ( 'NONE', #37144, #36124 ) ;
#13139 = EDGE_CURVE ( 'NONE', #24845, #43525, #40194, .T. ) ;
#13140 = DIRECTION ( 'NONE',  ( -1.000000000000000000, -0.000000000000000000, -0.000000000000000000 ) ) ;
#13141 = ORIENTED_EDGE ( 'NONE', *, *, #25550, .T. ) ;
#13142 = CARTESIAN_POINT ( 'NONE',  ( 1.528535732727733132, 1.480350918634800728, 2.526383692155887317 ) ) ;
#13143 = EDGE_CURVE ( 'NONE', #14372, #40564, #8438, .T. ) ;
#13144 = ORIENTED_EDGE ( 'NONE', *, *, #34036, .T. ) ;
#13145 = LINE ( 'NONE', #13653, #19539 ) ;
#13146 = EDGE_CURVE ( 'NONE', #45868, #39288, #4824, .T. ) ;
#13147 = CARTESIAN_POINT ( 'NONE',  ( -1.707223610577860429, 0.000000000000000000, -0.3728134436854625422 ) ) ;
#13148 = CARTESIAN_POINT ( 'NONE',  ( 0.2646829987306326126, 5.905511811023623991, -2.940868978332396910 ) ) ;
#13149 = CARTESIAN_POINT ( 'NONE',  ( 0.2727639067037610499, 0.000000000000000000, 2.047244094488179567 ) ) ;
#13150 = CARTESIAN_POINT ( 'NONE',  ( 2.106197740627111514, 3.223484195733438362, -1.279361934207793094 ) ) ;
#13151 = VECTOR ( 'NONE', #26107, 39.37007874015748143 ) ;
#13152 = ORIENTED_EDGE ( 'NONE', *, *, #32950, .T. ) ;
#13153 = DIRECTION ( 'NONE',  ( -0.000000000000000000, 1.000000000000000000, -0.000000000000000000 ) ) ;
#13154 = CARTESIAN_POINT ( 'NONE',  ( 1.636583440222563857, 0.000000000000000000, -0.6299212598425181220 ) ) ;
#13155 = B_SPLINE_CURVE_WITH_KNOTS ( 'NONE', 3,
 ( #48376, #37577, #9177, #33711 ),
 .UNSPECIFIED., .F., .F.,
 ( 4, 4 ),
 ( 0.1211873102087489551, 0.1625992483279400380 ),
 .UNSPECIFIED. ) ;
#13156 = ORIENTED_EDGE ( 'NONE', *, *, #20729, .F. ) ;
#13157 = CARTESIAN_POINT ( 'NONE',  ( 2.378961647330872786, 3.267716535433070391, 0.5584465239797037350 ) ) ;
#13158 = ORIENTED_EDGE ( 'NONE', *, *, #10551, .F. ) ;
#13159 = EDGE_CURVE ( 'NONE', #43500, #30156, #5310, .T. ) ;
#13160 = CONICAL_SURFACE ( 'NONE', #32140, 3.033577403570480779, 1.554780866114618743 ) ;
#13161 = CARTESIAN_POINT ( 'NONE',  ( -0.8942052331142547050, 0.000000000000000000, 1.259842519685033357 ) ) ;
#13162 = DIRECTION ( 'NONE',  ( 1.734723475976806848E-16, -0.000000000000000000, 1.000000000000000000 ) ) ;
#13163 = LINE ( 'NONE', #39304, #27356 ) ;
#13164 = EDGE_CURVE ( 'NONE', #49043, #30631, #943, .T. ) ;
#13165 = CARTESIAN_POINT ( 'NONE',  ( -1.636583440222564301, 3.346456692913386100, -0.6299212598425177889 ) ) ;
#13166 = ADVANCED_FACE ( 'NONE', ( #4304 ), #35804, .F. ) ;
#13167 = EDGE_LOOP ( 'NONE', ( #30267, #2253, #17066, #15549 ) ) ;
#13168 = EDGE_LOOP ( 'NONE', ( #1791, #36235, #26921, #27053 ) ) ;
#13169 = CARTESIAN_POINT ( 'NONE',  ( 0.07982360342473591996, 1.709180471932028711, 0.000000000000000000 ) ) ;
#13170 = CARTESIAN_POINT ( 'NONE',  ( -1.719272085561387442, 0.5247476050418645732, 1.308128460514559332 ) ) ;
#13171 = FACE_BOUND ( 'NONE', #11889, .T. ) ;
#13172 = ORIENTED_EDGE ( 'NONE', *, *, #40482, .T. ) ;
#13173 = AXIS2_PLACEMENT_3D ( 'NONE', #4690, #47243, #39542 ) ;
#13174 = CARTESIAN_POINT ( 'NONE',  ( 0.9439235339024302229, 1.657403817845428451, -2.073500882935703338 ) ) ;
#13175 = CARTESIAN_POINT ( 'NONE',  ( -1.195183497228115035E-16, 0.000000000000000000, -0.3149606299212591165 ) ) ;
#13176 = VERTEX_POINT ( 'NONE', #19786 ) ;
#13177 = ADVANCED_FACE ( 'NONE', ( #12562 ), #36704, .F. ) ;
#13178 = CARTESIAN_POINT ( 'NONE',  ( 0.000000000000000000, 3.267716535433071279, 0.000000000000000000 ) ) ;
#13179 = CARTESIAN_POINT ( 'NONE',  ( 1.892591856222374469, 0.05823298773025239322, -0.4824499329568616157 ) ) ;
#13180 = ORIENTED_EDGE ( 'NONE', *, *, #7278, .T. ) ;
#13181 = VERTEX_POINT ( 'NONE', #31942 ) ;
#13182 = ORIENTED_EDGE ( 'NONE', *, *, #23495, .T. ) ;
#13183 = CARTESIAN_POINT ( 'NONE',  ( -0.3486774197067339376, 3.267716535433071279, 1.209717811016579078E-16 ) ) ;
#13184 = DIRECTION ( 'NONE',  ( 0.000000000000000000, 0.000000000000000000, -1.000000000000000000 ) ) ;
#13185 = CONICAL_SURFACE ( 'NONE', #11517, 1.850107469027523210, 0.6386652850508578450 ) ;
#13186 = LINE ( 'NONE', #5694, #13526 ) ;
#13187 = EDGE_CURVE ( 'NONE', #35330, #39943, #47636, .T. ) ;
#13188 = LINE ( 'NONE', #12661, #1615 ) ;
#13189 = ORIENTED_EDGE ( 'NONE', *, *, #26379, .T. ) ;
#13190 = ORIENTED_EDGE ( 'NONE', *, *, #36496, .T. ) ;
#13191 = FACE_OUTER_BOUND ( 'NONE', #12287, .T. ) ;
#13192 = CARTESIAN_POINT ( 'NONE',  ( -0.6214413264104939882, 0.000000000000000000, 1.732283464566921172 ) ) ;
#13193 = CARTESIAN_POINT ( 'NONE',  ( 0.000000000000000000, 0.000000000000000000, 0.000000000000000000 ) ) ;
#13194 = DIRECTION ( 'NONE',  ( -1.156061316345072978E-16, -1.000000000000000000, -1.040474016969658122E-17 ) ) ;
#13195 = CARTESIAN_POINT ( 'NONE',  ( -1.439733046521777027, 3.267716535433071279, -1.771653543307080581 ) ) ;
#13196 = VECTOR ( 'NONE', #32497, 39.37007874015748143 ) ;
#13197 = B_SPLINE_CURVE_WITH_KNOTS ( 'NONE', 3,
 ( #38665, #34787, #19278, #27532 ),
 .UNSPECIFIED., .F., .F.,
 ( 4, 4 ),
 ( 0.03083869506961483056, 0.04878547865986578719 ),
 .UNSPECIFIED. ) ;
#13198 = EDGE_CURVE ( 'NONE', #14529, #23981, #32718, .T. ) ;
#13199 = DIRECTION ( 'NONE',  ( -0.000000000000000000, 1.000000000000000000, -0.000000000000000000 ) ) ;
#13200 = EDGE_CURVE ( 'NONE', #50651, #8216, #32974, .T. ) ;
#13201 = DIRECTION ( 'NONE',  ( -6.104789737168205836E-17, 1.000000000000000000, 1.134460028949762747E-16 ) ) ;
#13202 = EDGE_CURVE ( 'NONE', #24291, #16391, #9968, .T. ) ;
#13203 = ORIENTED_EDGE ( 'NONE', *, *, #35072, .F. ) ;
#13204 = LINE ( 'NONE', #33346, #11860 ) ;
#13205 = DIRECTION ( 'NONE',  ( 1.000000000000000000, 0.000000000000000000, 0.000000000000000000 ) ) ;
#13206 = AXIS2_PLACEMENT_3D ( 'NONE', #43155, #24062, #306 ) ;
#13207 = ORIENTED_EDGE ( 'NONE', *, *, #47657, .F. ) ;
#13208 = ORIENTED_EDGE ( 'NONE', *, *, #1730, .T. ) ;
#13209 = CARTESIAN_POINT ( 'NONE',  ( 0.000000000000000000, 3.267716535433071279, -0.5118110236220466680 ) ) ;
#13210 = CARTESIAN_POINT ( 'NONE',  ( 0.1968503937007870241, 3.346456692913386100, -2.204724409448811429 ) ) ;
#13211 = ORIENTED_EDGE ( 'NONE', *, *, #29110, .F. ) ;
#13212 = VERTEX_POINT ( 'NONE', #37599 ) ;
#13213 = LINE ( 'NONE', #21464, #47642 ) ;
#13214 = EDGE_CURVE ( 'NONE', #31073, #5934, #25600, .T. ) ;
#13215 = ORIENTED_EDGE ( 'NONE', *, *, #30270, .T. ) ;
#13216 = CARTESIAN_POINT ( 'NONE',  ( -0.07591351300297284610, 3.267716535433071279, 0.9055118110236167750 ) ) ;
#13217 = EDGE_CURVE ( 'NONE', #11147, #22241, #24949, .T. ) ;
#13218 = CARTESIAN_POINT ( 'NONE',  ( -1.909347346926324906, 0.000000000000000000, -0.6692913385826758654 ) ) ;
#13219 = EDGE_CURVE ( 'NONE', #14807, #45414, #41462, .T. ) ;
#13220 = VERTEX_POINT ( 'NONE', #1967 ) ;
#13221 = EDGE_LOOP ( 'NONE', ( #24473, #21167, #3880, #36325 ) ) ;
#13222 = ORIENTED_EDGE ( 'NONE', *, *, #41580, .T. ) ;
#13223 = DIRECTION ( 'NONE',  ( -0.000000000000000000, 0.000000000000000000, 1.000000000000000000 ) ) ;
#13224 = EDGE_CURVE ( 'NONE', #596, #19294, #25078, .T. ) ;
#13226 = ORIENTED_EDGE ( 'NONE', *, *, #25031, .T. ) ;
#13225 = EDGE_CURVE ( 'NONE', #49804, #27786, #25711, .T. ) ;
#13227 = EDGE_LOOP ( 'NONE', ( #15513, #42523, #265, #38423 ) ) ;
#13228 = DIRECTION ( 'NONE',  ( 1.734723475976806848E-16, -0.000000000000000000, 1.000000000000000000 ) ) ;
#13229 = CARTESIAN_POINT ( 'NONE',  ( 0.000000000000000000, 2.755905511811023612, 0.000000000000000000 ) ) ;
#13230 = CARTESIAN_POINT ( 'NONE',  ( 2.222091332265985208, 1.743492810207595500, 0.6702560524809636489 ) ) ;
#13231 = VECTOR ( 'NONE', #49707, 39.37007874015748143 ) ;
#13232 = EDGE_LOOP ( 'NONE', ( #29248, #41686, #13432, #48802 ) ) ;
#13233 = VECTOR ( 'NONE', #19442, 39.37007874015748143 ) ;
#13234 = CARTESIAN_POINT ( 'NONE',  ( 0.01640433704663615821, 1.719511132758201999, 2.952755905511811108 ) ) ;
#13235 = DIRECTION ( 'NONE',  ( 0.8660254037844431485, 0.000000000000000000, 0.4999999999999918954 ) ) ;
#13236 = CARTESIAN_POINT ( 'NONE',  ( 1.854898449969132335, 1.741084675012395833, -1.705377970569586621 ) ) ;
#13237 = ORIENTED_EDGE ( 'NONE', *, *, #27058, .T. ) ;
#13238 = CARTESIAN_POINT ( 'NONE',  ( 1.929629134066521701, 6.692913385826772199, 0.9824921284572420976 ) ) ;
#13239 = CARTESIAN_POINT ( 'NONE',  ( -0.2727639067037607723, 0.000000000000000000, -0.4724409448818883694 ) ) ;
#13240 = CARTESIAN_POINT ( 'NONE',  ( 1.363819533518803251, 3.267716535433071279, -0.6692913385826764205 ) ) ;
#13241 = EDGE_LOOP ( 'NONE', ( #24345, #7431, #1146, #15564 ) ) ;
#13242 = ORIENTED_EDGE ( 'NONE', *, *, #14068, .F. ) ;
#13243 = VECTOR ( 'NONE', #43607, 39.37007874015748143 ) ;
#13244 = LINE ( 'NONE', #43690, #28728 ) ;
#13245 =( CONVERSION_BASED_UNIT ( 'INCH', #13494 ) LENGTH_UNIT ( ) NAMED_UNIT ( #16241 ) );
#13246 = PLANE ( 'NONE',  #50247 ) ;
#13247 = DIRECTION ( 'NONE',  ( 0.000000000000000000, -1.000000000000000000, 0.000000000000000000 ) ) ;
#13248 = DIRECTION ( 'NONE',  ( 0.8345732537212999791, -6.397775707690033618E-17, 0.5508969814521065267 ) ) ;
#13249 = VERTEX_POINT ( 'NONE', #33480 ) ;
#13250 = VERTEX_POINT ( 'NONE', #22102 ) ;
#13251 = CARTESIAN_POINT ( 'NONE',  ( -1.478009596860490715, 1.585803725363800210, 1.616919955472289727 ) ) ;
#13252 = ORIENTED_EDGE ( 'NONE', *, *, #40325, .T. ) ;
#13253 = CARTESIAN_POINT ( 'NONE',  ( 0.000000000000000000, 3.267716535433071279, 0.7874015748031456541 ) ) ;
#13254 = CARTESIAN_POINT ( 'NONE',  ( -0.2727639067037605503, 3.267716535433071279, 4.731699523581609125E-17 ) ) ;
#13255 = DIRECTION ( 'NONE',  ( -0.000000000000000000, 1.000000000000000000, 0.000000000000000000 ) ) ;
#13256 = EDGE_CURVE ( 'NONE', #49170, #33914, #37859, .T. ) ;
#13257 = DIRECTION ( 'NONE',  ( 2.866708903754326305E-17, 1.000000000000000000, 1.255987235303924321E-16 ) ) ;
#13258 = LINE ( 'NONE', #25377, #8106 ) ;
#13259 = ORIENTED_EDGE ( 'NONE', *, *, #18585, .F. ) ;
#13260 = ADVANCED_FACE ( 'NONE', ( #49418 ), #9718, .F. ) ;
#13261 = DIRECTION ( 'NONE',  ( 1.734723475976806848E-16, -0.000000000000000000, 1.000000000000000000 ) ) ;
#13262 = CARTESIAN_POINT ( 'NONE',  ( 1.363819533518803251, 3.267716535433071279, -2.365849761790805487E-16 ) ) ;
#13263 = EDGE_CURVE ( 'NONE', #10495, #32762, #6088, .T. ) ;
#13264 = B_SPLINE_CURVE_WITH_KNOTS ( 'NONE', 3,
 ( #18518, #14644, #30389, #34522 ),
 .UNSPECIFIED., .F., .F.,
 ( 4, 4 ),
 ( 0.0005256063878724909297, 0.003025860639318088061 ),
 .UNSPECIFIED. ) ;
#13265 = VECTOR ( 'NONE', #13135, 39.37007874015748143 ) ;
#13266 = ORIENTED_EDGE ( 'NONE', *, *, #15630, .T. ) ;
#13267 = CARTESIAN_POINT ( 'NONE',  ( -2.074049943651441019, 6.692913385826772199, 0.6221544894623932676 ) ) ;
#13268 = VECTOR ( 'NONE', #42670, 39.37007874015748143 ) ;
#13269 = CARTESIAN_POINT ( 'NONE',  ( -1.909347346926324462, 0.000000000000000000, 0.2755905511810996522 ) ) ;
#13270 = DIRECTION ( 'NONE',  ( 1.000000000000000000, -0.000000000000000000, 0.000000000000000000 ) ) ;
#13271 = ORIENTED_EDGE ( 'NONE', *, *, #43846, .T. ) ;
#13272 = CARTESIAN_POINT ( 'NONE',  ( 1.909347346926324684, 0.000000000000000000, 0.5905511811023582691 ) ) ;
#13273 = DIRECTION ( 'NONE',  ( 0.01601477604151182663, -0.9998717552508123996, 0.000000000000000000 ) ) ;
#13274 = VERTEX_POINT ( 'NONE', #21078 ) ;
#13275 = LINE ( 'NONE', #29007, #42810 ) ;
#13276 = AXIS2_PLACEMENT_3D ( 'NONE', #20842, #36595, #36851 ) ;
#13277 = FACE_OUTER_BOUND ( 'NONE', #1212, .T. ) ;
#13278 = ORIENTED_EDGE ( 'NONE', *, *, #31878, .F. ) ;
#13279 = CARTESIAN_POINT ( 'NONE',  ( -2.082617625631827174, 3.267716535433071279, -0.3149606299212589500 ) ) ;
#13280 = CARTESIAN_POINT ( 'NONE',  ( -1.636583440222563635, 0.000000000000000000, -4.780733988912460139E-16 ) ) ;
#13281 = EDGE_CURVE ( 'NONE', #38547, #6492, #1453, .T. ) ;
#13282 = FACE_OUTER_BOUND ( 'NONE', #14231, .T. ) ;
#13283 = CARTESIAN_POINT ( 'NONE',  ( -0.6235241006192322466, 1.205361022782829114E-17, 2.074304693190349269 ) ) ;
#13284 = CARTESIAN_POINT ( 'NONE',  ( -1.909347346926324462, 3.267716535433071279, 3.312189666507127188E-16 ) ) ;
#13285 = EDGE_LOOP ( 'NONE', ( #49756, #22932, #2439, #15571 ) ) ;
#13286 = VERTEX_POINT ( 'NONE', #17209 ) ;
#13287 = DIRECTION ( 'NONE',  ( -0.01601477604151182663, 0.9998717552508123996, -0.000000000000000000 ) ) ;
#13288 = LINE ( 'NONE', #17160, #38647 ) ;
#13289 = EDGE_CURVE ( 'NONE', #7776, #22612, #44808, .T. ) ;
#13290 = ORIENTED_EDGE ( 'NONE', *, *, #50604, .T. ) ;
#13291 = DIRECTION ( 'NONE',  ( -0.000000000000000000, 1.000000000000000000, -0.000000000000000000 ) ) ;
#13292 = CARTESIAN_POINT ( 'NONE',  ( 0.000000000000000000, 3.267716535433071279, -1.141732283464563791 ) ) ;
#13293 = DIRECTION ( 'NONE',  ( -3.469446951953613696E-16, 0.000000000000000000, -1.000000000000000000 ) ) ;
#13295 = CARTESIAN_POINT ( 'NONE',  ( 0.000000000000000000, 3.346456692913386100, 0.000000000000000000 ) ) ;
#13294 = B_SPLINE_CURVE_WITH_KNOTS ( 'NONE', 3,
 ( #14180, #14439, #12024, #11515 ),
 .UNSPECIFIED., .F., .F.,
 ( 4, 4 ),
 ( 0.02644966475140674358, 0.02714458517981072419 ),
 .UNSPECIFIED. ) ;
#13296 = ORIENTED_EDGE ( 'NONE', *, *, #47739, .T. ) ;
#13297 = ORIENTED_EDGE ( 'NONE', *, *, #10298, .T. ) ;
#13298 = CARTESIAN_POINT ( 'NONE',  ( -1.636583440222563635, 3.346456692913386100, 0.3149606299212578953 ) ) ;
#13299 = LINE ( 'NONE', #10181, #6854 ) ;
#13300 = CARTESIAN_POINT ( 'NONE',  ( -0.3486774197067339376, 3.346456692913386100, 0.3149606299212577287 ) ) ;
#13301 = VERTEX_POINT ( 'NONE', #5585 ) ;
#13302 = CARTESIAN_POINT ( 'NONE',  ( 1.953585199828835606, 3.346456692913386100, -0.7874015748031474304 ) ) ;
#13303 = FACE_BOUND ( 'NONE', #32336, .T. ) ;
#13304 = VERTEX_POINT ( 'NONE', #21337 ) ;
#13305 = DIRECTION ( 'NONE',  ( 1.000000000000000000, -0.000000000000000000, 0.000000000000000000 ) ) ;
#13306 = VERTEX_POINT ( 'NONE', #10222 ) ;
#13307 = EDGE_LOOP ( 'NONE', ( #28269, #49538, #42739, #23995 ) ) ;
#13308 = CARTESIAN_POINT ( 'NONE',  ( -0.6214413264104939882, 3.267716535433071279, 0.5905511811023582691 ) ) ;
#13309 = VECTOR ( 'NONE', #37336, 39.37007874015748854 ) ;
#13310 = AXIS2_PLACEMENT_3D ( 'NONE', #48420, #9225, #37112 ) ;
#13311 = ORIENTED_EDGE ( 'NONE', *, *, #31051, .F. ) ;
#13312 = FACE_OUTER_BOUND ( 'NONE', #22302, .T. ) ;
#13313 = DIRECTION ( 'NONE',  ( -0.000000000000000000, 1.000000000000000000, -0.000000000000000000 ) ) ;
#13314 = VERTEX_POINT ( 'NONE', #1709 ) ;
#13315 = AXIS2_PLACEMENT_3D ( 'NONE', #24907, #39888, #12783 ) ;
#13316 = CARTESIAN_POINT ( 'NONE',  ( 0.08139965876239094178, 1.610780518492231694, 0.000000000000000000 ) ) ;
#13317 = DIRECTION ( 'NONE',  ( -1.000000000000000000, 0.000000000000000000, -0.000000000000000000 ) ) ;
#13318 = CARTESIAN_POINT ( 'NONE',  ( -1.321932112650661351, 0.002299539184349054001, -1.195809976494780047 ) ) ;
#13319 = VECTOR ( 'NONE', #34032, 39.37007874015748143 ) ;
#13320 = CARTESIAN_POINT ( 'NONE',  ( -0.8182917201112819283, 0.000000000000000000, -0.7874015748031467643 ) ) ;
#13321 = EDGE_CURVE ( 'NONE', #12193, #30195, #33221, .T. ) ;
#13322 = DIRECTION ( 'NONE',  ( -0.000000000000000000, 1.000000000000000000, -0.000000000000000000 ) ) ;
#13323 = CARTESIAN_POINT ( 'NONE',  ( 0.04921259842519667971, 1.708690180665275005, 2.244725876464058523 ) ) ;
#13324 = ORIENTED_EDGE ( 'NONE', *, *, #12320, .T. ) ;
#13325 = EDGE_CURVE ( 'NONE', #9488, #21677, #17797, .T. ) ;
#13326 = CARTESIAN_POINT ( 'NONE',  ( -0.3486774197067334935, 3.267716535433071279, 0.4330708661417290162 ) ) ;
#13327 = CARTESIAN_POINT ( 'NONE',  ( 2.951990591674675368, 1.666783180044518087, -0.08331184815398359755 ) ) ;
#13328 = EDGE_CURVE ( 'NONE', #10750, #1759, #29327, .T. ) ;
#13329 = ORIENTED_EDGE ( 'NONE', *, *, #42519, .F. ) ;
#13330 = FACE_OUTER_BOUND ( 'NONE', #47917, .T. ) ;
#13331 = CARTESIAN_POINT ( 'NONE',  ( 0.7423782071083084855, 3.346456692913386100, -1.574803149606293529 ) ) ;
#13332 = VERTEX_POINT ( 'NONE', #21588 ) ;
#13333 = CARTESIAN_POINT ( 'NONE',  ( 0.1968503937007871074, 3.267716535433071279, -6.829619984160646953E-17 ) ) ;
#13334 = DIRECTION ( 'NONE',  ( -1.000000000000000000, 0.000000000000000000, -0.000000000000000000 ) ) ;
#13335 = CARTESIAN_POINT ( 'NONE',  ( 1.973323729629757217, 0.000000000000000000, -0.7899196136953162695 ) ) ;
#13336 = ORIENTED_EDGE ( 'NONE', *, *, #30233, .T. ) ;
#13337 = CARTESIAN_POINT ( 'NONE',  ( -0.2727639067037602172, 0.000000000000000000, 1.102362204724404160 ) ) ;
#13338 = ORIENTED_EDGE ( 'NONE', *, *, #23286, .F. ) ;
#13339 = FACE_BOUND ( 'NONE', #23314, .T. ) ;
#13340 = FACE_OUTER_BOUND ( 'NONE', #15658, .T. ) ;
#13341 = VECTOR ( 'NONE', #31603, 39.37007874015748143 ) ;
#13342 = CONICAL_SURFACE ( 'NONE', #3414, 2.244934639244524632, 1.554780866114618743 ) ;
#13343 = CARTESIAN_POINT ( 'NONE',  ( -0.5455278134075217666, 3.240372690294659908, -2.395036701391033862 ) ) ;
#13344 = EDGE_CURVE ( 'NONE', #2567, #48435, #18976, .T. ) ;
#13345 = CARTESIAN_POINT ( 'NONE',  ( 1.909347346926324684, 3.267716535433071279, -3.312189666507128175E-16 ) ) ;
#13346 = AXIS2_PLACEMENT_3D ( 'NONE', #41786, #22672, #41283 ) ;
#13347 = EDGE_LOOP ( 'NONE', ( #11051, #33886, #22625, #50738 ) ) ;
#13348 = ORIENTED_EDGE ( 'NONE', *, *, #1617, .T. ) ;
#13349 = DIRECTION ( 'NONE',  ( 1.000000000000000000, 0.000000000000000000, -3.469446951953613696E-16 ) ) ;
#13350 = ORIENTED_EDGE ( 'NONE', *, *, #18421, .T. ) ;
#13351 = ADVANCED_FACE ( 'NONE', ( #7610 ), #6853, .F. ) ;
#13352 = AXIS2_PLACEMENT_3D ( 'NONE', #8975, #36090, #1481 ) ;
#13353 = CARTESIAN_POINT ( 'NONE',  ( -2.867773316779184789, 5.905511811023623991, -0.7050287376752433222 ) ) ;
#13354 = EDGE_LOOP ( 'NONE', ( #32537, #39516, #24268, #1586 ) ) ;
#13355 = DIRECTION ( 'NONE',  ( -3.324886662288880100E-16, 5.168407336632174847E-17, 1.000000000000000000 ) ) ;
#13356 = VECTOR ( 'NONE', #19151, 39.37007874015748143 ) ;
#13357 = EDGE_LOOP ( 'NONE', ( #28551, #48967, #26198, #19905 ) ) ;
#13358 = LINE ( 'NONE', #41991, #31535 ) ;
#13359 = LINE ( 'NONE', #9484, #20693 ) ;
#13360 = EDGE_LOOP ( 'NONE', ( #9885, #21696, #7696, #31786, #39811, #17185, #17259, #32681, #45301, #36860, #48015 ) ) ;
#13361 = DIRECTION ( 'NONE',  ( 1.000000000000000000, 0.000000000000000000, 0.000000000000000000 ) ) ;
#13362 = ORIENTED_EDGE ( 'NONE', *, *, #31887, .T. ) ;
#13363 = EDGE_LOOP ( 'NONE', ( #18816, #11466, #44015, #18736 ) ) ;
#13364 = EDGE_CURVE ( 'NONE', #21109, #41720, #10391, .T. ) ;
#13365 = ORIENTED_EDGE ( 'NONE', *, *, #27668, .F. ) ;
#13366 = ORIENTED_EDGE ( 'NONE', *, *, #37683, .T. ) ;
#13367 = CARTESIAN_POINT ( 'NONE',  ( 0.7423782071083087075, 3.267716535433071279, -2.575641807848710194E-16 ) ) ;
#13368 = EDGE_LOOP ( 'NONE', ( #31237, #18701, #3301, #5286 ) ) ;
#13369 = CARTESIAN_POINT ( 'NONE',  ( 0.8182917201112817063, 0.000000000000000000, -1.417322834645664331 ) ) ;
#13370 = ORIENTED_EDGE ( 'NONE', *, *, #3579, .F. ) ;
#13371 = FACE_OUTER_BOUND ( 'NONE', #16908, .T. ) ;
#13372 = VECTOR ( 'NONE', #13997, 39.37007874015748143 ) ;
#13373 = DIRECTION ( 'NONE',  ( -1.000000000000000000, 0.000000000000000000, -0.000000000000000000 ) ) ;
#13374 = ORIENTED_EDGE ( 'NONE', *, *, #41782, .F. ) ;
#13375 = VECTOR ( 'NONE', #13410, 39.37007874015748143 ) ;
#13376 = PLANE ( 'NONE',  #39305 ) ;
#13377 = CARTESIAN_POINT ( 'NONE',  ( -1.215880257433763489, 0.002872929996209854387, 1.316888785179493482 ) ) ;
#13378 = ORIENTED_EDGE ( 'NONE', *, *, #32735, .F. ) ;
#13379 = CARTESIAN_POINT ( 'NONE',  ( 0.3382312733057609155, 5.905511811023623991, -2.139420919314965808 ) ) ;
#13380 = CARTESIAN_POINT ( 'NONE',  ( 1.152895553066221934, 1.205361022782829114E-17, -1.833672301139072092 ) ) ;
#13381 = DIRECTION ( 'NONE',  ( -0.000000000000000000, 0.000000000000000000, 1.000000000000000000 ) ) ;
#13382 = CARTESIAN_POINT ( 'NONE',  ( 0.4696143004045479352, 0.000000000000000000, 0.1574803149606283648 ) ) ;
#13383 = ADVANCED_FACE ( 'NONE', ( #15104 ), #34481, .F. ) ;
#13384 = VECTOR ( 'NONE', #4688, 39.37007874015748143 ) ;
#13385 = DIRECTION ( 'NONE',  ( 0.000000000000000000, 0.000000000000000000, -1.000000000000000000 ) ) ;
#13386 = ADVANCED_FACE ( 'NONE', ( #30860 ), #22354, .F. ) ;
#13387 = EDGE_LOOP ( 'NONE', ( #42183, #39207, #43597, #11747, #845, #32123, #11933, #40354, #32770, #11054, #46781 ) ) ;
#13388 = CARTESIAN_POINT ( 'NONE',  ( -1.712496953225537633, 3.267716535433071279, 1.325184350462985883 ) ) ;
#13389 = ADVANCED_FACE ( 'NONE', ( #10478 ), #14348, .F. ) ;
#13390 = CARTESIAN_POINT ( 'NONE',  ( -0.07591351300297340121, 3.267716535433071279, -0.6692913385826758654 ) ) ;
#13391 = VERTEX_POINT ( 'NONE', #15360 ) ;
#13392 = CARTESIAN_POINT ( 'NONE',  ( 2.069629837364519886, 3.267716535433071279, -1.299212598425194320 ) ) ;
#13393 = ORIENTED_EDGE ( 'NONE', *, *, #26298, .F. ) ;
#13394 = DIRECTION ( 'NONE',  ( 0.000000000000000000, 1.000000000000000000, 0.000000000000000000 ) ) ;
#13395 = CARTESIAN_POINT ( 'NONE',  ( 0.5455278134075217666, 0.000000000000000000, 1.889763779527550369 ) ) ;
#13396 = CARTESIAN_POINT ( 'NONE',  ( 0.000000000000000000, 3.267716535433071279, 0.4330708661417290162 ) ) ;
#13397 = DIRECTION ( 'NONE',  ( 0.000000000000000000, 0.000000000000000000, -1.000000000000000000 ) ) ;
#13398 = EDGE_CURVE ( 'NONE', #2602, #48050, #50415, .T. ) ;
#13399 = CARTESIAN_POINT ( 'NONE',  ( -2.165354330708661568, 1.574803149606301966, 0.08080958537891422266 ) ) ;
#13400 = VERTEX_POINT ( 'NONE', #30604 ) ;
#13401 = CARTESIAN_POINT ( 'NONE',  ( 0.5455278134075211005, 3.267716535433071279, -9.463399047163219482E-17 ) ) ;
#13402 = FACE_BOUND ( 'NONE', #29833, .T. ) ;
#13403 = VERTEX_POINT ( 'NONE', #19221 ) ;
#13404 = DIRECTION ( 'NONE',  ( -1.156061316345074457E-16, -1.000000000000000000, 1.040474016969491568E-17 ) ) ;
#13405 = ORIENTED_EDGE ( 'NONE', *, *, #26204, .T. ) ;
#13406 = DIRECTION ( 'NONE',  ( -1.000000000000000000, 0.000000000000000000, -0.000000000000000000 ) ) ;
#13407 = CARTESIAN_POINT ( 'NONE',  ( -0.2156685157583834722, 0.000000000000000000, -2.945280361644576850 ) ) ;
#13408 = AXIS2_PLACEMENT_3D ( 'NONE', #40794, #5683, #41812 ) ;
#13409 = EDGE_CURVE ( 'NONE', #16156, #4725, #42958, .T. ) ;
#13410 = DIRECTION ( 'NONE',  ( 1.734723475976806848E-16, -0.000000000000000000, 1.000000000000000000 ) ) ;
#13411 = CIRCLE ( 'NONE', #47967, 2.165354330708661568 ) ;
#13412 = CARTESIAN_POINT ( 'NONE',  ( -1.363819533518803029, 3.267716535433071279, 1.102362204724404160 ) ) ;
#13413 = VERTEX_POINT ( 'NONE', #11488 ) ;
#13414 = ORIENTED_EDGE ( 'NONE', *, *, #46296, .F. ) ;
#13415 = DIRECTION ( 'NONE',  ( -0.000000000000000000, 1.000000000000000000, -0.000000000000000000 ) ) ;
#13417 = CARTESIAN_POINT ( 'NONE',  ( -2.029281105070185109, 1.044437984162145394, 1.555352403886350432 ) ) ;
#13416 = AXIS2_PLACEMENT_3D ( 'NONE', #32613, #849, #48047 ) ;
#13418 = FACE_BOUND ( 'NONE', #37453, .T. ) ;
#13419 = VERTEX_POINT ( 'NONE', #41971 ) ;
#13420 = ADVANCED_FACE ( 'NONE', ( #46566 ), #44167, .T. ) ;
#13421 = CONICAL_SURFACE ( 'NONE', #27398, 2.165354330708661568, 0.2617993877991570129 ) ;
#13422 = AXIS2_PLACEMENT_3D ( 'NONE', #29180, #32565, #20667 ) ;
#13423 = DIRECTION ( 'NONE',  ( 1.000000000000000000, 0.000000000000000000, 0.000000000000000000 ) ) ;
#13424 = DIRECTION ( 'NONE',  ( -3.469446951953613696E-16, 0.000000000000000000, -1.000000000000000000 ) ) ;
#13425 = ORIENTED_EDGE ( 'NONE', *, *, #37145, .T. ) ;
#13426 = B_SPLINE_CURVE_WITH_KNOTS ( 'NONE', 3,
 ( #41412, #32923, #33683, #25156 ),
 .UNSPECIFIED., .F., .F.,
 ( 4, 4 ),
 ( 0.0005438425946845861902, 0.0009539043374978324087 ),
 .UNSPECIFIED. ) ;
#13427 = CARTESIAN_POINT ( 'NONE',  ( -0.8182917201112819283, 3.346456692913386100, -2.047244094488181343 ) ) ;
#13428 =( REPRESENTATION_RELATIONSHIP ('NONE','NONE', #50198, #8330 ) REPRESENTATION_RELATIONSHIP_WITH_TRANSFORMATION ( #23765 )SHAPE_REPRESENTATION_RELATIONSHIP( ) );
#13429 = CARTESIAN_POINT ( 'NONE',  ( 0.1968503937007873017, 0.000000000000000000, -0.6299212598425177889 ) ) ;
#13430 = EDGE_CURVE ( 'NONE', #18373, #23227, #34983, .T. ) ;
#13431 = ORIENTED_EDGE ( 'NONE', *, *, #3585, .F. ) ;
#13432 = ORIENTED_EDGE ( 'NONE', *, *, #43544, .F. ) ;
#13434 = EDGE_CURVE ( 'NONE', #19538, #28015, #10979, .T. ) ;
#13433 = ORIENTED_EDGE ( 'NONE', *, *, #11208, .F. ) ;
#13435 = DIRECTION ( 'NONE',  ( 1.000000000000000000, 0.000000000000000000, -3.469446951953613696E-16 ) ) ;
#13436 = CARTESIAN_POINT ( 'NONE',  ( -2.708695948734475500, 1.570819970757063144, -1.175586072237004176 ) ) ;
#13437 = DIRECTION ( 'NONE',  ( -1.000000000000000000, 0.000000000000000000, 1.734723475976806848E-16 ) ) ;
#13438 = LINE ( 'NONE', #9565, #39528 ) ;
#13439 = EDGE_LOOP ( 'NONE', ( #24708, #10887, #47350, #15561 ) ) ;
#13440 = ORIENTED_EDGE ( 'NONE', *, *, #43095, .T. ) ;
#13441 = CARTESIAN_POINT ( 'NONE',  ( 1.363819533518803029, 0.000000000000000000, -1.732283464566923170 ) ) ;
#13442 = SURFACE_STYLE_USAGE ( .BOTH. , #1305 ) ;
#13443 = PLANE ( 'NONE',  #36536 ) ;
#13444 = B_SPLINE_CURVE_WITH_KNOTS ( 'NONE', 3,
 ( #35838, #465, #24734, #16477 ),
 .UNSPECIFIED., .F., .F.,
 ( 4, 4 ),
 ( 0.01165461794221865459, 0.03073677718705081913 ),
 .UNSPECIFIED. ) ;
#13445 = PLANE ( 'NONE',  #41640 ) ;
#13446 = CARTESIAN_POINT ( 'NONE',  ( -0.1204783766914112736, 0.008687915765946812099, -1.887631293257881815 ) ) ;
#13447 = EDGE_CURVE ( 'NONE', #23374, #3253, #42718, .T. ) ;
#13448 = LINE ( 'NONE', #29186, #2870 ) ;
#13449 = EDGE_CURVE ( 'NONE', #48162, #14514, #45876, .T. ) ;
#13450 = EDGE_CURVE ( 'NONE', #5207, #3630, #2725, .T. ) ;
#13451 = CARTESIAN_POINT ( 'NONE',  ( -1.181102362204724088, 0.5905511811023621549, 1.181102362204724088 ) ) ;
#13452 = AXIS2_PLACEMENT_3D ( 'NONE', #37308, #49126, #33184 ) ;
#13453 = ORIENTED_EDGE ( 'NONE', *, *, #13049, .F. ) ;
#13454 = CARTESIAN_POINT ( 'NONE',  ( -1.091055626815042201, 3.346456692913386100, 0.4330708661417290162 ) ) ;
#13455 = CYLINDRICAL_SURFACE ( 'NONE', #39227, 2.164630168518208109 ) ;
#13456 = ORIENTED_EDGE ( 'NONE', *, *, #4411, .F. ) ;
#13457 = AXIS2_PLACEMENT_3D ( 'NONE', #8277, #8533, #13184 ) ;
#13458 = ORIENTED_EDGE ( 'NONE', *, *, #38599, .F. ) ;
#13459 = VECTOR ( 'NONE', #44853, 39.37007874015748143 ) ;
#13460 = CARTESIAN_POINT ( 'NONE',  ( 1.909347346926324684, 3.267716535433071279, 0.4724409448818868706 ) ) ;
#13461 = DIRECTION ( 'NONE',  ( 1.000000000000000000, 0.000000000000000000, -3.469446951953613696E-16 ) ) ;
#13462 = EDGE_LOOP ( 'NONE', ( #9380, #1511, #45440, #2681 ) ) ;
#13463 = VECTOR ( 'NONE', #23146, 39.37007874015748143 ) ;
#13464 = ORIENTED_EDGE ( 'NONE', *, *, #22081, .T. ) ;
#13465 = DIRECTION ( 'NONE',  ( -0.000000000000000000, 0.000000000000000000, 1.000000000000000000 ) ) ;
#13466 = VERTEX_POINT ( 'NONE', #31111 ) ;
#13467 = FACE_OUTER_BOUND ( 'NONE', #24199, .T. ) ;
#13468 = DIRECTION ( 'NONE',  ( -3.469446951953613696E-16, 0.000000000000000000, -1.000000000000000000 ) ) ;
#13469 = EDGE_CURVE ( 'NONE', #33133, #25081, #26050, .T. ) ;
#13470 = ORIENTED_EDGE ( 'NONE', *, *, #40455, .F. ) ;
#13471 = ORIENTED_EDGE ( 'NONE', *, *, #22572, .T. ) ;
#13472 = VERTEX_POINT ( 'NONE', #42213 ) ;
#13473 = DIRECTION ( 'NONE',  ( 1.000000000000000000, 0.000000000000000000, 0.000000000000000000 ) ) ;
#13474 = VERTEX_POINT ( 'NONE', #22602 ) ;
#13475 = ORIENTED_EDGE ( 'NONE', *, *, #36811, .F. ) ;
#13476 = CARTESIAN_POINT ( 'NONE',  ( -0.07591351300297333182, 0.000000000000000000, 0.1574803149606283648 ) ) ;
#13477 = DIRECTION ( 'NONE',  ( -0.000000000000000000, -1.000000000000000000, -0.000000000000000000 ) ) ;
#13478 = CARTESIAN_POINT ( 'NONE',  ( 0.7937023274952557106, 0.02690111800290191299, -1.761563333612303106 ) ) ;
#13479 = ADVANCED_FACE ( 'NONE', ( #38357 ), #33831, .F. ) ;
#13480 = VERTEX_POINT ( 'NONE', #14453 ) ;
#13481 = EDGE_CURVE ( 'NONE', #26976, #2475, #17560, .T. ) ;
#13482 = DIRECTION ( 'NONE',  ( 0.000000000000000000, 0.000000000000000000, 1.000000000000000000 ) ) ;
#13483 = CARTESIAN_POINT ( 'NONE',  ( 0.000000000000000000, 2.755905511811022723, 0.000000000000000000 ) ) ;
#13484 = DIRECTION ( 'NONE',  ( 1.734723475976806848E-16, -0.000000000000000000, 1.000000000000000000 ) ) ;
#13485 = EDGE_CURVE ( 'NONE', #42097, #38291, #29943, .T. ) ;
#13486 = ORIENTED_EDGE ( 'NONE', *, *, #7381, .F. ) ;
#13487 = CARTESIAN_POINT ( 'NONE',  ( -2.055928985459924530, 6.692913385826772199, 0.7197570096327609024 ) ) ;
#13488 = VECTOR ( 'NONE', #28130, 39.37007874015748143 ) ;
#13489 = DIRECTION ( 'NONE',  ( -0.000000000000000000, 1.000000000000000000, -0.000000000000000000 ) ) ;
#13490 = DIRECTION ( 'NONE',  ( 1.734723475976806848E-16, -0.000000000000000000, 1.000000000000000000 ) ) ;
#13491 = ORIENTED_EDGE ( 'NONE', *, *, #44186, .F. ) ;
#13492 = VECTOR ( 'NONE', #37598, 39.37007874015748143 ) ;
#13493 = ORIENTED_EDGE ( 'NONE', *, *, #6929, .F. ) ;
#13494 = LENGTH_MEASURE_WITH_UNIT ( LENGTH_MEASURE( 0.02539999999999999897 ), #14002 );
#13495 = CIRCLE ( 'NONE', #5231, 2.106299212598425008 ) ;
#13496 = AXIS2_PLACEMENT_3D ( 'NONE', #21763, #48826, #21505 ) ;
#13497 = PLANE ( 'NONE',  #38763 ) ;
#13498 = DIRECTION ( 'NONE',  ( -1.000000000000000000, 0.000000000000000000, 0.000000000000000000 ) ) ;
#13499 = CARTESIAN_POINT ( 'NONE',  ( -1.439733046521776583, 3.267716535433071279, -1.259842519685034468 ) ) ;
#13500 = VERTEX_POINT ( 'NONE', #25814 ) ;
#13501 = ORIENTED_EDGE ( 'NONE', *, *, #28280, .T. ) ;
#13502 = VECTOR ( 'NONE', #30594, 39.37007874015748143 ) ;
#13503 = DIRECTION ( 'NONE',  ( -1.000000000000000000, 0.000000000000000000, -0.000000000000000000 ) ) ;
#13504 = ORIENTED_EDGE ( 'NONE', *, *, #5334, .T. ) ;
#13505 = LINE ( 'NONE', #17377, #48824 ) ;
#13506 = CARTESIAN_POINT ( 'NONE',  ( 2.437180031585944207, 1.459818316683583639, -1.667735833703099191 ) ) ;
#13507 = EDGE_CURVE ( 'NONE', #2179, #43511, #49884, .T. ) ;
#13508 = ADVANCED_FACE ( 'NONE', ( #17311 ), #30197, .F. ) ;
#13509 = ADVANCED_FACE ( 'NONE', ( #2322 ), #6453, .F. ) ;
#13510 = CARTESIAN_POINT ( 'NONE',  ( 2.932638728931774352, 1.666481914436860334, 0.3475908556738225297 ) ) ;
#13511 = DIRECTION ( 'NONE',  ( -3.469446951953613696E-16, 0.000000000000000000, -1.000000000000000000 ) ) ;
#13512 = CYLINDRICAL_SURFACE ( 'NONE', #37796, 2.165354330708661568 ) ;
#13513 = ORIENTED_EDGE ( 'NONE', *, *, #24415, .T. ) ;
#13514 = ADVANCED_FACE ( 'NONE', ( #37956 ), #33323, .F. ) ;
#13515 = DIRECTION ( 'NONE',  ( 0.000000000000000000, 0.000000000000000000, 1.000000000000000000 ) ) ;
#13516 = EDGE_CURVE ( 'NONE', #21275, #12193, #10071, .T. ) ;
#13517 = LINE ( 'NONE', #21005, #48738 ) ;
#13518 = ORIENTED_EDGE ( 'NONE', *, *, #29050, .T. ) ;
#13519 = LINE ( 'NONE', #21263, #35605 ) ;
#13520 = DIRECTION ( 'NONE',  ( 0.01601477604151182663, -0.9998717552508123996, 0.000000000000000000 ) ) ;
#13521 = DIRECTION ( 'NONE',  ( -0.000000000000000000, 1.000000000000000000, -0.000000000000000000 ) ) ;
#13522 = ORIENTED_EDGE ( 'NONE', *, *, #21282, .T. ) ;
#13523 = CARTESIAN_POINT ( 'NONE',  ( 1.723188456408574432, 1.574803149606302854, 1.311251662046225785 ) ) ;
#13524 = CARTESIAN_POINT ( 'NONE',  ( 2.106197740627111514, 0.000000000000000000, -1.102362204724406602 ) ) ;
#13525 = VECTOR ( 'NONE', #34955, 39.37007874015748143 ) ;
#13526 = VECTOR ( 'NONE', #8791, 39.37007874015748143 ) ;
#13527 = ORIENTED_EDGE ( 'NONE', *, *, #1908, .T. ) ;
#13528 = AXIS2_PLACEMENT_3D ( 'NONE', #28877, #1771, #1263 ) ;
#13529 = CARTESIAN_POINT ( 'NONE',  ( 2.808237744965994320, 0.000000000000000000, 0.9124517550441679781 ) ) ;
#13530 = CARTESIAN_POINT ( 'NONE',  ( 1.636583440222563857, 0.000000000000000000, 1.259842519685033135 ) ) ;
#13531 = EDGE_LOOP ( 'NONE', ( #18080, #30126, #48378, #41374 ) ) ;
#13532 = DIRECTION ( 'NONE',  ( -0.000000000000000000, 0.000000000000000000, 1.000000000000000000 ) ) ;
#13533 = VECTOR ( 'NONE', #38789, 39.37007874015748143 ) ;
#13534 = CIRCLE ( 'NONE', #42370, 2.164630168518208109 ) ;
#13535 = CARTESIAN_POINT ( 'NONE',  ( 1.287906020515829919, 3.346456692913386100, -1.666671669919371102 ) ) ;
#13536 = LINE ( 'NONE', #29271, #41190 ) ;
#13537 = CARTESIAN_POINT ( 'NONE',  ( 1.015142113812069535, 3.267716535433071279, -3.521981712565032882E-16 ) ) ;
#13538 = DIRECTION ( 'NONE',  ( 1.734723475976806848E-16, -0.000000000000000000, 1.000000000000000000 ) ) ;
#13539 = EDGE_LOOP ( 'NONE', ( #7937, #43437, #7961, #28212 ) ) ;
#13540 = ORIENTED_EDGE ( 'NONE', *, *, #26473, .T. ) ;
#13541 = LINE ( 'NONE', #29541, #28987 ) ;
#13542 = VECTOR ( 'NONE', #41584, 39.37007874015748143 ) ;
#13543 = CARTESIAN_POINT ( 'NONE',  ( -0.3486774197067334935, 0.000000000000000000, 0.4330708661417290162 ) ) ;
#13544 = VERTEX_POINT ( 'NONE', #37446 ) ;
#13545 = CARTESIAN_POINT ( 'NONE',  ( 1.287906020515830141, 0.000000000000000000, -0.3149606299212596716 ) ) ;
#13546 = DIRECTION ( 'NONE',  ( -3.469446951953613696E-16, 0.000000000000000000, -1.000000000000000000 ) ) ;
#13547 = CARTESIAN_POINT ( 'NONE',  ( 2.867773316779195447, 1.665472095473279790, -0.7050287376752005786 ) ) ;
#13548 = EDGE_LOOP ( 'NONE', ( #4977, #12077, #35369, #46918 ) ) ;
#13549 = ORIENTED_EDGE ( 'NONE', *, *, #2147, .T. ) ;
#13550 = ADVANCED_FACE ( 'NONE', ( #18075 ), #45914, .F. ) ;
#13551 = DIRECTION ( 'NONE',  ( -1.000000000000000000, 0.000000000000000000, 1.734723475976806848E-16 ) ) ;
#13552 = DIRECTION ( 'NONE',  ( -1.000000000000000000, 0.000000000000000000, 0.000000000000000000 ) ) ;
#13553 = CARTESIAN_POINT ( 'NONE',  ( -2.275425600868766995, 1.581315431065779542, -1.443027908266066639 ) ) ;
#13554 = VERTEX_POINT ( 'NONE', #49511 ) ;
#13555 = CARTESIAN_POINT ( 'NONE',  ( 1.833433833923351353, 0.000000000000000000, 1.574803149606291974 ) ) ;
#13556 = EDGE_CURVE ( 'NONE', #21355, #17854, #9607, .T. ) ;
#13557 = FACE_BOUND ( 'NONE', #43192, .T. ) ;
#13558 = EDGE_LOOP ( 'NONE', ( #391, #13522, #32776, #4201 ) ) ;
#13559 = CARTESIAN_POINT ( 'NONE',  ( 2.109061063546357584, 1.748596092898957233, 1.744865349675275956 ) ) ;
#13560 = ORIENTED_EDGE ( 'NONE', *, *, #24911, .T. ) ;
#13561 = ORIENTED_EDGE ( 'NONE', *, *, #47358, .F. ) ;
#13562 = LINE ( 'NONE', #21559, #11847 ) ;
#13563 = ORIENTED_EDGE ( 'NONE', *, *, #42014, .F. ) ;
#13564 = DIRECTION ( 'NONE',  ( -1.000000000000000000, 0.000000000000000000, 1.734723475976806848E-16 ) ) ;
#13565 = CARTESIAN_POINT ( 'NONE',  ( 0.7722537565518702296, 1.629158966512215923, -2.613214498325589386 ) ) ;
#13566 = VERTEX_POINT ( 'NONE', #41819 ) ;
#13567 =( GEOMETRIC_REPRESENTATION_CONTEXT ( 3 ) GLOBAL_UNCERTAINTY_ASSIGNED_CONTEXT ( ( #2460 ) ) GLOBAL_UNIT_ASSIGNED_CONTEXT ( ( #9874, #41876, #17617 ) ) REPRESENTATION_CONTEXT ( 'NONE', 'WORKASPACE' ) );
#13568 = VECTOR ( 'NONE', #6837, 39.37007874015748143 ) ;
#13569 = VECTOR ( 'NONE', #28052, 39.37007874015748143 ) ;
#13570 = EDGE_CURVE ( 'NONE', #28950, #5726, #18321, .T. ) ;
#13571 =( LENGTH_UNIT ( ) NAMED_UNIT ( * ) SI_UNIT ( $, .METRE. ) );
#13572 = DIRECTION ( 'NONE',  ( 0.000000000000000000, 0.000000000000000000, 1.000000000000000000 ) ) ;
#13573 = CARTESIAN_POINT ( 'NONE',  ( -0.2727639067037602172, 0.000000000000000000, 1.417322834645662777 ) ) ;
#13574 = VECTOR ( 'NONE', #50728, 39.37007874015748143 ) ;
#13575 = AXIS2_PLACEMENT_3D ( 'NONE', #32455, #44305, #13084 ) ;
#13576 = EDGE_CURVE ( 'NONE', #31520, #2997, #37968, .T. ) ;
#13577 = CARTESIAN_POINT ( 'NONE',  ( 2.623970503359832840, 1.658226141870901227, 0.8008345106751136866 ) ) ;
#13578 = ADVANCED_FACE ( 'NONE', ( #37192 ), #12861, .T. ) ;
#13579 = DIRECTION ( 'NONE',  ( 0.000000000000000000, 0.000000000000000000, -1.000000000000000000 ) ) ;
#13580 = CARTESIAN_POINT ( 'NONE',  ( -0.2134117707794043750, 0.02450148541315291459, -1.822192086320855164 ) ) ;
#13581 = AXIS2_PLACEMENT_3D ( 'NONE', #35100, #491, #7478 ) ;
#13582 = ORIENTED_EDGE ( 'NONE', *, *, #1953, .T. ) ;
#13583 = LINE ( 'NONE', #14083, #45571 ) ;
#13584 = EDGE_CURVE ( 'NONE', #20129, #9823, #9562, .T. ) ;
#13585 = EDGE_CURVE ( 'NONE', #14008, #7984, #45154, .T. ) ;
#13586 = DIRECTION ( 'NONE',  ( 0.000000000000000000, 0.000000000000000000, -1.000000000000000000 ) ) ;
#13587 = ORIENTED_EDGE ( 'NONE', *, *, #18395, .T. ) ;
#13588 = CARTESIAN_POINT ( 'NONE',  ( 1.363819533518803029, 0.000000000000000000, -1.417322834645665219 ) ) ;
#13589 = FACE_OUTER_BOUND ( 'NONE', #40339, .T. ) ;
#13590 = ORIENTED_EDGE ( 'NONE', *, *, #29590, .T. ) ;
#13591 = LINE ( 'NONE', #22100, #26319 ) ;
#13592 = LINE ( 'NONE', #29591, #10171 ) ;
#13593 = DIRECTION ( 'NONE',  ( -0.9998717552508122886, -0.01601477604151182316, 0.000000000000000000 ) ) ;
#13594 = VERTEX_POINT ( 'NONE', #41312 ) ;
#13595 = CARTESIAN_POINT ( 'NONE',  ( 2.074049943651431693, 5.118110236220475784, 0.6221544894624241318 ) ) ;
#13596 = ORIENTED_EDGE ( 'NONE', *, *, #47759, .T. ) ;
#13597 = FACE_BOUND ( 'NONE', #2627, .T. ) ;
#13598 = FACE_OUTER_BOUND ( 'NONE', #30066, .T. ) ;
#13599 = PLANE ( 'NONE',  #7846 ) ;
#13600 = LINE ( 'NONE', #29337, #40025 ) ;
#13601 = ORIENTED_EDGE ( 'NONE', *, *, #22064, .F. ) ;
#13602 = EDGE_LOOP ( 'NONE', ( #20185, #34681, #34601, #10275 ) ) ;
#13603 = VECTOR ( 'NONE', #43329, 39.37007874015748143 ) ;
#13604 = CARTESIAN_POINT ( 'NONE',  ( -0.2727639067037602172, 3.346456692913386100, 1.102362204724404160 ) ) ;
#13605 = ORIENTED_EDGE ( 'NONE', *, *, #23574, .T. ) ;
#13606 = VECTOR ( 'NONE', #44664, 39.37007874015748143 ) ;
#13607 = LINE ( 'NONE', #36081, #42566 ) ;
#13608 = EDGE_LOOP ( 'NONE', ( #31778, #23515, #11870, #17844 ) ) ;
#13609 = AXIS2_PLACEMENT_3D ( 'NONE', #27734, #4247, #19981 ) ;
#13610 = DIRECTION ( 'NONE',  ( 0.000000000000000000, -1.000000000000000000, 0.000000000000000000 ) ) ;
#13611 = ORIENTED_EDGE ( 'NONE', *, *, #29777, .T. ) ;
#13612 = CARTESIAN_POINT ( 'NONE',  ( 0.8182917201112824834, 3.346456692913386100, 2.047244094488179567 ) ) ;
#13613 = CARTESIAN_POINT ( 'NONE',  ( -0.6381684359064370149, 1.664872118777908527, -2.127367250395180598 ) ) ;
#13614 = EDGE_CURVE ( 'NONE', #9471, #16563, #21690, .T. ) ;
#13615 = CIRCLE ( 'NONE', #16894, 0.3740157480314960647 ) ;
#13616 = EDGE_LOOP ( 'NONE', ( #12881, #43457, #43141, #41683 ) ) ;
#13617 = EDGE_CURVE ( 'NONE', #36555, #16654, #37601, .T. ) ;
#13618 = CARTESIAN_POINT ( 'NONE',  ( 0.000000000000000000, 3.267716535433071279, 0.000000000000000000 ) ) ;
#13619 = ORIENTED_EDGE ( 'NONE', *, *, #4896, .F. ) ;
#13620 = EDGE_LOOP ( 'NONE', ( #18277, #38388, #40730, #5093 ) ) ;
#13621 = EDGE_CURVE ( 'NONE', #1816, #46637, #27066, .T. ) ;
#13622 = ORIENTED_EDGE ( 'NONE', *, *, #13134, .F. ) ;
#13623 = ORIENTED_EDGE ( 'NONE', *, *, #44828, .F. ) ;
#13624 = DIRECTION ( 'NONE',  ( 0.000000000000000000, 0.000000000000000000, -1.000000000000000000 ) ) ;
#13625 = ORIENTED_EDGE ( 'NONE', *, *, #33669, .F. ) ;
#13626 = CARTESIAN_POINT ( 'NONE',  ( 2.378961647330872786, 3.267716535433071279, -0.5118110236220471121 ) ) ;
#13627 = ORIENTED_EDGE ( 'NONE', *, *, #40719, .F. ) ;
#13628 = CARTESIAN_POINT ( 'NONE',  ( -2.076715649576790224, 1.576214352228098470, 0.6230206298219045369 ) ) ;
#13629 = EDGE_CURVE ( 'NONE', #27405, #47107, #24424, .T. ) ;
#13630 = LINE ( 'NONE', #6395, #42869 ) ;
#13631 = ORIENTED_EDGE ( 'NONE', *, *, #21032, .T. ) ;
#13632 = DIRECTION ( 'NONE',  ( 1.000000000000000000, 0.000000000000000000, -3.469446951953613696E-16 ) ) ;
#13633 = CARTESIAN_POINT ( 'NONE',  ( -0.6214413264104945434, 3.267716535433071279, -1.102362204724405492 ) ) ;
#13634 = VECTOR ( 'NONE', #16173, 39.37007874015748143 ) ;
#13635 = ORIENTED_EDGE ( 'NONE', *, *, #26379, .F. ) ;
#13636 = CARTESIAN_POINT ( 'NONE',  ( -1.936609506549060722, 1.676883605369557051, 0.9862484270667263297 ) ) ;
#13637 = CARTESIAN_POINT ( 'NONE',  ( -1.166969139818016199, 3.346456692913386100, 1.850393700787392293 ) ) ;
#13638 = EDGE_CURVE ( 'NONE', #20465, #10525, #2831, .T. ) ;
#13639 = VECTOR ( 'NONE', #28611, 39.37007874015748854 ) ;
#13640 = CARTESIAN_POINT ( 'NONE',  ( 1.363819533518803029, 3.267716535433071279, -1.929133858267710666 ) ) ;
#13641 = VECTOR ( 'NONE', #35174, 39.37007874015748143 ) ;
#13642 = DIRECTION ( 'NONE',  ( 0.000000000000000000, 0.000000000000000000, 1.000000000000000000 ) ) ;
#13643 = DIRECTION ( 'NONE',  ( 1.142080616180681165E-16, -1.000000000000000000, -2.072570748943160811E-17 ) ) ;
#13644 = DIRECTION ( 'NONE',  ( 0.000000000000000000, -1.000000000000000000, 0.000000000000000000 ) ) ;
#13645 = EDGE_LOOP ( 'NONE', ( #47319, #26225, #29942, #9730 ) ) ;
#13646 = FACE_OUTER_BOUND ( 'NONE', #19555, .T. ) ;
#13647 = DIRECTION ( 'NONE',  ( 0.000000000000000000, 0.000000000000000000, -1.000000000000000000 ) ) ;
#13648 = VECTOR ( 'NONE', #35747, 39.37007874015748143 ) ;
#13649 = ORIENTED_EDGE ( 'NONE', *, *, #4933, .T. ) ;
#13650 = DIRECTION ( 'NONE',  ( -1.156482317317871478E-16, 0.000000000000000000, -1.000000000000000000 ) ) ;
#13651 = ORIENTED_EDGE ( 'NONE', *, *, #1328, .T. ) ;
#13652 = EDGE_CURVE ( 'NONE', #33364, #27812, #7213, .T. ) ;
#13653 = CARTESIAN_POINT ( 'NONE',  ( 0.5455278134075217666, 3.346456692913386100, 1.889763779527550369 ) ) ;
#13654 = DIRECTION ( 'NONE',  ( -0.04486483035051863633, 1.288287287306305283E-16, 0.9989930665413144784 ) ) ;
#13655 = DIRECTION ( 'NONE',  ( -0.000000000000000000, 1.000000000000000000, -0.000000000000000000 ) ) ;
#13656 = CARTESIAN_POINT ( 'NONE',  ( -1.344179059205499849, 1.694369366911352204, 2.345726623500195451 ) ) ;
#13657 = CARTESIAN_POINT ( 'NONE',  ( 0.000000000000000000, 3.267716535433071279, 1.259842519685033357 ) ) ;
#13658 = ORIENTED_EDGE ( 'NONE', *, *, #2140, .T. ) ;
#13659 = DIRECTION ( 'NONE',  ( 0.000000000000000000, 0.000000000000000000, -1.000000000000000000 ) ) ;
#13660 = CARTESIAN_POINT ( 'NONE',  ( 0.8329809839909850799, 1.732245219823249638, -2.833254665166554442 ) ) ;
#13661 = DIRECTION ( 'NONE',  ( 0.000000000000000000, 1.000000000000000000, 0.000000000000000000 ) ) ;
#13662 = VERTEX_POINT ( 'NONE', #34827 ) ;
#13663 = DIRECTION ( 'NONE',  ( -0.000000000000000000, 1.000000000000000000, -0.000000000000000000 ) ) ;
#13664 = DIRECTION ( 'NONE',  ( 1.000000000000000000, 0.000000000000000000, 0.000000000000000000 ) ) ;
#13665 = ORIENTED_EDGE ( 'NONE', *, *, #50257, .F. ) ;
#13666 = CARTESIAN_POINT ( 'NONE',  ( 2.437180031585944207, 1.658768335924418080, -1.667735833703099191 ) ) ;
#13667 = CARTESIAN_POINT ( 'NONE',  ( 0.8182917201112819283, 0.000000000000000000, 0.2755905511810994302 ) ) ;
#13668 = CARTESIAN_POINT ( 'NONE',  ( 0.000000000000000000, 3.267716535433071279, 0.1181102362204704270 ) ) ;
#13669 = AXIS2_PLACEMENT_3D ( 'NONE', #2906, #34657, #11409 ) ;
#13670 = VERTEX_POINT ( 'NONE', #7709 ) ;
#13672 = ORIENTED_EDGE ( 'NONE', *, *, #46798, .T. ) ;
#13671 = ADVANCED_FACE ( 'NONE', ( #3081 ), #30957, .F. ) ;
#13673 = VECTOR ( 'NONE', #36617, 39.37007874015748143 ) ;
#13674 = LINE ( 'NONE', #9286, #18577 ) ;
#13675 = DIRECTION ( 'NONE',  ( 1.734723475976806848E-16, -0.000000000000000000, 1.000000000000000000 ) ) ;
#13676 = FACE_BOUND ( 'NONE', #17994, .T. ) ;
#13677 = VECTOR ( 'NONE', #40269, 39.37007874015748854 ) ;
#13678 = ADVANCED_FACE ( 'NONE', ( #31209 ), #22955, .F. ) ;
#13679 = CARTESIAN_POINT ( 'NONE',  ( 0.08139965876239094178, 1.610780518492231694, 0.000000000000000000 ) ) ;
#13680 = DIRECTION ( 'NONE',  ( -0.000000000000000000, 1.000000000000000000, -0.000000000000000000 ) ) ;
#13681 = EDGE_CURVE ( 'NONE', #36107, #24851, #7143, .T. ) ;
#13682 = AXIS2_PLACEMENT_3D ( 'NONE', #42610, #34874, #19360 ) ;
#13684 = EDGE_LOOP ( 'NONE', ( #36840, #39769, #12093, #7857 ) ) ;
#13683 = EDGE_CURVE ( 'NONE', #26431, #26163, #51017, .T. ) ;
#13685 = ORIENTED_EDGE ( 'NONE', *, *, #9724, .F. ) ;
#13686 = CARTESIAN_POINT ( 'NONE',  ( 0.08139965876239094178, 1.610780518492231694, 0.000000000000000000 ) ) ;
#13687 = CONICAL_SURFACE ( 'NONE', #42529, 1.850107469027523210, 0.6386652850508578450 ) ;
#13688 = CARTESIAN_POINT ( 'NONE',  ( -2.076656781855024114, 1.674640491952791077, 0.6230015025396302697 ) ) ;
#13689 = VERTEX_POINT ( 'NONE', #11081 ) ;
#13690 = ORIENTED_EDGE ( 'NONE', *, *, #49585, .T. ) ;
#13691 = ORIENTED_EDGE ( 'NONE', *, *, #2021, .F. ) ;
#13692 = CARTESIAN_POINT ( 'NONE',  ( 1.761123562704338452, 3.346456692913386100, 1.259842519685033135 ) ) ;
#13693 = DIRECTION ( 'NONE',  ( -0.000000000000000000, 0.000000000000000000, 1.000000000000000000 ) ) ;
#13694 = EDGE_CURVE ( 'NONE', #9041, #30555, #16993, .T. ) ;
#13695 = PLANE ( 'NONE',  #9392 ) ;
#13696 = CARTESIAN_POINT ( 'NONE',  ( 1.687984952120843207, 3.346456692913386100, -1.259842519685035800 ) ) ;
#13697 = VERTEX_POINT ( 'NONE', #15707 ) ;
#13698 = VERTEX_POINT ( 'NONE', #26568 ) ;
#13699 = DIRECTION ( 'NONE',  ( -0.000000000000000000, 1.000000000000000000, -0.000000000000000000 ) ) ;
#13700 = B_SPLINE_CURVE_WITH_KNOTS ( 'NONE', 3,
 ( #27448, #16608, #23837, #28209 ),
 .UNSPECIFIED., .F., .F.,
 ( 4, 4 ),
 ( 2.655965292660759762E-07, 0.002500437883007026758 ),
 .UNSPECIFIED. ) ;
#13701 = LINE ( 'NONE', #50030, #40660 ) ;
#13702 = EDGE_CURVE ( 'NONE', #7345, #36591, #42571, .T. ) ;
#13703 = FACE_OUTER_BOUND ( 'NONE', #49601, .T. ) ;
#13704 = CARTESIAN_POINT ( 'NONE',  ( 1.015142113812069091, 3.267716535433071279, -2.222792731763669760 ) ) ;
#13705 = CARTESIAN_POINT ( 'NONE',  ( -0.5455278134075208785, 3.346456692913386100, 0.9448818897637749625 ) ) ;
#13706 = EDGE_CURVE ( 'NONE', #28139, #22211, #41612, .T. ) ;
#13707 = VECTOR ( 'NONE', #25125, 39.37007874015748143 ) ;
#13708 = CARTESIAN_POINT ( 'NONE',  ( 0.04573806838996180568, 0.000000000000000000, 0.07195353765596652906 ) ) ;
#13709 = ORIENTED_EDGE ( 'NONE', *, *, #21364, .F. ) ;
#13710 = VECTOR ( 'NONE', #13205, 39.37007874015748143 ) ;
#13711 = LINE ( 'NONE', #9836, #1149 ) ;
#13712 = DIRECTION ( 'NONE',  ( 1.000000000000000000, -0.000000000000000000, 0.000000000000000000 ) ) ;
#13713 = AXIS2_PLACEMENT_3D ( 'NONE', #45595, #14387, #24987 ) ;
#13714 = ORIENTED_EDGE ( 'NONE', *, *, #19059, .T. ) ;
#13715 = EDGE_CURVE ( 'NONE', #31775, #39889, #22704, .T. ) ;
#13716 = AXIS2_PLACEMENT_3D ( 'NONE', #40077, #40344, #4713 ) ;
#13717 = VERTEX_POINT ( 'NONE', #38211 ) ;
#13718 = CARTESIAN_POINT ( 'NONE',  ( -1.461782879395278290, 0.000000000000000000, -1.598346982901829527 ) ) ;
#13719 = PLANE ( 'NONE',  #36925 ) ;
#13720 = AXIS2_PLACEMENT_3D ( 'NONE', #25358, #26121, #45967 ) ;
#13721 = ORIENTED_EDGE ( 'NONE', *, *, #25204, .F. ) ;
#13722 = VECTOR ( 'NONE', #17229, 39.37007874015748143 ) ;
#13723 = ADVANCED_FACE ( 'NONE', ( #39202 ), #15460, .F. ) ;
#13724 = ORIENTED_EDGE ( 'NONE', *, *, #25636, .T. ) ;
#13725 = CARTESIAN_POINT ( 'NONE',  ( -0.2727639067037602727, 3.346456692913386100, 1.535433070866133898 ) ) ;
#13726 = VERTEX_POINT ( 'NONE', #11582 ) ;
#13727 = FACE_OUTER_BOUND ( 'NONE', #33681, .T. ) ;
#13728 = CARTESIAN_POINT ( 'NONE',  ( 0.8182917201112824834, 3.346456692913386100, 1.535433070866133898 ) ) ;
#13729 = VERTEX_POINT ( 'NONE', #27315 ) ;
#13730 = ORIENTED_EDGE ( 'NONE', *, *, #2017, .F. ) ;
#13731 = LINE ( 'NONE', #50060, #8205 ) ;
#13732 = ORIENTED_EDGE ( 'NONE', *, *, #37352, .F. ) ;
#13733 = ORIENTED_EDGE ( 'NONE', *, *, #40138, .T. ) ;
#13734 = DIRECTION ( 'NONE',  ( -0.000000000000000000, 1.000000000000000000, -0.000000000000000000 ) ) ;
#13735 = DIRECTION ( 'NONE',  ( -1.267583980596137654E-16, 1.000000000000000000, -2.300325776299734791E-17 ) ) ;
#13736 = CARTESIAN_POINT ( 'NONE',  ( 0.2727639067037604947, 0.000000000000000000, -1.102362204724405714 ) ) ;
#13737 = EDGE_CURVE ( 'NONE', #975, #10759, #47158, .T. ) ;
#13738 = VERTEX_POINT ( 'NONE', #16740 ) ;
#13739 = DIRECTION ( 'NONE',  ( -0.000000000000000000, 1.000000000000000000, -0.000000000000000000 ) ) ;
#13740 = CARTESIAN_POINT ( 'NONE',  ( -0.6214413264104939882, 3.267716535433071279, 0.9055118110236167750 ) ) ;
#13741 = CARTESIAN_POINT ( 'NONE',  ( 2.629403693901861360E-16, 3.267716535433071279, -4.561288315631693258E-32 ) ) ;
#13742 = AXIS2_PLACEMENT_3D ( 'NONE', #15160, #18781, #19275 ) ;
#13743 = EDGE_CURVE ( 'NONE', #26074, #39122, #4345, .T. ) ;
#13744 = ORIENTED_EDGE ( 'NONE', *, *, #3269, .T. ) ;
#13745 = LINE ( 'NONE', #9615, #43013 ) ;
#13746 = CARTESIAN_POINT ( 'NONE',  ( 0.000000000000000000, 3.267716535433071279, -0.9448818897637765168 ) ) ;
#13747 = CONICAL_SURFACE ( 'NONE', #36044, 3.033577403570480779, 1.554780866114618743 ) ;
#13748 = AXIS2_PLACEMENT_3D ( 'NONE', #50897, #39847, #4480 ) ;
#13749 = LINE ( 'NONE', #5991, #28251 ) ;
#13750 = VERTEX_POINT ( 'NONE', #24483 ) ;
#13751 = VERTEX_POINT ( 'NONE', #28083 ) ;
#13752 = LINE ( 'NONE', #29495, #12640 ) ;
#13753 = CIRCLE ( 'NONE', #12084, 2.952755905511811552 ) ;
#13754 = CARTESIAN_POINT ( 'NONE',  ( -4.268512490100411402E-16, 3.267716535433071279, -2.086614173228339641 ) ) ;
#13755 = CARTESIAN_POINT ( 'NONE',  ( -2.473328087603087866, 1.680701298296960688, -1.612973869594296783 ) ) ;
#13756 = EDGE_LOOP ( 'NONE', ( #37189, #3211, #22136, #3054 ) ) ;
#13757 = ORIENTED_EDGE ( 'NONE', *, *, #32233, .T. ) ;
#13758 = AXIS2_PLACEMENT_3D ( 'NONE', #12516, #36532, #17414 ) ;
#13759 = CARTESIAN_POINT ( 'NONE',  ( -0.8942052331142552601, 0.000000000000000000, 1.692913385826762873 ) ) ;
#13760 = ORIENTED_EDGE ( 'NONE', *, *, #19942, .F. ) ;
#13761 = LINE ( 'NONE', #37008, #38980 ) ;
#13762 = LINE ( 'NONE', #13254, #12748 ) ;
#13763 = EDGE_CURVE ( 'NONE', #7991, #30461, #4100, .T. ) ;
#13764 = DIRECTION ( 'NONE',  ( 0.000000000000000000, -0.9063077870366510469, -0.4226182617406972208 ) ) ;
#13765 = PLANE ( 'NONE',  #34315 ) ;
#13766 = CARTESIAN_POINT ( 'NONE',  ( -1.528559409259449442, 1.546995005732493711, 2.526369546086722373 ) ) ;
#13767 = ORIENTED_EDGE ( 'NONE', *, *, #24462, .F. ) ;
#13768 = PLANE ( 'NONE',  #21719 ) ;
#13769 = CARTESIAN_POINT ( 'NONE',  ( -0.6584127755596833609, 0.000000000000000000, 1.614277297217976859 ) ) ;
#13770 = DIRECTION ( 'NONE',  ( 0.5877852522924802425, 9.388193118000637501E-17, -0.8090169943749422332 ) ) ;
#13771 = EDGE_CURVE ( 'NONE', #21877, #21738, #20603, .T. ) ;
#13772 = ORIENTED_EDGE ( 'NONE', *, *, #36886, .T. ) ;
#13773 = DIRECTION ( 'NONE',  ( 0.4338837391175526803, -1.045958227173635857E-16, 0.9009688679024218105 ) ) ;
#13774 = EDGE_CURVE ( 'NONE', #18870, #13250, #44085, .T. ) ;
#13775 = DIRECTION ( 'NONE',  ( -0.000000000000000000, 1.000000000000000000, -0.000000000000000000 ) ) ;
#13776 = LINE ( 'NONE', #9902, #13132 ) ;
#13778 = EDGE_CURVE ( 'NONE', #31200, #9169, #8224, .T. ) ;
#13777 = VERTEX_POINT ( 'NONE', #4602 ) ;
#13779 = AXIS2_PLACEMENT_3D ( 'NONE', #49352, #48584, #37277 ) ;
#13780 = DIRECTION ( 'NONE',  ( 1.734723475976806848E-16, -0.000000000000000000, 1.000000000000000000 ) ) ;
#13781 = DIRECTION ( 'NONE',  ( -1.598721155460225418E-14, 0.000000000000000000, 1.000000000000000000 ) ) ;
#13782 = VECTOR ( 'NONE', #2769, 39.37007874015748854 ) ;
#13783 = EDGE_CURVE ( 'NONE', #1039, #20045, #20346, .T. ) ;
#13784 = VERTEX_POINT ( 'NONE', #40233 ) ;
#13785 = CARTESIAN_POINT ( 'NONE',  ( 0.5455278134075211005, 0.000000000000000000, -1.456692913385822630 ) ) ;
#13786 = DIRECTION ( 'NONE',  ( 2.866708903754326305E-17, 1.000000000000000000, 1.255987235303924321E-16 ) ) ;
#13787 = VERTEX_POINT ( 'NONE', #8730 ) ;
#13788 = CARTESIAN_POINT ( 'NONE',  ( -0.9043257427339754795, 0.5245521110397223241, -1.991275222317478999 ) ) ;
#13789 = EDGE_CURVE ( 'NONE', #552, #22006, #32758, .T. ) ;
#13790 = DIRECTION ( 'NONE',  ( 1.000000000000000000, 0.000000000000000000, 0.000000000000000000 ) ) ;
#13791 = CARTESIAN_POINT ( 'NONE',  ( 0.4696143004045476022, 3.267716535433071279, -2.113816876263008293 ) ) ;
#13792 = LINE ( 'NONE', #13537, #6206 ) ;
#13793 = LINE ( 'NONE', #5787, #17218 ) ;
#13794 = EDGE_LOOP ( 'NONE', ( #6380, #30007, #6182, #43761 ) ) ;
#13795 = ORIENTED_EDGE ( 'NONE', *, *, #39296, .F. ) ;
#13796 = CARTESIAN_POINT ( 'NONE',  ( -0.07591351300297340121, 3.267716535433071279, -1.929133858267710000 ) ) ;
#13797 = DIRECTION ( 'NONE',  ( 1.000000000000000000, 0.000000000000000000, -3.469446951953613696E-16 ) ) ;
#13798 = ORIENTED_EDGE ( 'NONE', *, *, #6762, .T. ) ;
#13799 = CARTESIAN_POINT ( 'NONE',  ( 1.833433833923351353, 0.000000000000000000, -1.259842519685035800 ) ) ;
#13800 = DIRECTION ( 'NONE',  ( -3.469446951953613696E-16, 0.000000000000000000, -1.000000000000000000 ) ) ;
#13801 = PLANE ( 'NONE',  #17884 ) ;
#13802 = VECTOR ( 'NONE', #12103, 39.37007874015748143 ) ;
#13803 = EDGE_CURVE ( 'NONE', #11723, #38637, #47928, .T. ) ;
#13804 = ORIENTED_EDGE ( 'NONE', *, *, #14671, .F. ) ;
#13805 = VERTEX_POINT ( 'NONE', #16483 ) ;
#13806 = CARTESIAN_POINT ( 'NONE',  ( 0.8182917201112818173, 3.267716535433071279, -1.419509857074483292E-16 ) ) ;
#13807 = CARTESIAN_POINT ( 'NONE',  ( -1.439733046521776361, 3.267716535433071279, 0.1181102362204704270 ) ) ;
#13808 = DIRECTION ( 'NONE',  ( 0.000000000000000000, 0.000000000000000000, -1.000000000000000000 ) ) ;
#13809 = ADVANCED_FACE ( 'NONE', ( #39459 ), #40091, .T. ) ;
#13810 = VERTEX_POINT ( 'NONE', #48186 ) ;
#13811 = LINE ( 'NONE', #2188, #38873 ) ;
#13812 = CARTESIAN_POINT ( 'NONE',  ( -1.461363083917493810, 6.692913385826772199, 1.597866488315562439 ) ) ;
#13813 = EDGE_LOOP ( 'NONE', ( #6310, #19737, #49868, #12844 ) ) ;
#13814 = CARTESIAN_POINT ( 'NONE',  ( 0.000000000000000000, 3.346456692913386100, 0.000000000000000000 ) ) ;
#13815 = VERTEX_POINT ( 'NONE', #19823 ) ;
#13816 = ORIENTED_EDGE ( 'NONE', *, *, #43972, .T. ) ;
#13817 = CARTESIAN_POINT ( 'NONE',  ( 0.9948011493083116497, 0.5223602044264220590, 0.9948011493083110945 ) ) ;
#13818 = DIRECTION ( 'NONE',  ( -3.469446951953613696E-16, 0.000000000000000000, -1.000000000000000000 ) ) ;
#13819 = AXIS2_PLACEMENT_3D ( 'NONE', #47532, #11949, #24339 ) ;
#13820 = VECTOR ( 'NONE', #18911, 39.37007874015748143 ) ;
#13821 = ORIENTED_EDGE ( 'NONE', *, *, #45532, .T. ) ;
#13822 = CARTESIAN_POINT ( 'NONE',  ( 2.823445274216730638, 1.763256531483745837, 0.8656477926280683466 ) ) ;
#13823 = DIRECTION ( 'NONE',  ( -0.000000000000000000, 1.000000000000000000, -0.000000000000000000 ) ) ;
#13824 = ORIENTED_EDGE ( 'NONE', *, *, #4699, .F. ) ;
#13825 = AXIS2_PLACEMENT_3D ( 'NONE', #10964, #11221, #42704 ) ;
#13826 = DIRECTION ( 'NONE',  ( -1.000000000000000000, 0.000000000000000000, 0.000000000000000000 ) ) ;
#13827 = FACE_OUTER_BOUND ( 'NONE', #49062, .T. ) ;
#13828 = CARTESIAN_POINT ( 'NONE',  ( 1.081562861160096700, 0.04524287409729283588, -1.572369041216798768 ) ) ;
#13829 = DIRECTION ( 'NONE',  ( -0.000000000000000000, 1.000000000000000000, -0.000000000000000000 ) ) ;
#13830 = DIRECTION ( 'NONE',  ( 0.000000000000000000, 0.000000000000000000, -1.000000000000000000 ) ) ;
#13831 = VERTEX_POINT ( 'NONE', #24739 ) ;
#13832 = PLANE ( 'NONE',  #42308 ) ;
#13833 = VECTOR ( 'NONE', #14081, 39.37007874015748143 ) ;
#13834 = LINE ( 'NONE', #45549, #13309 ) ;
#13835 = ORIENTED_EDGE ( 'NONE', *, *, #36522, .T. ) ;
#13836 = LINE ( 'NONE', #48898, #37238 ) ;
#13837 = EDGE_CURVE ( 'NONE', #43925, #12716, #47419, .T. ) ;
#13838 = CARTESIAN_POINT ( 'NONE',  ( -0.3136974817027967100, 1.615928078135840051, -2.936457595020224520 ) ) ;
#13839 = ORIENTED_EDGE ( 'NONE', *, *, #1239, .T. ) ;
#13840 = FACE_OUTER_BOUND ( 'NONE', #3760, .T. ) ;
#13841 = EDGE_CURVE ( 'NONE', #35717, #7477, #12601, .T. ) ;
#13842 = LINE ( 'NONE', #33979, #16774 ) ;
#13843 = EDGE_CURVE ( 'NONE', #43306, #1528, #45813, .T. ) ;
#13844 = DIRECTION ( 'NONE',  ( 1.734723475976806848E-16, -0.000000000000000000, 1.000000000000000000 ) ) ;
#13845 = ORIENTED_EDGE ( 'NONE', *, *, #15134, .F. ) ;
#13846 = CARTESIAN_POINT ( 'NONE',  ( 0.5455278134075217666, 3.346456692913386100, 2.095509194042718626 ) ) ;
#13847 = ORIENTED_EDGE ( 'NONE', *, *, #49403, .F. ) ;
#13848 = B_SPLINE_CURVE_WITH_KNOTS ( 'NONE', 3,
 ( #38597, #27209, #34718, #7601 ),
 .UNSPECIFIED., .F., .F.,
 ( 4, 4 ),
 ( 4.389659793852969620E-07, 0.04940888453222644361 ),
 .UNSPECIFIED. ) ;
#13849 = FACE_BOUND ( 'NONE', #2494, .T. ) ;
#13850 = LINE ( 'NONE', #2232, #22627 ) ;
#13851 = FACE_OUTER_BOUND ( 'NONE', #976, .T. ) ;
#13852 = PLANE ( 'NONE',  #8702 ) ;
#13853 = AXIS2_PLACEMENT_3D ( 'NONE', #48847, #13532, #5780 ) ;
#13854 = VECTOR ( 'NONE', #13655, 39.37007874015748143 ) ;
#13855 = VERTEX_POINT ( 'NONE', #28340 ) ;
#13856 = ORIENTED_EDGE ( 'NONE', *, *, #20608, .F. ) ;
#13857 = LINE ( 'NONE', #6104, #17206 ) ;
#13858 = ORIENTED_EDGE ( 'NONE', *, *, #14474, .T. ) ;
#13859 = VECTOR ( 'NONE', #29422, 39.37007874015748143 ) ;
#13860 = EDGE_CURVE ( 'NONE', #11675, #42907, #40911, .T. ) ;
#13861 = DIRECTION ( 'NONE',  ( -0.000000000000000000, 0.000000000000000000, 1.000000000000000000 ) ) ;
#13862 = ORIENTED_EDGE ( 'NONE', *, *, #5472, .F. ) ;
#13863 = LINE ( 'NONE', #18747, #23985 ) ;
#13864 = EDGE_CURVE ( 'NONE', #46567, #2988, #44589, .T. ) ;
#13865 = ORIENTED_EDGE ( 'NONE', *, *, #2777, .F. ) ;
#13866 = DIRECTION ( 'NONE',  ( 1.734723475976806848E-16, 0.000000000000000000, 1.000000000000000000 ) ) ;
#13867 = ADVANCED_FACE ( 'NONE', ( #43574 ), #15960, .F. ) ;
#13868 = CONICAL_SURFACE ( 'NONE', #42703, 2.246510896728926010, 0.01601546068027819014 ) ;
#13869 = DIRECTION ( 'NONE',  ( 0.000000000000000000, 0.000000000000000000, 1.000000000000000000 ) ) ;
#13870 = ORIENTED_EDGE ( 'NONE', *, *, #41516, .F. ) ;
#13871 = EDGE_CURVE ( 'NONE', #17434, #25112, #7038, .T. ) ;
#13872 = LINE ( 'NONE', #25738, #33193 ) ;
#13873 = ORIENTED_EDGE ( 'NONE', *, *, #16214, .F. ) ;
#13874 = EDGE_LOOP ( 'NONE', ( #47859, #22654, #11735, #4552 ) ) ;
#13875 = VECTOR ( 'NONE', #37912, 39.37007874015748143 ) ;
#13876 = ORIENTED_EDGE ( 'NONE', *, *, #41261, .F. ) ;
#13877 = VERTEX_POINT ( 'NONE', #16225 ) ;
#13878 = CARTESIAN_POINT ( 'NONE',  ( -0.2493966119946618154, 1.605482210820551758, -2.222016418551142181 ) ) ;
#13879 = ORIENTED_EDGE ( 'NONE', *, *, #43770, .T. ) ;
#13880 = DIRECTION ( 'NONE',  ( 1.734723475976806848E-16, -0.000000000000000000, 1.000000000000000000 ) ) ;
#13881 = PLANE ( 'NONE',  #31020 ) ;
#13882 = VECTOR ( 'NONE', #2549, 39.37007874015748143 ) ;
#13883 = DIRECTION ( 'NONE',  ( 0.000000000000000000, 0.000000000000000000, 1.000000000000000000 ) ) ;
#13884 = VERTEX_POINT ( 'NONE', #9240 ) ;
#13886 = CARTESIAN_POINT ( 'NONE',  ( 0.07982360342473591996, 1.709180471932028711, 0.000000000000000000 ) ) ;
#13885 = B_SPLINE_CURVE_WITH_KNOTS ( 'NONE', 3,
 ( #39877, #43729, #3051, #32397 ),
 .UNSPECIFIED., .F., .F.,
 ( 4, 4 ),
 ( 0.01116762523142644965, 0.03073605728027439810 ),
 .UNSPECIFIED. ) ;
#13887 = CARTESIAN_POINT ( 'NONE',  ( 1.833433833923351353, 0.000000000000000000, -0.6299212598425181220 ) ) ;
#13888 = ORIENTED_EDGE ( 'NONE', *, *, #14202, .T. ) ;
#13889 = CARTESIAN_POINT ( 'NONE',  ( 0.5756566573088583993, 1.629780628454260194, 2.896516654582643291 ) ) ;
#13890 = CARTESIAN_POINT ( 'NONE',  ( 0.000000000000000000, 3.346456692913386100, 0.000000000000000000 ) ) ;
#13891 = CARTESIAN_POINT ( 'NONE',  ( 0.000000000000000000, 3.346456692913386100, 0.000000000000000000 ) ) ;
#13892 = CARTESIAN_POINT ( 'NONE',  ( -1.091055626815042645, 3.346456692913386100, -0.6299212598425177889 ) ) ;
#13893 = VECTOR ( 'NONE', #35427, 39.37007874015748143 ) ;
#13894 = CARTESIAN_POINT ( 'NONE',  ( 1.363819533518803251, 0.000000000000000000, 0.7874015748031454320 ) ) ;
#13895 = LINE ( 'NONE', #21899, #34348 ) ;
#13896 = ORIENTED_EDGE ( 'NONE', *, *, #29505, .F. ) ;
#13897 = DIRECTION ( 'NONE',  ( -0.01601477604151182663, 0.9998717552508123996, -0.000000000000000000 ) ) ;
#13898 = CARTESIAN_POINT ( 'NONE',  ( 0.000000000000000000, 2.755905511811024056, 0.000000000000000000 ) ) ;
#13899 = VECTOR ( 'NONE', #17494, 39.37007874015748143 ) ;
#13900 = EDGE_CURVE ( 'NONE', #39624, #21917, #17251, .T. ) ;
#13901 = B_SPLINE_CURVE_WITH_KNOTS ( 'NONE', 3,
 ( #3879, #50301, #47199, #11869 ),
 .UNSPECIFIED., .F., .F.,
 ( 4, 4 ),
 ( 3.459388077773027594E-07, 0.04345450118629323039 ),
 .UNSPECIFIED. ) ;
#13902 = ORIENTED_EDGE ( 'NONE', *, *, #4403, .T. ) ;
#13903 = DIRECTION ( 'NONE',  ( -0.9998717552508122886, -0.01601477604151185785, 0.000000000000000000 ) ) ;
#13904 = EDGE_CURVE ( 'NONE', #18049, #9822, #25506, .T. ) ;
#13905 = AXIS2_PLACEMENT_3D ( 'NONE', #19783, #23155, #3544 ) ;
#13906 = ORIENTED_EDGE ( 'NONE', *, *, #17789, .F. ) ;
#13907 = DIRECTION ( 'NONE',  ( 1.734723475976806848E-16, -0.000000000000000000, 1.000000000000000000 ) ) ;
#13908 = EDGE_CURVE ( 'NONE', #5433, #38240, #9512, .T. ) ;
#13909 = DIRECTION ( 'NONE',  ( 0.7071067811865469066, 0.7071067811865481278, -4.088782444488994004E-17 ) ) ;
#13910 = CARTESIAN_POINT ( 'NONE',  ( 0.4696143004045479352, 3.346456692913386100, -0.1574803149606298636 ) ) ;
#13911 = VECTOR ( 'NONE', #41008, 39.37007874015748143 ) ;
#13912 = CARTESIAN_POINT ( 'NONE',  ( 0.1968503937007877735, 3.346456692913386100, 0.7480314960629874665 ) ) ;
#13913 = DIRECTION ( 'NONE',  ( -1.000000000000000000, 0.000000000000000000, -0.000000000000000000 ) ) ;
#13914 = VERTEX_POINT ( 'NONE', #44845 ) ;
#13915 = DIRECTION ( 'NONE',  ( 1.000000000000000000, 0.000000000000000000, 0.000000000000000000 ) ) ;
#13916 = ORIENTED_EDGE ( 'NONE', *, *, #37580, .F. ) ;
#13917 = ORIENTED_EDGE ( 'NONE', *, *, #5565, .F. ) ;
#13918 = DIRECTION ( 'NONE',  ( -1.000000000000000000, 0.000000000000000000, 1.734723475976806848E-16 ) ) ;
#13919 = ORIENTED_EDGE ( 'NONE', *, *, #5408, .T. ) ;
#13920 = DIRECTION ( 'NONE',  ( 1.000000000000000000, 0.000000000000000000, 0.000000000000000000 ) ) ;
#13921 = CARTESIAN_POINT ( 'NONE',  ( -1.377952755905510918, 0.000000000000000000, -4.133858267716536083 ) ) ;
#13922 = VERTEX_POINT ( 'NONE', #5624 ) ;
#13923 = DIRECTION ( 'NONE',  ( -0.000000000000000000, 0.000000000000000000, 1.000000000000000000 ) ) ;
#13924 = ADVANCED_FACE ( 'NONE', ( #1743 ), #2004, .F. ) ;
#13925 =( BOUNDED_CURVE ( )  B_SPLINE_CURVE ( 3, ( #44328, #1731, #48171, #21612 ),
 .UNSPECIFIED., .F., .F. ) 
 B_SPLINE_CURVE_WITH_KNOTS ( ( 4, 4 ),
 ( 5.423165295728897384, 5.474004202337919622 ),
 .UNSPECIFIED. ) 
 CURVE ( )  GEOMETRIC_REPRESENTATION_ITEM ( )  RATIONAL_B_SPLINE_CURVE ( ( 1.000000000000000000, 0.9997846287284284372, 0.9997846287284284372, 1.000000000000000000 ) ) 
 REPRESENTATION_ITEM ( '' )  );
#13926 = VECTOR ( 'NONE', #39626, 39.37007874015748143 ) ;
#13927 = LINE ( 'NONE', #34314, #18315 ) ;
#13928 = CARTESIAN_POINT ( 'NONE',  ( 1.022166022771838767, 1.735184344206899487, 2.770237021086607410 ) ) ;
#13929 = ORIENTED_EDGE ( 'NONE', *, *, #45938, .F. ) ;
#13930 = ORIENTED_EDGE ( 'NONE', *, *, #1374, .F. ) ;
#13931 = ADVANCED_FACE ( 'NONE', ( #41754 ), #17750, .F. ) ;
#13932 = LINE ( 'NONE', #45899, #31472 ) ;
#13933 = FACE_BOUND ( 'NONE', #34671, .T. ) ;
#13934 = ORIENTED_EDGE ( 'NONE', *, *, #37123, .T. ) ;
#13935 = VECTOR ( 'NONE', #44455, 39.37007874015748143 ) ;
#13936 = VECTOR ( 'NONE', #6679, 39.37007874015748143 ) ;
#13937 = CARTESIAN_POINT ( 'NONE',  ( -2.105608695257993102, 1.045687859213095594, -1.448867510875124776 ) ) ;
#13938 = DIRECTION ( 'NONE',  ( 1.734723475976806848E-16, 0.000000000000000000, 1.000000000000000000 ) ) ;
#13939 = ORIENTED_EDGE ( 'NONE', *, *, #4963, .F. ) ;
#13940 = ORIENTED_EDGE ( 'NONE', *, *, #50630, .F. ) ;
#13941 = LINE ( 'NONE', #18314, #4333 ) ;
#13942 = CARTESIAN_POINT ( 'NONE',  ( -2.076696040374840901, 1.609023065478501602, 0.6230142584059638056 ) ) ;
#13943 = EDGE_LOOP ( 'NONE', ( #31006, #49260, #44187, #27625 ) ) ;
#13944 = ORIENTED_EDGE ( 'NONE', *, *, #47759, .F. ) ;
#13945 = VECTOR ( 'NONE', #40, 39.37007874015748143 ) ;
#13946 = EDGE_LOOP ( 'NONE', ( #10775, #21237, #27542, #39302 ) ) ;
#13947 = DIRECTION ( 'NONE',  ( -0.000000000000000000, 0.000000000000000000, 1.000000000000000000 ) ) ;
#13948 = CARTESIAN_POINT ( 'NONE',  ( -1.166969139818015533, 3.346456692913386100, 1.102362204724404160 ) ) ;
#13949 = CARTESIAN_POINT ( 'NONE',  ( -2.412085630707005990, 1.673474101395583835, 0.2770771474091495157 ) ) ;
#13950 = CARTESIAN_POINT ( 'NONE',  ( 0.08119777152254364916, 1.623385212329073957, 0.000000000000000000 ) ) ;
#13951 = ORIENTED_EDGE ( 'NONE', *, *, #18385, .F. ) ;
#13952 = ORIENTED_EDGE ( 'NONE', *, *, #11187, .F. ) ;
#13953 = LINE ( 'NONE', #18330, #10954 ) ;
#13954 = DIRECTION ( 'NONE',  ( -0.000000000000000000, 0.000000000000000000, 1.000000000000000000 ) ) ;
#13955 = LINE ( 'NONE', #33840, #43949 ) ;
#13956 = DIRECTION ( 'NONE',  ( -0.8584487936018727616, 0.000000000000000000, 0.5128992774058948045 ) ) ;
#13957 = CARTESIAN_POINT ( 'NONE',  ( 1.215807329263347114, 1.628950133432788494, 1.938968878379255578 ) ) ;
#13958 = PLANE ( 'NONE',  #9476 ) ;
#13959 = CIRCLE ( 'NONE', #759, 2.244934639244525076 ) ;
#13960 = DIRECTION ( 'NONE',  ( -3.469446951953613696E-16, 0.000000000000000000, -1.000000000000000000 ) ) ;
#13961 = EDGE_CURVE ( 'NONE', #28095, #37439, #37385, .T. ) ;
#13962 = ORIENTED_EDGE ( 'NONE', *, *, #17880, .F. ) ;
#13963 = FACE_OUTER_BOUND ( 'NONE', #50085, .T. ) ;
#13964 = CARTESIAN_POINT ( 'NONE',  ( -1.091055626815042645, 3.346456692913386100, 1.801691980386209258 ) ) ;
#13965 = EDGE_CURVE ( 'NONE', #33353, #2321, #26877, .T. ) ;
#13966 = VERTEX_POINT ( 'NONE', #17497 ) ;
#13967 = EDGE_CURVE ( 'NONE', #21978, #29226, #33257, .T. ) ;
#13968 = ORIENTED_EDGE ( 'NONE', *, *, #35313, .T. ) ;
#13969 = AXIS2_PLACEMENT_3D ( 'NONE', #46541, #15830, #47290 ) ;
#13970 = CARTESIAN_POINT ( 'NONE',  ( -1.363819533518803473, 3.267716535433071279, 2.027638360164056852 ) ) ;
#13971 = VERTEX_POINT ( 'NONE', #37639 ) ;
#13972 = EDGE_CURVE ( 'NONE', #2567, #47393, #49205, .T. ) ;
#13973 = VECTOR ( 'NONE', #38609, 39.37007874015748143 ) ;
#13974 = EDGE_LOOP ( 'NONE', ( #27458, #13021, #49481, #5738 ) ) ;
#13975 = DIRECTION ( 'NONE',  ( -3.986037398843765983E-20, -1.000000000000000000, -1.160734090543304660E-16 ) ) ;
#13976 = VECTOR ( 'NONE', #27656, 39.37007874015748143 ) ;
#13977 = ORIENTED_EDGE ( 'NONE', *, *, #12225, .F. ) ;
#13978 = DIRECTION ( 'NONE',  ( 0.000000000000000000, 0.000000000000000000, -1.000000000000000000 ) ) ;
#13979 = LINE ( 'NONE', #26601, #18950 ) ;
#13980 = ADVANCED_FACE ( 'NONE', ( #13371 ), #13881, .T. ) ;
#13981 = EDGE_LOOP ( 'NONE', ( #12183, #8122, #22378, #26957, #26295, #10585, #18726, #19043, #14023, #49965 ) ) ;
#13982 = VERTEX_POINT ( 'NONE', #29371 ) ;
#13983 = DIRECTION ( 'NONE',  ( -0.9009688679024218105, 1.288287287306305530E-16, 0.4338837391175526803 ) ) ;
#13984 = VERTEX_POINT ( 'NONE', #30132 ) ;
#13985 = ORIENTED_EDGE ( 'NONE', *, *, #14575, .F. ) ;
#13986 = EDGE_CURVE ( 'NONE', #24851, #1464, #25240, .T. ) ;
#13987 = DIRECTION ( 'NONE',  ( 1.734723475976806848E-16, -0.000000000000000000, 1.000000000000000000 ) ) ;
#13988 = DIRECTION ( 'NONE',  ( -0.000000000000000000, -1.000000000000000000, -0.000000000000000000 ) ) ;
#13989 = DIRECTION ( 'NONE',  ( -1.118904554427321068E-16, -1.000000000000000000, -3.087980359898530052E-17 ) ) ;
#13990 = ORIENTED_EDGE ( 'NONE', *, *, #34521, .T. ) ;
#13991 = LINE ( 'NONE', #49815, #34532 ) ;
#13992 = CARTESIAN_POINT ( 'NONE',  ( 1.327305353890115169, 0.5249316475426857309, -1.337120392888858422 ) ) ;
#13993 = AXIS2_PLACEMENT_3D ( 'NONE', #10365, #22489, #29979 ) ;
#13994 = ADVANCED_FACE ( 'NONE', ( #45096 ), #25492, .F. ) ;
#13995 = CARTESIAN_POINT ( 'NONE',  ( 0.000000000000000000, 3.267716535433071279, -1.929133858267710000 ) ) ;
#13996 = ORIENTED_EDGE ( 'NONE', *, *, #16264, .F. ) ;
#13997 = DIRECTION ( 'NONE',  ( 8.902872254220023478E-17, 1.000000000000000000, -9.311674343991161395E-17 ) ) ;
#13998 = DIRECTION ( 'NONE',  ( 1.000000000000000000, -0.000000000000000000, 0.000000000000000000 ) ) ;
#13999 = DIRECTION ( 'NONE',  ( 0.9009688679024218105, 0.000000000000000000, -0.4338837391175526803 ) ) ;
#14000 = VERTEX_POINT ( 'NONE', #9499 ) ;
#14001 = VERTEX_POINT ( 'NONE', #2259 ) ;
#14002 =( LENGTH_UNIT ( ) NAMED_UNIT ( * ) SI_UNIT ( $, .METRE. ) );
#14003 = EDGE_CURVE ( 'NONE', #32172, #25793, #5874, .T. ) ;
#14004 = VECTOR ( 'NONE', #8280, 39.37007874015748143 ) ;
#14005 = DIRECTION ( 'NONE',  ( -3.469446951953613696E-16, 0.000000000000000000, -1.000000000000000000 ) ) ;
#14006 = PLANE ( 'NONE',  #39316 ) ;
#14007 = DIRECTION ( 'NONE',  ( 1.000000000000000000, 0.000000000000000000, 0.000000000000000000 ) ) ;
#14008 = VERTEX_POINT ( 'NONE', #21623 ) ;
#14009 = VERTEX_POINT ( 'NONE', #25748 ) ;
#14010 = CARTESIAN_POINT ( 'NONE',  ( 2.043634885149959057, 6.692913385826772199, 0.7157624142946238388 ) ) ;
#14011 = VECTOR ( 'NONE', #2359, 39.37007874015748143 ) ;
#14012 = EDGE_LOOP ( 'NONE', ( #38278, #47827, #22291, #16937 ) ) ;
#14013 = CARTESIAN_POINT ( 'NONE',  ( 0.1067246931122726866, 0.02962905676920215767, 0.000000000000000000 ) ) ;
#14014 = CARTESIAN_POINT ( 'NONE',  ( 2.491402175429654253, 0.000000000000000000, -1.585592796919505831 ) ) ;
#14015 = DIRECTION ( 'NONE',  ( -1.000000000000000000, 0.000000000000000000, 1.734723475976806848E-16 ) ) ;
#14016 = CARTESIAN_POINT ( 'NONE',  ( -0.6157060063382256976, 0.5249316475426859530, 1.780600056526914443 ) ) ;
#14017 = CARTESIAN_POINT ( 'NONE',  ( 0.000000000000000000, 3.346456692913386100, 0.000000000000000000 ) ) ;
#14018 = VERTEX_POINT ( 'NONE', #49450 ) ;
#14019 = CARTESIAN_POINT ( 'NONE',  ( -1.909347346926324906, 0.000000000000000000, -0.4724409448818884805 ) ) ;
#14020 = CARTESIAN_POINT ( 'NONE',  ( -1.556712866041156440, 0.000000000000000000, 2.509548638715847435 ) ) ;
#14021 = DIRECTION ( 'NONE',  ( 1.000000000000000000, 0.000000000000000000, -3.469446951953613696E-16 ) ) ;
#14022 = EDGE_CURVE ( 'NONE', #16438, #810, #23671, .T. ) ;
#14023 = ORIENTED_EDGE ( 'NONE', *, *, #47947, .F. ) ;
#14024 = FACE_OUTER_BOUND ( 'NONE', #37359, .T. ) ;
#14025 = DIRECTION ( 'NONE',  ( 1.734723475976806848E-16, 0.000000000000000000, 1.000000000000000000 ) ) ;
#14026 = DIRECTION ( 'NONE',  ( -0.9998717552508122886, -0.01601477604151181275, 0.000000000000000000 ) ) ;
#14027 = EDGE_CURVE ( 'NONE', #27409, #26538, #14130, .T. ) ;
#14028 = ORIENTED_EDGE ( 'NONE', *, *, #38933, .F. ) ;
#14029 = EDGE_CURVE ( 'NONE', #18853, #9214, #46854, .T. ) ;
#14030 = CARTESIAN_POINT ( 'NONE',  ( 1.723188456408574210, 6.692913385826772199, 1.311251662046226452 ) ) ;
#14031 = ORIENTED_EDGE ( 'NONE', *, *, #16939, .T. ) ;
#14032 = DIRECTION ( 'NONE',  ( -3.469446951953613696E-16, 0.000000000000000000, -1.000000000000000000 ) ) ;
#14033 = CARTESIAN_POINT ( 'NONE',  ( 0.9360721529196784907, 0.000000000000000000, 1.470771056236116481 ) ) ;
#14034 = VERTEX_POINT ( 'NONE', #11525 ) ;
#14035 = DIRECTION ( 'NONE',  ( -0.9998717552508121775, -0.01601477604151182663, 0.000000000000000000 ) ) ;
#14036 = VECTOR ( 'NONE', #9756, 39.37007874015748143 ) ;
#14037 = LINE ( 'NONE', #13535, #24318 ) ;
#14038 = DIRECTION ( 'NONE',  ( 0.000000000000000000, 0.000000000000000000, -1.000000000000000000 ) ) ;
#14039 = CARTESIAN_POINT ( 'NONE',  ( 1.560669927219590747, 0.000000000000000000, -0.7874015748031473194 ) ) ;
#14040 = VECTOR ( 'NONE', #7584, 39.37007874015748143 ) ;
#14041 = DIRECTION ( 'NONE',  ( -0.000000000000000000, 1.000000000000000000, -0.000000000000000000 ) ) ;
#14042 = ORIENTED_EDGE ( 'NONE', *, *, #19491, .F. ) ;
#14043 = ORIENTED_EDGE ( 'NONE', *, *, #21032, .F. ) ;
#14044 = FACE_OUTER_BOUND ( 'NONE', #10733, .T. ) ;
#14045 = CARTESIAN_POINT ( 'NONE',  ( 0.08139965876239094178, 1.610780518492231694, 0.000000000000000000 ) ) ;
#14046 = ORIENTED_EDGE ( 'NONE', *, *, #40098, .T. ) ;
#14047 = LINE ( 'NONE', #49373, #37463 ) ;
#14048 = DIRECTION ( 'NONE',  ( 1.000000000000000000, 0.000000000000000000, 0.000000000000000000 ) ) ;
#14049 = AXIS2_PLACEMENT_3D ( 'NONE', #24775, #29149, #9796 ) ;
#14050 = LINE ( 'NONE', #30051, #22015 ) ;
#14051 = ORIENTED_EDGE ( 'NONE', *, *, #42467, .F. ) ;
#14052 = VERTEX_POINT ( 'NONE', #46105 ) ;
#14053 = CARTESIAN_POINT ( 'NONE',  ( 1.426808618753927282, 0.05077261674489902399, -1.296082183384024811 ) ) ;
#14054 = LINE ( 'NONE', #14305, #11775 ) ;
#14055 = EDGE_CURVE ( 'NONE', #30221, #30309, #3781, .T. ) ;
#14056 = CARTESIAN_POINT ( 'NONE',  ( -1.025452293874513199, 0.4610579152940182390, -1.025452293874513865 ) ) ;
#14057 = ORIENTED_EDGE ( 'NONE', *, *, #25936, .F. ) ;
#14058 = CARTESIAN_POINT ( 'NONE',  ( -1.675546303352015709, 1.681065010344670041, 1.399148864732502995 ) ) ;
#14059 = LINE ( 'NONE', #38327, #16146 ) ;
#14060 = VERTEX_POINT ( 'NONE', #38646 ) ;
#14061 = CARTESIAN_POINT ( 'NONE',  ( -0.8182917201112819283, 3.346456692913386100, -2.047244094488181343 ) ) ;
#14062 = ORIENTED_EDGE ( 'NONE', *, *, #27668, .T. ) ;
#14063 = VERTEX_POINT ( 'NONE', #10763 ) ;
#14064 = CARTESIAN_POINT ( 'NONE',  ( 2.015507221693567885, 1.674567190253306803, 1.140476272524640455 ) ) ;
#14065 = CARTESIAN_POINT ( 'NONE',  ( -0.8182917201112814842, 0.000000000000000000, 0.9055118110236167750 ) ) ;
#14066 = EDGE_CURVE ( 'NONE', #45414, #31828, #27002, .T. ) ;
#14067 = CARTESIAN_POINT ( 'NONE',  ( -1.738823649205010868, 4.685061407880516032E-05, -0.1273528623143732053 ) ) ;
#14068 = EDGE_CURVE ( 'NONE', #18488, #38076, #15649, .T. ) ;
#14069 = VERTEX_POINT ( 'NONE', #6888 ) ;
#14070 = CARTESIAN_POINT ( 'NONE',  ( 1.841876542152869556, 1.049866565067837820, -0.8407752411460415187 ) ) ;
#14071 = FACE_OUTER_BOUND ( 'NONE', #42593, .T. ) ;
#14072 = ORIENTED_EDGE ( 'NONE', *, *, #22408, .T. ) ;
#14073 = EDGE_CURVE ( 'NONE', #42740, #10279, #42756, .T. ) ;
#14074 = CARTESIAN_POINT ( 'NONE',  ( 0.2727639067037602172, 3.346456692913386100, -2.088563196121306476 ) ) ;
#14075 = FACE_OUTER_BOUND ( 'NONE', #41368, .T. ) ;
#14076 = EDGE_CURVE ( 'NONE', #19538, #42180, #19011, .T. ) ;
#14077 = AXIS2_PLACEMENT_3D ( 'NONE', #43642, #32568, #24548 ) ;
#14078 = AXIS2_PLACEMENT_3D ( 'NONE', #26285, #6416, #37916 ) ;
#14079 = CARTESIAN_POINT ( 'NONE',  ( 0.8182917201112819283, 3.346456692913386100, -1.299212598425193210 ) ) ;
#14080 = FACE_OUTER_BOUND ( 'NONE', #25351, .T. ) ;
#14081 = DIRECTION ( 'NONE',  ( -0.5877852522924802425, -9.388193118000637501E-17, 0.8090169943749422332 ) ) ;
#14082 = ORIENTED_EDGE ( 'NONE', *, *, #22577, .F. ) ;
#14083 = CARTESIAN_POINT ( 'NONE',  ( -0.7303501086101925610, -2.370459731021293560E-16, 2.086068174627930816 ) ) ;
#14084 = CONICAL_SURFACE ( 'NONE', #5864, 2.244934639244524632, 1.554780866114618743 ) ;
#14085 = FACE_OUTER_BOUND ( 'NONE', #794, .T. ) ;
#14086 = EDGE_CURVE ( 'NONE', #45769, #21117, #39144, .T. ) ;
#14087 = ORIENTED_EDGE ( 'NONE', *, *, #4749, .T. ) ;
#14088 = CARTESIAN_POINT ( 'NONE',  ( 0.1968503937007878568, 3.346456692913386100, 1.259842519685033357 ) ) ;
#14089 = DIRECTION ( 'NONE',  ( -0.9510565162951544194, 0.000000000000000000, 0.3090169943749447312 ) ) ;
#14090 = ORIENTED_EDGE ( 'NONE', *, *, #41590, .T. ) ;
#14091 = CARTESIAN_POINT ( 'NONE',  ( 0.000000000000000000, 3.267716535433071279, 2.362204724409437961 ) ) ;
#14092 = ADVANCED_FACE ( 'NONE', ( #3522, #7151 ), #35027, .F. ) ;
#14093 = DIRECTION ( 'NONE',  ( 0.000000000000000000, 0.000000000000000000, 1.000000000000000000 ) ) ;
#14094 = EDGE_CURVE ( 'NONE', #26280, #50705, #14894, .T. ) ;
#14095 = CARTESIAN_POINT ( 'NONE',  ( 1.015142113812069313, 0.000000000000000000, 0.9055118110236164419 ) ) ;
#14096 = ORIENTED_EDGE ( 'NONE', *, *, #44892, .T. ) ;
#14097 = DIRECTION ( 'NONE',  ( -3.469446951953613696E-16, 0.000000000000000000, -1.000000000000000000 ) ) ;
#14098 = EDGE_LOOP ( 'NONE', ( #34932, #40524, #22103, #49023 ) ) ;
#14099 = LINE ( 'NONE', #23608, #29507 ) ;
#14100 = DIRECTION ( 'NONE',  ( -0.9909497617679331460, 1.562041240006052286E-17, -0.1342332658176667026 ) ) ;
#14101 = CARTESIAN_POINT ( 'NONE',  ( 0.5455278134075217666, 3.346456692913386100, 1.889763779527550369 ) ) ;
#14102 = CARTESIAN_POINT ( 'NONE',  ( -0.6214413264104945434, 3.267716535433071279, -0.3543307086614175816 ) ) ;
#14103 = EDGE_CURVE ( 'NONE', #8395, #43635, #42006, .T. ) ;
#14104 = EDGE_LOOP ( 'NONE', ( #10363, #45341, #39107, #14450, #34690, #15444, #7789, #20422, #9795, #11654, #34573 ) ) ;
#14105 = ORIENTED_EDGE ( 'NONE', *, *, #8985, .F. ) ;
#14106 = CARTESIAN_POINT ( 'NONE',  ( -2.867773316779185677, 0.000000000000000000, -0.7050287376752425450 ) ) ;
#14107 = DIRECTION ( 'NONE',  ( 1.000000000000000000, 0.000000000000000000, 0.000000000000000000 ) ) ;
#14108 = EDGE_LOOP ( 'NONE', ( #11898, #11831, #41244, #44049 ) ) ;
#14109 = AXIS2_PLACEMENT_3D ( 'NONE', #43072, #27080, #15475 ) ;
#14110 = LINE ( 'NONE', #49684, #26458 ) ;
#14111 = VECTOR ( 'NONE', #23951, 39.37007874015748143 ) ;
#14112 = ORIENTED_EDGE ( 'NONE', *, *, #16728, .T. ) ;
#14113 = DIRECTION ( 'NONE',  ( 0.000000000000000000, -1.000000000000000000, 0.000000000000000000 ) ) ;
#14114 = EDGE_CURVE ( 'NONE', #5907, #36192, #38890, .T. ) ;
#14115 = DIRECTION ( 'NONE',  ( 1.000000000000000000, 0.000000000000000000, 0.000000000000000000 ) ) ;
#14116 = VERTEX_POINT ( 'NONE', #15146 ) ;
#14117 = CARTESIAN_POINT ( 'NONE',  ( 1.015142113812069757, 3.267716535433071279, -3.521981712565034361E-16 ) ) ;
#14118 = ORIENTED_EDGE ( 'NONE', *, *, #7056, .T. ) ;
#14119 = VECTOR ( 'NONE', #27362, 39.37007874015748143 ) ;
#14120 = ORIENTED_EDGE ( 'NONE', *, *, #35024, .T. ) ;
#14121 = ADVANCED_FACE ( 'NONE', ( #19258 ), #50699, .F. ) ;
#14122 = AXIS2_PLACEMENT_3D ( 'NONE', #7166, #15159, #30657 ) ;
#14123 = EDGE_CURVE ( 'NONE', #23451, #4391, #34270, .T. ) ;
#14124 = ADVANCED_FACE ( 'NONE', ( #23386 ), #18768, .F. ) ;
#14125 = ORIENTED_EDGE ( 'NONE', *, *, #684, .T. ) ;
#14126 = EDGE_LOOP ( 'NONE', ( #48947, #42024, #24131, #21284 ) ) ;
#14127 = DIRECTION ( 'NONE',  ( -3.469446951953613696E-16, 0.000000000000000000, -1.000000000000000000 ) ) ;
#14128 = ORIENTED_EDGE ( 'NONE', *, *, #10338, .F. ) ;
#14129 = CARTESIAN_POINT ( 'NONE',  ( 1.560669927219590303, 0.000000000000000000, -1.732283464566923170 ) ) ;
#14130 = LINE ( 'NONE', #3270, #31843 ) ;
#14131 = LINE ( 'NONE', #1745, #25569 ) ;
#14132 = EDGE_CURVE ( 'NONE', #643, #15782, #13264, .T. ) ;
#14133 = CARTESIAN_POINT ( 'NONE',  ( 1.087963734054938625, 1.205361022782829114E-17, 1.724994741719410918 ) ) ;
#14134 = CARTESIAN_POINT ( 'NONE',  ( 0.5455278134075211005, 3.346456692913386100, 0.4330708661417287386 ) ) ;
#14135 = ORIENTED_EDGE ( 'NONE', *, *, #23762, .F. ) ;
#14136 = CARTESIAN_POINT ( 'NONE',  ( 1.128956743970954912, 1.693175862103839746, 1.985505143361423697 ) ) ;
#14137 = CARTESIAN_POINT ( 'NONE',  ( 0.000000000000000000, 3.267716535433071279, 0.3149606299212578953 ) ) ;
#14138 = EDGE_CURVE ( 'NONE', #33806, #35465, #2764, .T. ) ;
#14139 = DIRECTION ( 'NONE',  ( 0.000000000000000000, 0.000000000000000000, -1.000000000000000000 ) ) ;
#14140 = CARTESIAN_POINT ( 'NONE',  ( -0.5455278134075208785, 3.267716535433071279, 0.4330708661417290162 ) ) ;
#14141 = VECTOR ( 'NONE', #11029, 39.37007874015748143 ) ;
#14142 = ORIENTED_EDGE ( 'NONE', *, *, #38920, .T. ) ;
#14143 = VECTOR ( 'NONE', #7886, 39.37007874015748143 ) ;
#14144 = LINE ( 'NONE', #2016, #35044 ) ;
#14145 = CARTESIAN_POINT ( 'NONE',  ( -1.738921996492520661, 6.764728787913346618E-05, 0.1249482579781430736 ) ) ;
#14146 = EDGE_LOOP ( 'NONE', ( #35203, #28457, #8194, #30105 ) ) ;
#14147 = CARTESIAN_POINT ( 'NONE',  ( -1.002022727364110688, 1.659044326116128509, -1.967298165164199419 ) ) ;
#14148 = FACE_OUTER_BOUND ( 'NONE', #37016, .T. ) ;
#14149 = EDGE_CURVE ( 'NONE', #2854, #44079, #47869, .T. ) ;
#14150 = EDGE_LOOP ( 'NONE', ( #4734, #8640, #25857, #21717 ) ) ;
#14151 = ADVANCED_FACE ( 'NONE', ( #43764 ), #4037, .T. ) ;
#14152 = CONICAL_SURFACE ( 'NONE', #8408, 2.244934639244524632, 1.554780866114618743 ) ;
#14153 = ORIENTED_EDGE ( 'NONE', *, *, #43250, .T. ) ;
#14154 = LINE ( 'NONE', #15166, #24797 ) ;
#14155 = CARTESIAN_POINT ( 'NONE',  ( -0.2727639067037607723, 3.267716535433071279, -1.102362204724405714 ) ) ;
#14156 = VECTOR ( 'NONE', #19463, 39.37007874015748143 ) ;
#14157 = CARTESIAN_POINT ( 'NONE',  ( -1.909347346926324906, 3.346456692913386100, -0.7874015748031470974 ) ) ;
#14158 = CARTESIAN_POINT ( 'NONE',  ( -2.139020239325885253, 1.673641627049041514, 0.3394120305351381872 ) ) ;
#14159 = CARTESIAN_POINT ( 'NONE',  ( 1.091055626815043311, 0.000000000000000000, 1.377952755905504256 ) ) ;
#14160 = ORIENTED_EDGE ( 'NONE', *, *, #5156, .F. ) ;
#14161 = CARTESIAN_POINT ( 'NONE',  ( -0.2727639067037602727, 0.000000000000000000, 1.220472440944875281 ) ) ;
#14162 = ORIENTED_EDGE ( 'NONE', *, *, #50267, .F. ) ;
#14163 = ORIENTED_EDGE ( 'NONE', *, *, #19897, .T. ) ;
#14164 = DIRECTION ( 'NONE',  ( 0.000000000000000000, -1.000000000000000000, 0.000000000000000000 ) ) ;
#14165 = ORIENTED_EDGE ( 'NONE', *, *, #32567, .F. ) ;
#14166 = CARTESIAN_POINT ( 'NONE',  ( 0.2627480064045706332, 0.000000000000000000, 1.723473835155035605 ) ) ;
#14167 = CARTESIAN_POINT ( 'NONE',  ( 0.2727639067037604947, 3.346456692913386100, -0.7874015748031473194 ) ) ;
#14168 = ORIENTED_EDGE ( 'NONE', *, *, #31643, .F. ) ;
#14169 = CARTESIAN_POINT ( 'NONE',  ( 1.363819533518803029, 3.346456692913386100, -1.732283464566923170 ) ) ;
#14170 = CARTESIAN_POINT ( 'NONE',  ( -0.6214413264104939882, 3.267716535433071279, 1.417322834645662777 ) ) ;
#14171 = LINE ( 'NONE', #18055, #32130 ) ;
#14172 = EDGE_LOOP ( 'NONE', ( #4589, #6324, #16919, #8385 ) ) ;
#14173 = ORIENTED_EDGE ( 'NONE', *, *, #37106, .F. ) ;
#14174 = CARTESIAN_POINT ( 'NONE',  ( 0.1526276323950742364, 1.644729766260672577, -2.244838780058033390 ) ) ;
#14175 = FACE_BOUND ( 'NONE', #37216, .T. ) ;
#14176 = EDGE_LOOP ( 'NONE', ( #49992, #45515, #36708, #49818 ) ) ;
#14177 = AXIS2_PLACEMENT_3D ( 'NONE', #18151, #42140, #38035 ) ;
#14178 = VECTOR ( 'NONE', #49565, 39.37007874015748854 ) ;
#14179 = CARTESIAN_POINT ( 'NONE',  ( -1.387241876633674265, 6.692913385826772199, 1.662624236931676602 ) ) ;
#14180 = CARTESIAN_POINT ( 'NONE',  ( -2.443311489867025621, 3.267716535433071279, -0.03937007874015881204 ) ) ;
#14181 = EDGE_CURVE ( 'NONE', #3351, #28908, #50154, .T. ) ;
#14182 = EDGE_LOOP ( 'NONE', ( #3870, #39293, #28227, #33384 ) ) ;
#14183 = ORIENTED_EDGE ( 'NONE', *, *, #7329, .F. ) ;
#14184 = CARTESIAN_POINT ( 'NONE',  ( -0.4369915662458470074, 0.02092044581182531462, -1.768387524372482034 ) ) ;
#14185 = EDGE_CURVE ( 'NONE', #36209, #39707, #29254, .T. ) ;
#14186 = VECTOR ( 'NONE', #30300, 39.37007874015748143 ) ;
#14187 = CARTESIAN_POINT ( 'NONE',  ( 0.000000000000000000, 2.755905511811024056, 0.000000000000000000 ) ) ;
#14188 = ORIENTED_EDGE ( 'NONE', *, *, #50646, .F. ) ;
#14189 = ORIENTED_EDGE ( 'NONE', *, *, #45169, .F. ) ;
#14190 = AXIS2_PLACEMENT_3D ( 'NONE', #39580, #31329, #34951 ) ;
#14191 = EDGE_LOOP ( 'NONE', ( #45991, #4394, #49761, #5973 ) ) ;
#14192 = CARTESIAN_POINT ( 'NONE',  ( 0.7078551077791208623, 0.5249316475426862860, 1.746015920298445767 ) ) ;
#14193 = VECTOR ( 'NONE', #24189, 39.37007874015748143 ) ;
#14194 = CARTESIAN_POINT ( 'NONE',  ( 1.014069264286641570, 0.000000000000000000, -1.062992125984252301 ) ) ;
#14195 = CARTESIAN_POINT ( 'NONE',  ( 0.8182917201112819283, 3.346456692913386100, -0.1574803149606301411 ) ) ;
#14196 = CARTESIAN_POINT ( 'NONE',  ( 0.4696143004045476577, 0.000000000000000000, -1.732283464566922726 ) ) ;
#14197 = ORIENTED_EDGE ( 'NONE', *, *, #34069, .T. ) ;
#14198 = ORIENTED_EDGE ( 'NONE', *, *, #19760, .T. ) ;
#14199 = CARTESIAN_POINT ( 'NONE',  ( -0.9053572107128330382, 1.602824473448254405, 2.552372930600343981 ) ) ;
#14200 = CARTESIAN_POINT ( 'NONE',  ( 1.692057011007029876, 0.03618185373504610031, -1.057949673616393804 ) ) ;
#14201 = DIRECTION ( 'NONE',  ( -1.000000000000000000, 0.000000000000000000, 1.734723475976806848E-16 ) ) ;
#14202 = EDGE_CURVE ( 'NONE', #4534, #25341, #4635, .T. ) ;
#14203 = CARTESIAN_POINT ( 'NONE',  ( 1.287906020515829919, 3.261681340554358766, -2.079996175279934523 ) ) ;
#14204 = DIRECTION ( 'NONE',  ( -0.000000000000000000, 1.000000000000000000, -0.000000000000000000 ) ) ;
#14205 = EDGE_CURVE ( 'NONE', #39335, #41869, #33514, .T. ) ;
#14206 = CARTESIAN_POINT ( 'NONE',  ( 0.2727639067037604947, 3.267716535433071279, 0.4724409448818868706 ) ) ;
#14207 = CARTESIAN_POINT ( 'NONE',  ( -2.182111253630085290, 3.226699998040846395, -1.141732283464563791 ) ) ;
#14208 = ORIENTED_EDGE ( 'NONE', *, *, #46733, .F. ) ;
#14209 = CARTESIAN_POINT ( 'NONE',  ( 1.560669927219590303, 0.000000000000000000, -1.102362204724405714 ) ) ;
#14210 = LINE ( 'NONE', #34098, #2171 ) ;
#14211 = EDGE_CURVE ( 'NONE', #4521, #10846, #8421, .T. ) ;
#14212 = EDGE_CURVE ( 'NONE', #27610, #22305, #20283, .T. ) ;
#14213 = ORIENTED_EDGE ( 'NONE', *, *, #26104, .T. ) ;
#14214 = ORIENTED_EDGE ( 'NONE', *, *, #49204, .F. ) ;
#14215 = CIRCLE ( 'NONE', #48699, 2.165354330708661568 ) ;
#14216 = CARTESIAN_POINT ( 'NONE',  ( 2.378961647330872786, 0.000000000000000000, 0.3149606299212573401 ) ) ;
#14217 = ORIENTED_EDGE ( 'NONE', *, *, #43080, .F. ) ;
#14218 = VECTOR ( 'NONE', #11315, 39.37007874015748143 ) ;
#14219 = EDGE_LOOP ( 'NONE', ( #17970, #5381, #36359, #23799 ) ) ;
#14220 = LINE ( 'NONE', #45688, #48448 ) ;
#14221 = VECTOR ( 'NONE', #40264, 39.37007874015748143 ) ;
#14222 = ORIENTED_EDGE ( 'NONE', *, *, #27408, .T. ) ;
#14223 = AXIS2_PLACEMENT_3D ( 'NONE', #8997, #11649, #46731 ) ;
#14224 = AXIS2_PLACEMENT_3D ( 'NONE', #14459, #33588, #45415 ) ;
#14225 = CARTESIAN_POINT ( 'NONE',  ( 0.7117868624172632996, 0.000000000000000000, -1.591464117667681366 ) ) ;
#14226 = CARTESIAN_POINT ( 'NONE',  ( -0.7117868624172403180, 0.000000000000000000, -1.591464117667691580 ) ) ;
#14227 = ORIENTED_EDGE ( 'NONE', *, *, #48899, .F. ) ;
#14228 = ORIENTED_EDGE ( 'NONE', *, *, #27063, .T. ) ;
#14229 = CARTESIAN_POINT ( 'NONE',  ( 0.000000000000000000, 0.000000000000000000, 0.000000000000000000 ) ) ;
#14230 = ORIENTED_EDGE ( 'NONE', *, *, #13450, .F. ) ;
#14231 = EDGE_LOOP ( 'NONE', ( #37093, #6688, #4601, #22887 ) ) ;
#14232 = CARTESIAN_POINT ( 'NONE',  ( -0.5756566573089003658, 0.000000000000000000, 2.896516654582634853 ) ) ;
#14233 = DIRECTION ( 'NONE',  ( -0.000000000000000000, 1.000000000000000000, -0.000000000000000000 ) ) ;
#14234 = DIRECTION ( 'NONE',  ( 1.000000000000000000, 0.000000000000000000, -3.469446951953613696E-16 ) ) ;
#14235 = CARTESIAN_POINT ( 'NONE',  ( 0.1968503937007872462, 0.000000000000000000, 0.1181102362204701633 ) ) ;
#14236 = EDGE_LOOP ( 'NONE', ( #36347, #2522, #9541, #51032 ) ) ;
#14237 = CARTESIAN_POINT ( 'NONE',  ( -1.985260859929298238, 0.000000000000000000, -1.141732283464563791 ) ) ;
#14238 = CARTESIAN_POINT ( 'NONE',  ( 1.636583440222563857, 0.000000000000000000, -0.3149606299212596716 ) ) ;
#14239 = DIRECTION ( 'NONE',  ( -1.000000000000000000, 0.000000000000000000, -0.000000000000000000 ) ) ;
#14240 = ORIENTED_EDGE ( 'NONE', *, *, #29423, .F. ) ;
#14241 = DIRECTION ( 'NONE',  ( 1.734723475976806848E-16, 0.000000000000000000, 1.000000000000000000 ) ) ;
#14242 = CARTESIAN_POINT ( 'NONE',  ( -1.232995795418201812, 0.000000000000000000, 1.780798594093550680 ) ) ;
#14243 = EDGE_CURVE ( 'NONE', #41617, #25178, #27510, .T. ) ;
#14244 = EDGE_CURVE ( 'NONE', #33109, #11793, #40177, .T. ) ;
#14245 = LINE ( 'NONE', #29996, #50460 ) ;
#14246 = ORIENTED_EDGE ( 'NONE', *, *, #7668, .T. ) ;
#14247 = ORIENTED_EDGE ( 'NONE', *, *, #32634, .F. ) ;
#14248 = LENGTH_MEASURE_WITH_UNIT ( LENGTH_MEASURE( 0.02539999999999999897 ), #49570 );
#14249 = EDGE_CURVE ( 'NONE', #20677, #48779, #7901, .T. ) ;
#14250 = CARTESIAN_POINT ( 'NONE',  ( 1.560669927219590747, 3.267716535433071279, -5.414661521997677271E-16 ) ) ;
#14251 = DIRECTION ( 'NONE',  ( 0.000000000000000000, -1.000000000000000000, 0.000000000000000000 ) ) ;
#14252 = ADVANCED_FACE ( 'NONE', ( #39401 ), #27771, .F. ) ;
#14253 = CARTESIAN_POINT ( 'NONE',  ( 1.636583440222563857, 0.000000000000000000, 0.9448818897637746295 ) ) ;
#14254 = ORIENTED_EDGE ( 'NONE', *, *, #25727, .F. ) ;
#14255 = B_SPLINE_CURVE_WITH_KNOTS ( 'NONE', 3,
 ( #18388, #41377, #7020, #33642 ),
 .UNSPECIFIED., .F., .F.,
 ( 4, 4 ),
 ( 0.002100519986389839076, 0.003739631879507434968 ),
 .UNSPECIFIED. ) ;
#14256 = EDGE_LOOP ( 'NONE', ( #20216, #9739, #32600, #2962, #11100, #6357, #44422, #26855, #28706, #31454, #22038, #11868, #31711, #34780, #46276, #8947, #37767, #20307, #30803, #38189, #47397, #4955, #47522, #46188, #23216, #44582, #4386, #47251, #35437, #31551, #44402, #44300, #9430, #42013, #15787, #38447, #21267, #37489, #10323, #17086, #32978, #50802, #223, #30263, #44851, #40058, #48363, #6205, #34810, #38426, #27635, #26778, #14939, #21908, #19723, #32427, #15771, #30072, #11766, #24259, #18873, #13672, #44331, #49574, #13504, #43104, #32597, #32425, #50573, #27543, #23130, #41592, #21672, #23695, #4154, #15922, #1431, #39201, #49937, #1545, #11068, #11863, #41826, #29620, #49274, #35233, #42266, #47472, #49879, #31331, #23076, #50119, #27948, #46258, #8964, #28258, #20528, #27225, #27348, #11009, #24275, #22482, #34834, #5144, #41455, #6777, #18798, #11805, #12191, #4510, #2408, #1990, #28683, #3674, #2449, #13631, #12839, #32757, #5097, #38365, #20271, #13919, #11001, #8297, #8367, #31846, #2631, #8678, #45628, #20536, #45247, #29969, #1717, #40238, #40119, #15674, #38013, #50363, #5127, #18128, #13560, #36131, #28657, #39263, #6548, #8602, #16584 ) ) ;
#14257 = VECTOR ( 'NONE', #32417, 39.37007874015748143 ) ;
#14258 = DIRECTION ( 'NONE',  ( 1.000000000000000000, 0.000000000000000000, -3.469446951953613696E-16 ) ) ;
#14259 = ORIENTED_EDGE ( 'NONE', *, *, #26699, .F. ) ;
#14260 = CARTESIAN_POINT ( 'NONE',  ( 1.287906020515830141, 0.000000000000000000, -0.6299212598425181220 ) ) ;
#14261 = CARTESIAN_POINT ( 'NONE',  ( -0.8182917201112814842, 3.267716535433071279, 0.7874015748031456541 ) ) ;
#14262 = VECTOR ( 'NONE', #11140, 39.37007874015748143 ) ;
#14263 = VECTOR ( 'NONE', #41325, 39.37007874015748143 ) ;
#14264 = EDGE_CURVE ( 'NONE', #5331, #20873, #47618, .T. ) ;
#14265 = CARTESIAN_POINT ( 'NONE',  ( 0.2841802383804452603, 0.03247133209088205741, 1.841575167587790718 ) ) ;
#14266 = DIRECTION ( 'NONE',  ( -1.000000000000000000, -0.000000000000000000, -0.000000000000000000 ) ) ;
#14267 = DIRECTION ( 'NONE',  ( -0.000000000000000000, 0.000000000000000000, 1.000000000000000000 ) ) ;
#14268 = AXIS2_PLACEMENT_3D ( 'NONE', #24433, #31932, #32707 ) ;
#14269 = ORIENTED_EDGE ( 'NONE', *, *, #21469, .F. ) ;
#14270 = DIRECTION ( 'NONE',  ( -0.000000000000000000, 1.000000000000000000, -0.000000000000000000 ) ) ;
#14271 = LINE ( 'NONE', #14020, #35922 ) ;
#14272 = EDGE_CURVE ( 'NONE', #50405, #8785, #40435, .T. ) ;
#14273 = CARTESIAN_POINT ( 'NONE',  ( -2.339241080213612545, 1.564176246289736616, 1.802537235681883843 ) ) ;
#14274 = ORIENTED_EDGE ( 'NONE', *, *, #13143, .F. ) ;
#14275 = CARTESIAN_POINT ( 'NONE',  ( 0.1968503937007878568, 3.267716535433071279, 1.889763779527550369 ) ) ;
#14276 = DIRECTION ( 'NONE',  ( -1.000000000000000000, 0.000000000000000000, 1.734723475976806848E-16 ) ) ;
#14277 = FACE_OUTER_BOUND ( 'NONE', #44185, .T. ) ;
#14278 = ORIENTED_EDGE ( 'NONE', *, *, #1344, .T. ) ;
#14279 = CARTESIAN_POINT ( 'NONE',  ( 1.363819533518803251, 0.000000000000000000, 0.5905511811023579360 ) ) ;
#14280 = EDGE_LOOP ( 'NONE', ( #16539, #39390, #43757, #19575 ) ) ;
#14281 = CARTESIAN_POINT ( 'NONE',  ( -1.377952755905513360, 0.000000000000000000, 2.165354330708661568 ) ) ;
#14282 = LINE ( 'NONE', #10156, #12603 ) ;
#14283 = ORIENTED_EDGE ( 'NONE', *, *, #37887, .T. ) ;
#14284 = DIRECTION ( 'NONE',  ( 0.9998717552508121775, 0.01601477604151182663, 0.000000000000000000 ) ) ;
#14285 = EDGE_CURVE ( 'NONE', #22293, #25302, #11973, .T. ) ;
#14286 = DIRECTION ( 'NONE',  ( 1.283101021437938170E-16, 1.000000000000000000, 1.154811821032258155E-17 ) ) ;
#14287 = CARTESIAN_POINT ( 'NONE',  ( -0.2727639067037607723, 3.346456692913386100, -0.4724409448818883694 ) ) ;
#14288 = LINE ( 'NONE', #1910, #32638 ) ;
#14289 = VECTOR ( 'NONE', #11131, 39.37007874015748143 ) ;
#14290 = VERTEX_POINT ( 'NONE', #36301 ) ;
#14291 = EDGE_LOOP ( 'NONE', ( #24536, #38930, #12081, #49179, #25326, #14823, #10687, #17963, #48541, #38757, #43365, #8049, #30996, #32046, #27450, #35687, #11554, #2683, #41301 ) ) ;
#14292 = DIRECTION ( 'NONE',  ( -3.469446951953613696E-16, 0.000000000000000000, -1.000000000000000000 ) ) ;
#14293 = PLANE ( 'NONE',  #41164 ) ;
#14294 = ORIENTED_EDGE ( 'NONE', *, *, #10303, .T. ) ;
#14295 = VECTOR ( 'NONE', #16117, 39.37007874015748143 ) ;
#14296 = CARTESIAN_POINT ( 'NONE',  ( -1.744243240276440732, -1.725014817524629540E-16, 1.328042291889479865 ) ) ;
#14297 = DIRECTION ( 'NONE',  ( -3.469446951953613696E-16, 0.000000000000000000, -1.000000000000000000 ) ) ;
#14298 = DIRECTION ( 'NONE',  ( 1.734723475976806848E-16, -0.000000000000000000, 1.000000000000000000 ) ) ;
#14299 = VECTOR ( 'NONE', #3501, 39.37007874015748143 ) ;
#14300 = VECTOR ( 'NONE', #23782, 39.37007874015748143 ) ;
#14301 = ORIENTED_EDGE ( 'NONE', *, *, #43024, .T. ) ;
#14302 = EDGE_LOOP ( 'NONE', ( #38263, #31079, #15296, #24386 ) ) ;
#14303 = B_SPLINE_CURVE_WITH_KNOTS ( 'NONE', 3,
 ( #29139, #24513, #32264, #28631 ),
 .UNSPECIFIED., .F., .F.,
 ( 4, 4 ),
 ( 1.642879463944005381E-05, 0.05043055294521734538 ),
 .UNSPECIFIED. ) ;
#14304 = CARTESIAN_POINT ( 'NONE',  ( 1.539674616754186820, 0.000000000000000000, -1.403993126671013059 ) ) ;
#14305 = CARTESIAN_POINT ( 'NONE',  ( -1.636583440222564523, 3.267716535433071279, 2.839019714148967570E-16 ) ) ;
#14306 = DIRECTION ( 'NONE',  ( -3.986037398843765983E-20, -1.000000000000000000, -1.160734090543304660E-16 ) ) ;
#14307 = VERTEX_POINT ( 'NONE', #31657 ) ;
#14308 = PLANE ( 'NONE',  #951 ) ;
#14309 = FACE_BOUND ( 'NONE', #16392, .T. ) ;
#14310 = CONICAL_SURFACE ( 'NONE', #47235, 2.244934639244524632, 1.554780866114618743 ) ;
#14311 = ORIENTED_EDGE ( 'NONE', *, *, #26092, .F. ) ;
#14312 = EDGE_CURVE ( 'NONE', #45331, #33133, #23906, .T. ) ;
#14313 = CARTESIAN_POINT ( 'NONE',  ( -1.091055626815042645, 3.346456692913386100, -1.889763779527552146 ) ) ;
#14314 = ORIENTED_EDGE ( 'NONE', *, *, #15975, .T. ) ;
#14315 = ORIENTED_EDGE ( 'NONE', *, *, #48775, .T. ) ;
#14316 = DIRECTION ( 'NONE',  ( 0.000000000000000000, -0.7071067811865479058, 0.7071067811865470176 ) ) ;
#14317 = CARTESIAN_POINT ( 'NONE',  ( 1.560669927219590747, 0.000000000000000000, -0.1574803149606304187 ) ) ;
#14318 = EDGE_CURVE ( 'NONE', #9214, #30067, #35784, .T. ) ;
#14319 = CARTESIAN_POINT ( 'NONE',  ( -1.738889418803986064, 2.342530735446346105E-05, -0.1273558160304689713 ) ) ;
#14320 = ADVANCED_FACE ( 'NONE', ( #412 ), #31924, .F. ) ;
#14321 = ORIENTED_EDGE ( 'NONE', *, *, #2655, .T. ) ;
#14322 = LINE ( 'NONE', #22833, #39273 ) ;
#14323 = EDGE_CURVE ( 'NONE', #26865, #33493, #21213, .T. ) ;
#14324 = LINE ( 'NONE', #10199, #11494 ) ;
#14325 = ORIENTED_EDGE ( 'NONE', *, *, #6255, .T. ) ;
#14326 = ORIENTED_EDGE ( 'NONE', *, *, #28011, .T. ) ;
#14327 = CARTESIAN_POINT ( 'NONE',  ( -1.014069264286641570, 0.4235180831842794702, -1.062992125984252301 ) ) ;
#14328 = CARTESIAN_POINT ( 'NONE',  ( -2.119913818043088316, 1.678103251997176359, 1.196659857809422300 ) ) ;
#14329 = EDGE_CURVE ( 'NONE', #24374, #36538, #32697, .T. ) ;
#14330 = CARTESIAN_POINT ( 'NONE',  ( 0.000000000000000000, 3.267716535433071279, 0.1574803149606286423 ) ) ;
#14331 = AXIS2_PLACEMENT_3D ( 'NONE', #36804, #40675, #1427 ) ;
#14332 = LINE ( 'NONE', #18209, #35223 ) ;
#14333 = DIRECTION ( 'NONE',  ( -1.000000000000000000, -0.000000000000000000, -0.000000000000000000 ) ) ;
#14334 = ORIENTED_EDGE ( 'NONE', *, *, #45825, .F. ) ;
#14335 = CARTESIAN_POINT ( 'NONE',  ( 2.708690932417664232, 1.452543555714349788, -1.175597808493610952 ) ) ;
#14336 = EDGE_CURVE ( 'NONE', #3944, #9810, #2215, .T. ) ;
#14337 = VECTOR ( 'NONE', #29131, 39.37007874015748143 ) ;
#14338 = PLANE ( 'NONE',  #21560 ) ;
#14339 = VECTOR ( 'NONE', #23364, 39.37007874015748143 ) ;
#14340 = VECTOR ( 'NONE', #2590, 39.37007874015748143 ) ;
#14341 = ORIENTED_EDGE ( 'NONE', *, *, #14055, .T. ) ;
#14342 = DIRECTION ( 'NONE',  ( 1.734723475976806848E-16, -0.000000000000000000, 1.000000000000000000 ) ) ;
#14343 = PLANE ( 'NONE',  #39339 ) ;
#14344 = EDGE_LOOP ( 'NONE', ( #44254, #23480, #9005, #43626 ) ) ;
#14345 = DIRECTION ( 'NONE',  ( -0.000000000000000000, 1.000000000000000000, -0.000000000000000000 ) ) ;
#14346 = EDGE_CURVE ( 'NONE', #43159, #40619, #17192, .T. ) ;
#14347 = CARTESIAN_POINT ( 'NONE',  ( -1.522953965282238586, 0.003526770554233742919, 0.8754220627670087351 ) ) ;
#14348 = PLANE ( 'NONE',  #14477 ) ;
#14349 = AXIS2_PLACEMENT_3D ( 'NONE', #28675, #32837, #5187 ) ;
#14350 = ORIENTED_EDGE ( 'NONE', *, *, #24049, .T. ) ;
#14351 = CARTESIAN_POINT ( 'NONE',  ( -0.9146000759343694275, 1.693252956796532871, -2.012610095043610769 ) ) ;
#14352 = ORIENTED_EDGE ( 'NONE', *, *, #14475, .T. ) ;
#14353 = CARTESIAN_POINT ( 'NONE',  ( 0.000000000000000000, 3.267716535433071279, 0.000000000000000000 ) ) ;
#14354 = EDGE_CURVE ( 'NONE', #31439, #23113, #5818, .T. ) ;
#14355 = DIRECTION ( 'NONE',  ( 0.9998717552508121775, 0.01601477604151182663, 0.000000000000000000 ) ) ;
#14356 = DIRECTION ( 'NONE',  ( -3.469446951953613696E-16, 0.000000000000000000, -1.000000000000000000 ) ) ;
#14357 = LINE ( 'NONE', #33744, #27623 ) ;
#14358 = ORIENTED_EDGE ( 'NONE', *, *, #11180, .T. ) ;
#14359 = VERTEX_POINT ( 'NONE', #6335 ) ;
#14360 = DIRECTION ( 'NONE',  ( 0.000000000000000000, 0.000000000000000000, -1.000000000000000000 ) ) ;
#14361 = EDGE_CURVE ( 'NONE', #42073, #25538, #45041, .T. ) ;
#14362 = DIRECTION ( 'NONE',  ( -0.000000000000000000, 1.000000000000000000, -0.000000000000000000 ) ) ;
#14363 = CARTESIAN_POINT ( 'NONE',  ( -1.252433315296644256, 1.589416742343778610, -1.807552045033091082 ) ) ;
#14364 = EDGE_LOOP ( 'NONE', ( #17665, #49485, #25925, #1848 ) ) ;
#14365 = EDGE_CURVE ( 'NONE', #13884, #575, #29313, .T. ) ;
#14366 = LINE ( 'NONE', #25473, #30596 ) ;
#14367 = ORIENTED_EDGE ( 'NONE', *, *, #14506, .F. ) ;
#14368 = LINE ( 'NONE', #25991, #21628 ) ;
#14369 = VECTOR ( 'NONE', #50885, 39.37007874015748143 ) ;
#14370 = LINE ( 'NONE', #3008, #37195 ) ;
#14371 = CIRCLE ( 'NONE', #33332, 2.246510896728926010 ) ;
#14372 = VERTEX_POINT ( 'NONE', #49147 ) ;
#14373 = CARTESIAN_POINT ( 'NONE',  ( -1.166969139818015755, 3.267716535433071279, 4.048737525165544676E-16 ) ) ;
#14374 = AXIS2_PLACEMENT_3D ( 'NONE', #20730, #24356, #21501 ) ;
#14375 = ORIENTED_EDGE ( 'NONE', *, *, #13843, .T. ) ;
#14376 = ORIENTED_EDGE ( 'NONE', *, *, #50908, .F. ) ;
#14377 = AXIS2_PLACEMENT_3D ( 'NONE', #17412, #2175, #17671 ) ;
#14378 = EDGE_CURVE ( 'NONE', #38642, #39685, #22808, .T. ) ;
#14379 = CONICAL_SURFACE ( 'NONE', #37495, 2.422428857167389982, 0.4363323129985800519 ) ;
#14380 = VERTEX_POINT ( 'NONE', #24931 ) ;
#14381 = ORIENTED_EDGE ( 'NONE', *, *, #25264, .T. ) ;
#14382 = CARTESIAN_POINT ( 'NONE',  ( 0.000000000000000000, 0.000000000000000000, -2.106299212598425008 ) ) ;
#14383 = ADVANCED_FACE ( 'NONE', ( #5306 ), #1689, .F. ) ;
#14384 = VECTOR ( 'NONE', #49224, 39.37007874015748143 ) ;
#14385 = VERTEX_POINT ( 'NONE', #45539 ) ;
#14386 = CARTESIAN_POINT ( 'NONE',  ( -1.038530695135446713, 0.4479795140330846137, 1.025452293874513199 ) ) ;
#14387 = DIRECTION ( 'NONE',  ( 1.000000000000000000, 0.000000000000000000, -3.469446951953613696E-16 ) ) ;
#14388 = CARTESIAN_POINT ( 'NONE',  ( -1.636583440222564301, 0.000000000000000000, -0.3149606299212592275 ) ) ;
#14389 = LINE ( 'NONE', #37646, #33549 ) ;
#14390 = LINE ( 'NONE', #42012, #23696 ) ;
#14391 = ORIENTED_EDGE ( 'NONE', *, *, #34, .F. ) ;
#14392 = CARTESIAN_POINT ( 'NONE',  ( -1.091055626815042645, 0.000000000000000000, 2.204724409448808764 ) ) ;
#14393 = CARTESIAN_POINT ( 'NONE',  ( 1.018961996185594021, 0.04424020667788951949, 1.609505285524495344 ) ) ;
#14394 = DIRECTION ( 'NONE',  ( 0.01601477604151182663, -0.9998717552508123996, 0.000000000000000000 ) ) ;
#14395 = LINE ( 'NONE', #44856, #18267 ) ;
#14396 = ORIENTED_EDGE ( 'NONE', *, *, #10047, .T. ) ;
#14397 = LINE ( 'NONE', #26518, #10839 ) ;
#14398 = DIRECTION ( 'NONE',  ( 1.000000000000000000, 0.000000000000000000, 0.000000000000000000 ) ) ;
#14399 = ORIENTED_EDGE ( 'NONE', *, *, #17860, .F. ) ;
#14400 = CARTESIAN_POINT ( 'NONE',  ( 0.000000000000000000, 3.267716535433071279, 0.000000000000000000 ) ) ;
#14401 = EDGE_CURVE ( 'NONE', #10925, #11129, #40939, .T. ) ;
#14402 = CARTESIAN_POINT ( 'NONE',  ( 1.909347346926324462, 3.267716535433071279, -1.299212598425194320 ) ) ;
#14403 = APPLICATION_CONTEXT ( 'automotive_design' ) ;
#14404 = ORIENTED_EDGE ( 'NONE', *, *, #15757, .F. ) ;
#14405 = VECTOR ( 'NONE', #48886, 39.37007874015748143 ) ;
#14406 = CONICAL_SURFACE ( 'NONE', #18538, 2.165354330708661568, 0.2617993877991570129 ) ;
#14407 = EDGE_LOOP ( 'NONE', ( #40588, #13182, #30030, #31593 ) ) ;
#14408 = CARTESIAN_POINT ( 'NONE',  ( -1.217629348859213367, 1.696353326100507042, -2.415009927941460077 ) ) ;
#14409 = ADVANCED_FACE ( 'NONE', ( #29049 ), #9949, .F. ) ;
#14410 = VECTOR ( 'NONE', #40709, 39.37007874015748143 ) ;
#14412 = AXIS2_PLACEMENT_3D ( 'NONE', #34730, #23100, #50662 ) ;
#14411 = PLANE ( 'NONE',  #2805 ) ;
#14413 = FACE_OUTER_BOUND ( 'NONE', #9361, .T. ) ;
#14414 = EDGE_CURVE ( 'NONE', #29717, #32803, #16941, .T. ) ;
#14415 = PLANE ( 'NONE',  #47306 ) ;
#14416 = CARTESIAN_POINT ( 'NONE',  ( 1.636583440222563857, 3.346456692913386100, 0.9448818897637746295 ) ) ;
#14417 = ORIENTED_EDGE ( 'NONE', *, *, #26557, .T. ) ;
#14418 = EDGE_CURVE ( 'NONE', #15165, #44082, #28799, .T. ) ;
#14419 = CARTESIAN_POINT ( 'NONE',  ( 0.000000000000000000, 2.755905511811024056, 0.000000000000000000 ) ) ;
#14420 = VECTOR ( 'NONE', #40710, 39.37007874015748143 ) ;
#14421 = ORIENTED_EDGE ( 'NONE', *, *, #48463, .F. ) ;
#14422 = ORIENTED_EDGE ( 'NONE', *, *, #9644, .F. ) ;
#14423 = LINE ( 'NONE', #30167, #38614 ) ;
#14424 = ORIENTED_EDGE ( 'NONE', *, *, #32560, .F. ) ;
#14425 = EDGE_CURVE ( 'NONE', #33393, #8577, #9443, .T. ) ;
#14426 = LINE ( 'NONE', #30169, #35341 ) ;
#14427 = DIRECTION ( 'NONE',  ( 1.000000000000000000, 0.000000000000000000, -3.469446951953613696E-16 ) ) ;
#14428 = ORIENTED_EDGE ( 'NONE', *, *, #5584, .T. ) ;
#14429 = LINE ( 'NONE', #14169, #9103 ) ;
#14430 = CARTESIAN_POINT ( 'NONE',  ( 1.636583440222563635, 3.346456692913386100, -0.9448818897637765168 ) ) ;
#14431 = CARTESIAN_POINT ( 'NONE',  ( -2.182111253630085734, 3.346456692913386100, -0.6299212598425177889 ) ) ;
#14432 = VERTEX_POINT ( 'NONE', #32956 ) ;
#14433 = ORIENTED_EDGE ( 'NONE', *, *, #7346, .F. ) ;
#14434 = DIRECTION ( 'NONE',  ( -1.000000000000000000, 0.000000000000000000, 1.734723475976806848E-16 ) ) ;
#14435 = FACE_BOUND ( 'NONE', #27714, .T. ) ;
#14436 = ORIENTED_EDGE ( 'NONE', *, *, #27641, .T. ) ;
#14437 = EDGE_CURVE ( 'NONE', #24910, #41415, #37070, .T. ) ;
#14438 = CARTESIAN_POINT ( 'NONE',  ( 1.915720322920900331, 0.05860343245220329955, -0.3867724703730804348 ) ) ;
#14439 = CARTESIAN_POINT ( 'NONE',  ( -2.447166048624850543, 3.259451480409341961, -0.03937007874015881204 ) ) ;
#14440 = ORIENTED_EDGE ( 'NONE', *, *, #9791, .F. ) ;
#14441 = VERTEX_POINT ( 'NONE', #48884 ) ;
#14442 = EDGE_CURVE ( 'NONE', #23316, #640, #30218, .T. ) ;
#14443 = CARTESIAN_POINT ( 'NONE',  ( -1.636583440222564301, 3.346456692913386100, -0.9448818897637762948 ) ) ;
#14444 = VECTOR ( 'NONE', #26578, 39.37007874015748854 ) ;
#14445 = EDGE_CURVE ( 'NONE', #640, #22920, #21061, .T. ) ;
#14446 = DIRECTION ( 'NONE',  ( 0.000000000000000000, 0.7071067811865482389, 0.7071067811865467956 ) ) ;
#14447 = AXIS2_PLACEMENT_3D ( 'NONE', #428, #35549, #16186 ) ;
#14448 = VERTEX_POINT ( 'NONE', #42941 ) ;
#14449 = VECTOR ( 'NONE', #47944, 39.37007874015748854 ) ;
#14450 = ORIENTED_EDGE ( 'NONE', *, *, #14086, .T. ) ;
#14451 = CIRCLE ( 'NONE', #45741, 2.086614173228346303 ) ;
#14452 = VERTEX_POINT ( 'NONE', #45795 ) ;
#14453 = CARTESIAN_POINT ( 'NONE',  ( -0.8182917201112819283, 3.346456692913386100, -1.417322834645664331 ) ) ;
#14454 = CARTESIAN_POINT ( 'NONE',  ( -0.1613169216229337344, 0.000000000000000000, -0.3340583758975808060 ) ) ;
#14455 = CARTESIAN_POINT ( 'NONE',  ( -1.363819533518803029, 3.346456692913386100, -0.03937007874015868020 ) ) ;
#14456 = ORIENTED_EDGE ( 'NONE', *, *, #2882, .T. ) ;
#14457 = EDGE_LOOP ( 'NONE', ( #46793, #48518, #24245, #1519 ) ) ;
#14458 = VECTOR ( 'NONE', #47324, 39.37007874015748143 ) ;
#14459 = CARTESIAN_POINT ( 'NONE',  ( 0.08139965876239094178, 1.610780518492231694, 0.000000000000000000 ) ) ;
#14460 = PLANE ( 'NONE',  #712 ) ;
#14461 = CARTESIAN_POINT ( 'NONE',  ( 0.9914495361338622192, 1.493354361723550294, 2.781765111341823360 ) ) ;
#14462 = CARTESIAN_POINT ( 'NONE',  ( -0.4462167695814984736, 1.635138177150359473, 2.183244083262989133 ) ) ;
#14463 = CARTESIAN_POINT ( 'NONE',  ( 0.07982360342473591996, 1.709180471932028711, 0.000000000000000000 ) ) ;
#14464 = CARTESIAN_POINT ( 'NONE',  ( -2.182111253630085290, 3.267716535433071279, 3.785359618865288779E-16 ) ) ;
#14465 = DIRECTION ( 'NONE',  ( -0.9839295885986321100, -2.068648768805177565E-17, 0.1785568947986229116 ) ) ;
#14466 = ORIENTED_EDGE ( 'NONE', *, *, #14361, .T. ) ;
#14467 = CARTESIAN_POINT ( 'NONE',  ( 1.971247363764868199, 6.692913385826772199, -0.8960709840011631400 ) ) ;
#14468 = DIRECTION ( 'NONE',  ( 1.000000000000000000, -0.000000000000000000, 0.000000000000000000 ) ) ;
#14469 = EDGE_LOOP ( 'NONE', ( #35871, #22062, #11247, #18472 ) ) ;
#14470 = ORIENTED_EDGE ( 'NONE', *, *, #5516, .T. ) ;
#14471 = LINE ( 'NONE', #38972, #22075 ) ;
#14472 = EDGE_CURVE ( 'NONE', #41084, #29009, #42194, .T. ) ;
#14473 = ORIENTED_EDGE ( 'NONE', *, *, #35858, .T. ) ;
#14474 = EDGE_CURVE ( 'NONE', #16004, #14001, #14587, .T. ) ;
#14475 = EDGE_CURVE ( 'NONE', #9482, #11793, #30360, .T. ) ;
#14476 = AXIS2_PLACEMENT_3D ( 'NONE', #10146, #33407, #41643 ) ;
#14477 = AXIS2_PLACEMENT_3D ( 'NONE', #2484, #3486, #30352 ) ;
#14478 = VERTEX_POINT ( 'NONE', #22579 ) ;
#14479 = LINE ( 'NONE', #50049, #28692 ) ;
#14480 = AXIS2_PLACEMENT_3D ( 'NONE', #9593, #45187, #16833 ) ;
#14481 = ORIENTED_EDGE ( 'NONE', *, *, #14323, .F. ) ;
#14482 = EDGE_CURVE ( 'NONE', #508, #41536, #38340, .T. ) ;
#14483 = CARTESIAN_POINT ( 'NONE',  ( 2.310037925956077043, 1.712093036975697258, 0.2632538465654825632 ) ) ;
#14484 = CARTESIAN_POINT ( 'NONE',  ( -1.363819533518803473, 0.000000000000000000, -0.4724409448818886470 ) ) ;
#14485 = VECTOR ( 'NONE', #12650, 39.37007874015748143 ) ;
#14486 = VERTEX_POINT ( 'NONE', #50643 ) ;
#14487 = ORIENTED_EDGE ( 'NONE', *, *, #34094, .F. ) ;
#14488 = VECTOR ( 'NONE', #7556, 39.37007874015748143 ) ;
#14489 = CARTESIAN_POINT ( 'NONE',  ( 0.000000000000000000, 3.267716535433071279, 0.6299212598425164567 ) ) ;
#14490 = ORIENTED_EDGE ( 'NONE', *, *, #39213, .T. ) ;
#14491 = ORIENTED_EDGE ( 'NONE', *, *, #31732, .F. ) ;
#14492 = CARTESIAN_POINT ( 'NONE',  ( -0.2906532981117672110, 1.205361022782829114E-17, 1.877244666688175245 ) ) ;
#14493 = PLANE ( 'NONE',  #44129 ) ;
#14494 = CARTESIAN_POINT ( 'NONE',  ( 1.833433833923351353, 0.000000000000000000, 0.6299212598425164567 ) ) ;
#14495 = LINE ( 'NONE', #5732, #10479 ) ;
#14496 = EDGE_CURVE ( 'NONE', #28725, #18986, #46053, .T. ) ;
#14497 = VERTEX_POINT ( 'NONE', #7093 ) ;
#14498 = EDGE_CURVE ( 'NONE', #44517, #5052, #3469, .T. ) ;
#14499 = DIRECTION ( 'NONE',  ( 0.01601477604151182663, -0.9998717552508123996, 0.000000000000000000 ) ) ;
#14500 = FACE_OUTER_BOUND ( 'NONE', #29321, .T. ) ;
#14501 = CARTESIAN_POINT ( 'NONE',  ( -1.909347346926324462, 0.000000000000000000, -0.03937007874015881204 ) ) ;
#14502 = EDGE_LOOP ( 'NONE', ( #33235, #18405, #16717, #40333 ) ) ;
#14503 = ADVANCED_FACE ( 'NONE', ( #19203 ), #50397, .F. ) ;
#14504 = CARTESIAN_POINT ( 'NONE',  ( -2.168245791271168788, 1.205361022782829114E-17, -2.004968704497279486 ) ) ;
#14505 = CARTESIAN_POINT ( 'NONE',  ( -1.091055626815042201, 3.346456692913386100, 1.574803149606291974 ) ) ;
#14506 = EDGE_CURVE ( 'NONE', #47754, #10447, #34214, .T. ) ;
#14507 = VERTEX_POINT ( 'NONE', #30837 ) ;
#14508 = ORIENTED_EDGE ( 'NONE', *, *, #20433, .T. ) ;
#14509 = SHAPE_REPRESENTATION_RELATIONSHIP ( 'NONE' , 'NONE' ,  #36385, #31660 ) ;
#14510 = ADVANCED_FACE ( 'NONE', ( #26449 ), #23331, .F. ) ;
#14511 = FACE_OUTER_BOUND ( 'NONE', #37314, .T. ) ;
#14512 = DIRECTION ( 'NONE',  ( 1.000000000000000000, -0.000000000000000000, 0.000000000000000000 ) ) ;
#14513 = PLANE ( 'NONE',  #42007 ) ;
#14514 = VERTEX_POINT ( 'NONE', #26203 ) ;
#14515 = ORIENTED_EDGE ( 'NONE', *, *, #7495, .T. ) ;
#14516=STYLED_ITEM('',(#51101),#24040);
#14517 = DIRECTION ( 'NONE',  ( -3.469446951953613696E-16, 0.000000000000000000, -1.000000000000000000 ) ) ;
#14518 = VECTOR ( 'NONE', #8930, 39.37007874015748143 ) ;
#14519 = CARTESIAN_POINT ( 'NONE',  ( 0.000000000000000000, 3.346456692913386100, 0.000000000000000000 ) ) ;
#14520 = ORIENTED_EDGE ( 'NONE', *, *, #7017, .T. ) ;
#14521 = DIRECTION ( 'NONE',  ( 0.3090169943749447867, 1.288287287306305776E-16, 0.9510565162951545304 ) ) ;
#14522 = CARTESIAN_POINT ( 'NONE',  ( 0.000000000000000000, 3.267716535433071279, 0.000000000000000000 ) ) ;
#14523 = CIRCLE ( 'NONE', #32673, 2.244934639244525076 ) ;
#14524 = AXIS2_PLACEMENT_3D ( 'NONE', #36904, #48719, #5656 ) ;
#14525 = DIRECTION ( 'NONE',  ( 0.9998717552508121775, 0.01601477604151182663, 0.000000000000000000 ) ) ;
#14526 = CARTESIAN_POINT ( 'NONE',  ( 0.3530705266098149164, -0.6299212598425202314, -0.1234057657284599735 ) ) ;
#14527 = CARTESIAN_POINT ( 'NONE',  ( -1.439733046521776583, 0.000000000000000000, -0.3149606299212592275 ) ) ;
#14528 = VECTOR ( 'NONE', #48164, 39.37007874015748143 ) ;
#14529 = VERTEX_POINT ( 'NONE', #10960 ) ;
#14530 = CARTESIAN_POINT ( 'NONE',  ( -0.07591351300297340121, 3.267716535433071279, -1.614173228346451605 ) ) ;
#14531 = CARTESIAN_POINT ( 'NONE',  ( 0.000000000000000000, 6.692913385826772199, 0.000000000000000000 ) ) ;
#14532 = B_SPLINE_CURVE_WITH_KNOTS ( 'NONE', 3,
 ( #33244, #29353, #4848, #9742 ),
 .UNSPECIFIED., .F., .F.,
 ( 4, 4 ),
 ( 0.1211775127643062860, 0.1625894504277921315 ),
 .UNSPECIFIED. ) ;
#14533 = DIRECTION ( 'NONE',  ( -1.000000000000000000, 0.000000000000000000, 1.734723475976806848E-16 ) ) ;
#14534 = ORIENTED_EDGE ( 'NONE', *, *, #46347, .T. ) ;
#14535 = PLANE ( 'NONE',  #29828 ) ;
#14536 = CARTESIAN_POINT ( 'NONE',  ( 0.000000000000000000, 0.000000000000000000, 0.000000000000000000 ) ) ;
#14537 = CARTESIAN_POINT ( 'NONE',  ( 2.919426793319799707, 1.448220119383965443, 0.4451252810446820196 ) ) ;
#14538 = ORIENTED_EDGE ( 'NONE', *, *, #36203, .T. ) ;
#14539 = DIRECTION ( 'NONE',  ( -1.000000000000000000, 0.000000000000000000, -0.000000000000000000 ) ) ;
#14540 = EDGE_CURVE ( 'NONE', #17362, #20582, #2707, .T. ) ;
#14541 = EDGE_CURVE ( 'NONE', #41218, #19504, #38089, .T. ) ;
#14542 = VERTEX_POINT ( 'NONE', #50152 ) ;
#14543 = DIRECTION ( 'NONE',  ( -1.000000000000000000, 0.000000000000000000, -0.000000000000000000 ) ) ;
#14544 = ORIENTED_EDGE ( 'NONE', *, *, #40164, .F. ) ;
#14545 = DIRECTION ( 'NONE',  ( -0.01601477604151182663, 0.9998717552508123996, -0.000000000000000000 ) ) ;
#14546 = EDGE_CURVE ( 'NONE', #7441, #43525, #46546, .T. ) ;
#14547 = CARTESIAN_POINT ( 'NONE',  ( 1.909347346926324684, 0.000000000000000000, 0.7874015748031456541 ) ) ;
#14548 = CARTESIAN_POINT ( 'NONE',  ( 1.236813753895252166, 1.738537790538875027, -2.681693691597563767 ) ) ;
#14549 = CARTESIAN_POINT ( 'NONE',  ( 0.5455278134075211005, 3.346456692913386100, -0.8267716535433055070 ) ) ;
#14550 = CIRCLE ( 'NONE', #2981, 2.165354330708661568 ) ;
#14551 = ORIENTED_EDGE ( 'NONE', *, *, #21861, .T. ) ;
#14552 = ORIENTED_EDGE ( 'NONE', *, *, #42754, .T. ) ;
#14553 = CARTESIAN_POINT ( 'NONE',  ( 0.000000000000000000, 3.267716535433071279, 0.4330708661417287386 ) ) ;
#14554 = VECTOR ( 'NONE', #37630, 39.37007874015748143 ) ;
#14555 = CARTESIAN_POINT ( 'NONE',  ( 0.4178893628429313778, -0.2057703422145253647, 0.1726618182594314710 ) ) ;
#14556 = AXIS2_PLACEMENT_3D ( 'NONE', #35214, #32118, #47551 ) ;
#14557 = VERTEX_POINT ( 'NONE', #34711 ) ;
#14558 = DIRECTION ( 'NONE',  ( -1.000000000000000000, 0.000000000000000000, 0.000000000000000000 ) ) ;
#14559 = DIRECTION ( 'NONE',  ( -1.000000000000000000, -0.000000000000000000, -0.000000000000000000 ) ) ;
#14560 = DIRECTION ( 'NONE',  ( -0.9998717552508122886, -0.01601477604151185785, 0.000000000000000000 ) ) ;
#14561 = AXIS2_PLACEMENT_3D ( 'NONE', #21290, #33434, #9672 ) ;
#14562 = ORIENTED_EDGE ( 'NONE', *, *, #5961, .F. ) ;
#14563 = ORIENTED_EDGE ( 'NONE', *, *, #33964, .F. ) ;
#14564 = EDGE_CURVE ( 'NONE', #5216, #17026, #2464, .T. ) ;
#14565 = CARTESIAN_POINT ( 'NONE',  ( 1.363819533518803251, 3.346456692913386100, 0.7874015748031454320 ) ) ;
#14566 = DIRECTION ( 'NONE',  ( 1.000000000000000000, -0.000000000000000000, 0.000000000000000000 ) ) ;
#14567 = AXIS2_PLACEMENT_3D ( 'NONE', #22421, #49730, #13913 ) ;
#14568 = CARTESIAN_POINT ( 'NONE',  ( 2.182111253630085290, 0.000000000000000000, 0.6299212598425161236 ) ) ;
#14569 = VERTEX_POINT ( 'NONE', #42449 ) ;
#14570 = DIRECTION ( 'NONE',  ( -0.000000000000000000, 1.000000000000000000, -1.156482317317871478E-16 ) ) ;
#14572 = VECTOR ( 'NONE', #34188, 39.37007874015748143 ) ;
#14571 = DIRECTION ( 'NONE',  ( 1.442222014787672788E-15, -0.7071067811865483499, -0.7071067811865465735 ) ) ;
#14573 = EDGE_LOOP ( 'NONE', ( #5067, #17796, #10135, #10129 ) ) ;
#14574 = EDGE_CURVE ( 'NONE', #7189, #46760, #42700, .T. ) ;
#14575 = EDGE_CURVE ( 'NONE', #10297, #26402, #18201, .T. ) ;
#14576 = CARTESIAN_POINT ( 'NONE',  ( -0.3486774197067340486, 3.346456692913386100, -1.456692913385822630 ) ) ;
#14577 = ORIENTED_EDGE ( 'NONE', *, *, #5684, .F. ) ;
#14578 = ORIENTED_EDGE ( 'NONE', *, *, #36631, .F. ) ;
#14579 = CARTESIAN_POINT ( 'NONE',  ( 2.014645367436137313, 1.707361785030628853, 1.140012488971987592 ) ) ;
#14580 = CARTESIAN_POINT ( 'NONE',  ( 1.015142113812069091, 0.000000000000000000, -1.929133858267711110 ) ) ;
#14581 = B_SPLINE_CURVE_WITH_KNOTS ( 'NONE', 3,
 ( #42578, #3337, #30965, #46922 ),
 .UNSPECIFIED., .F., .F.,
 ( 4, 4 ),
 ( 4.306281158823199186E-05, 0.05047191582401886617 ),
 .UNSPECIFIED. ) ;
#14582 = CARTESIAN_POINT ( 'NONE',  ( 1.287906020515830363, 3.267716535433071279, -4.468321617281356063E-16 ) ) ;
#14583 = CARTESIAN_POINT ( 'NONE',  ( 2.147141360900377105, 5.905511811023623991, 0.3405121111982931659 ) ) ;
#14584 = CARTESIAN_POINT ( 'NONE',  ( 1.091055626815042645, 0.000000000000000000, -0.6299212598425181220 ) ) ;
#14585 = ORIENTED_EDGE ( 'NONE', *, *, #48119, .F. ) ;
#14586 = ORIENTED_EDGE ( 'NONE', *, *, #734, .F. ) ;
#14587 = LINE ( 'NONE', #6835, #12079 ) ;
#14588 = DIRECTION ( 'NONE',  ( 1.734723475976806848E-16, 0.000000000000000000, 1.000000000000000000 ) ) ;
#14589 = CARTESIAN_POINT ( 'NONE',  ( 1.387661672111481170, 6.692913385826772199, -1.663104731517922596 ) ) ;
#14590 = DIRECTION ( 'NONE',  ( 1.734723475976806848E-16, -0.000000000000000000, 1.000000000000000000 ) ) ;
#14591 = DIRECTION ( 'NONE',  ( 0.000000000000000000, 0.000000000000000000, -1.000000000000000000 ) ) ;
#14592 = AXIS2_PLACEMENT_3D ( 'NONE', #35347, #46173, #30963 ) ;
#14593 = VERTEX_POINT ( 'NONE', #14327 ) ;
#14594 = CARTESIAN_POINT ( 'NONE',  ( -0.3486774197067342151, 3.346456692913386100, -2.204724409448810540 ) ) ;
#14595 = DIRECTION ( 'NONE',  ( 1.734723475976806848E-16, -0.000000000000000000, 1.000000000000000000 ) ) ;
#14596 = ORIENTED_EDGE ( 'NONE', *, *, #37594, .T. ) ;
#14597 = FACE_OUTER_BOUND ( 'NONE', #13620, .T. ) ;
#14598 = DIRECTION ( 'NONE',  ( 1.734723475976806848E-16, -0.000000000000000000, 1.000000000000000000 ) ) ;
#14599 = VERTEX_POINT ( 'NONE', #48065 ) ;
#14600 = DIRECTION ( 'NONE',  ( 0.000000000000000000, -1.000000000000000000, 0.000000000000000000 ) ) ;
#14601 = VECTOR ( 'NONE', #16868, 39.37007874015748143 ) ;
#14602 = CARTESIAN_POINT ( 'NONE',  ( 1.015142113812069091, 3.346456692913386100, -1.417322834645664331 ) ) ;
#14603 = CARTESIAN_POINT ( 'NONE',  ( -0.2727639067037607168, 3.267716535433071279, 4.731699523581612206E-17 ) ) ;
#14604 = ADVANCED_FACE ( 'NONE', ( #31860 ), #8863, .F. ) ;
#14605 = ADVANCED_FACE ( 'NONE', ( #8353 ), #40110, .F. ) ;
#14606 = ORIENTED_EDGE ( 'NONE', *, *, #321, .F. ) ;
#14607 = DIRECTION ( 'NONE',  ( -3.469446951953613696E-16, 0.000000000000000000, -1.000000000000000000 ) ) ;
#14608 = VERTEX_POINT ( 'NONE', #8096 ) ;
#14609 = FACE_BOUND ( 'NONE', #8720, .T. ) ;
#14610 = EDGE_CURVE ( 'NONE', #1329, #50585, #19453, .T. ) ;
#14611 = DIRECTION ( 'NONE',  ( -0.000000000000000000, 1.000000000000000000, -0.000000000000000000 ) ) ;
#14612 = PRODUCT_DEFINITION ( 'UNKNOWN', '', #15210, #1942 ) ;
#14613 = CARTESIAN_POINT ( 'NONE',  ( 1.560669927219590747, 3.346456692913386100, -0.1574803149606304187 ) ) ;
#14615 = ADVANCED_FACE ( 'NONE', ( #35982 ), #16359, .F. ) ;
#14614 = DIRECTION ( 'NONE',  ( -0.000000000000000000, 1.000000000000000000, -0.000000000000000000 ) ) ;
#14616 = EDGE_CURVE ( 'NONE', #4005, #46097, #36241, .T. ) ;
#14617 = ORIENTED_EDGE ( 'NONE', *, *, #16338, .T. ) ;
#14618 = EDGE_LOOP ( 'NONE', ( #25964, #16737, #39308, #46887 ) ) ;
#14619 = FACE_OUTER_BOUND ( 'NONE', #50357, .T. ) ;
#14620 = CARTESIAN_POINT ( 'NONE',  ( 0.1968503937007872184, 3.267716535433071279, -6.829619984160650651E-17 ) ) ;
#14621 = DIRECTION ( 'NONE',  ( 1.000000000000000000, 0.000000000000000000, 0.000000000000000000 ) ) ;
#14622 = DIRECTION ( 'NONE',  ( 1.000000000000000000, 0.000000000000000000, 0.000000000000000000 ) ) ;
#14623 = DIRECTION ( 'NONE',  ( 0.000000000000000000, 0.000000000000000000, -1.000000000000000000 ) ) ;
#14624 = ORIENTED_EDGE ( 'NONE', *, *, #34662, .F. ) ;
#14625 = EDGE_CURVE ( 'NONE', #30593, #3260, #19709, .T. ) ;
#14626 = ORIENTED_EDGE ( 'NONE', *, *, #36635, .F. ) ;
#14627 = FACE_OUTER_BOUND ( 'NONE', #1191, .T. ) ;
#14628 = VECTOR ( 'NONE', #17864, 39.37007874015748143 ) ;
#14629 = VECTOR ( 'NONE', #3221, 39.37007874015748143 ) ;
#14630 = FACE_OUTER_BOUND ( 'NONE', #2453, .T. ) ;
#14631 = VECTOR ( 'NONE', #12298, 39.37007874015748143 ) ;
#14632 = VERTEX_POINT ( 'NONE', #11715 ) ;
#14633 = ADVANCED_FACE ( 'NONE', ( #12474 ), #12737, .F. ) ;
#14634 = DIRECTION ( 'NONE',  ( -3.469446951953613696E-16, 0.000000000000000000, -1.000000000000000000 ) ) ;
#14635 = ORIENTED_EDGE ( 'NONE', *, *, #3413, .T. ) ;
#14636 = ORIENTED_EDGE ( 'NONE', *, *, #2186, .T. ) ;
#14637 = EDGE_CURVE ( 'NONE', #41415, #14810, #28217, .T. ) ;
#14638 = ORIENTED_EDGE ( 'NONE', *, *, #19979, .F. ) ;
#14639 = ORIENTED_EDGE ( 'NONE', *, *, #20400, .F. ) ;
#14640 = CARTESIAN_POINT ( 'NONE',  ( 0.1968503937007872462, 3.346456692913386100, -0.8267716535433052849 ) ) ;
#14642 = LINE ( 'NONE', #34766, #19621 ) ;
#14641 = VECTOR ( 'NONE', #16877, 39.37007874015748143 ) ;
#14643 = ADVANCED_FACE ( 'NONE', ( #31345 ), #8606, .F. ) ;
#14644 = CARTESIAN_POINT ( 'NONE',  ( 1.033659310791692709, 1.691649499786236133, -2.032992207565942788 ) ) ;
#14645 = CARTESIAN_POINT ( 'NONE',  ( -0.5455278134075214336, 3.346456692913386100, -1.771653543307081025 ) ) ;
#14646 = CARTESIAN_POINT ( 'NONE',  ( 0.08139965876239094178, 1.610780518492231694, 0.000000000000000000 ) ) ;
#14647 = CARTESIAN_POINT ( 'NONE',  ( -0.2430652128771645382, 1.574803149606302854, -2.151668812760861194 ) ) ;
#14648 = ORIENTED_EDGE ( 'NONE', *, *, #4478, .F. ) ;
#14649 = CARTESIAN_POINT ( 'NONE',  ( 1.244991204790707684, 3.267716535433071279, -1.771653543307081691 ) ) ;
#14650 = CARTESIAN_POINT ( 'NONE',  ( -0.8942052331142547050, 3.346456692913386100, 0.1181102362204705658 ) ) ;
#14651 = CARTESIAN_POINT ( 'NONE',  ( 1.909347346926324684, 3.267716535433071279, 1.021348170950612033 ) ) ;
#14652 = DIRECTION ( 'NONE',  ( 1.000000000000000000, 0.000000000000000000, 0.000000000000000000 ) ) ;
#14653 = EDGE_LOOP ( 'NONE', ( #10990, #2213, #33941, #10970 ) ) ;
#14654 = CARTESIAN_POINT ( 'NONE',  ( -1.863748091109392879, 3.346456692913386100, 1.102362204724404160 ) ) ;
#14655 = LINE ( 'NONE', #46122, #9613 ) ;
#14656 = VERTEX_POINT ( 'NONE', #32369 ) ;
#14657 = DIRECTION ( 'NONE',  ( -0.000000000000000000, 1.000000000000000000, -0.000000000000000000 ) ) ;
#14658 = VECTOR ( 'NONE', #33922, 39.37007874015748143 ) ;
#14659 = AXIS2_PLACEMENT_3D ( 'NONE', #24048, #812, #12687 ) ;
#14660 = CARTESIAN_POINT ( 'NONE',  ( -2.164823134740036181, 1.673236549936605977, -0.04796011690018290446 ) ) ;
#14661 = ORIENTED_EDGE ( 'NONE', *, *, #17015, .T. ) ;
#14662 = AXIS2_PLACEMENT_3D ( 'NONE', #22750, #50312, #18630 ) ;
#14663 = CARTESIAN_POINT ( 'NONE',  ( -0.5455278134075214336, 3.346456692913386100, -0.3149606299212593941 ) ) ;
#14664 = ORIENTED_EDGE ( 'NONE', *, *, #50333, .F. ) ;
#14665 = CARTESIAN_POINT ( 'NONE',  ( 0.2727639067037604392, 3.346456692913386100, -0.9842519685039348154 ) ) ;
#14666 = EDGE_CURVE ( 'NONE', #47601, #35447, #20217, .T. ) ;
#14667 = FACE_OUTER_BOUND ( 'NONE', #46738, .T. ) ;
#14668 = DIRECTION ( 'NONE',  ( -0.9998717552508121775, -0.01601477604151182663, 0.000000000000000000 ) ) ;
#14669 = CARTESIAN_POINT ( 'NONE',  ( -2.044241703397525978, 6.692913385826772199, -0.7159595814952903758 ) ) ;
#14671 = EDGE_CURVE ( 'NONE', #33352, #28267, #9618, .T. ) ;
#14670 = CARTESIAN_POINT ( 'NONE',  ( -2.102985103392958077, 3.267716535433071279, 0.1181102362204704270 ) ) ;
#14672 = ORIENTED_EDGE ( 'NONE', *, *, #19890, .T. ) ;
#14673 = EDGE_CURVE ( 'NONE', #37048, #32813, #20480, .T. ) ;
#14674 = AXIS2_PLACEMENT_3D ( 'NONE', #15200, #19064, #38207 ) ;
#14675 = DIRECTION ( 'NONE',  ( -3.469446951953613696E-16, 0.000000000000000000, -1.000000000000000000 ) ) ;
#14676 = EDGE_LOOP ( 'NONE', ( #38856, #3927, #7772, #50010 ) ) ;
#14677 = ORIENTED_EDGE ( 'NONE', *, *, #39482, .F. ) ;
#14678 = LINE ( 'NONE', #42789, #7283 ) ;
#14679 = ORIENTED_EDGE ( 'NONE', *, *, #20661, .F. ) ;
#14680 = LINE ( 'NONE', #18046, #2357 ) ;
#14681 = CARTESIAN_POINT ( 'NONE',  ( -1.363819533518803029, 3.346456692913386100, 1.417322834645662777 ) ) ;
#14682 = ORIENTED_EDGE ( 'NONE', *, *, #6333, .F. ) ;
#14683 = DIRECTION ( 'NONE',  ( -1.729310098865080642E-17, 1.000000000000000000, 1.276627980444840260E-16 ) ) ;
#14684 = DIRECTION ( 'NONE',  ( 1.734723475976806848E-16, -0.000000000000000000, 1.000000000000000000 ) ) ;
#14685 = B_SPLINE_CURVE_WITH_KNOTS ( 'NONE', 3,
 ( #12959, #28693, #44439, #24829 ),
 .UNSPECIFIED., .F., .F.,
 ( 4, 4 ),
 ( 0.001075175214026108947, 0.04744591858952573737 ),
 .UNSPECIFIED. ) ;
#14686 = CARTESIAN_POINT ( 'NONE',  ( 0.5544985201248122664, 1.716783259433079856, -2.194164409418295048 ) ) ;
#14687 = ORIENTED_EDGE ( 'NONE', *, *, #41350, .F. ) ;
#14688 = EDGE_LOOP ( 'NONE', ( #450, #20563, #26091, #5981 ) ) ;
#14689 = DIRECTION ( 'NONE',  ( 0.5407162030609374836, -0.6444004775717706579, -0.5407162030609372616 ) ) ;
#14690 = FACE_BOUND ( 'NONE', #31553, .T. ) ;
#14691 = ORIENTED_EDGE ( 'NONE', *, *, #14472, .T. ) ;
#14692 = CARTESIAN_POINT ( 'NONE',  ( -1.363819533518803473, 3.232777166330603524, 2.047244094488179567 ) ) ;
#14693 = FACE_OUTER_BOUND ( 'NONE', #18711, .T. ) ;
#14694 = AXIS2_PLACEMENT_3D ( 'NONE', #45629, #13661, #36198 ) ;
#14695 = EDGE_CURVE ( 'NONE', #15287, #24457, #346, .T. ) ;
#14696 = ORIENTED_EDGE ( 'NONE', *, *, #18500, .F. ) ;
#14697 = VERTEX_POINT ( 'NONE', #7844 ) ;
#14698 = CARTESIAN_POINT ( 'NONE',  ( -2.139038182717881487, 1.575216142802386754, 0.3394144611327329364 ) ) ;
#14699 = DIRECTION ( 'NONE',  ( 0.000000000000000000, 0.000000000000000000, 1.000000000000000000 ) ) ;
#14700 = ORIENTED_EDGE ( 'NONE', *, *, #39564, .F. ) ;
#14701 = AXIS2_PLACEMENT_3D ( 'NONE', #28588, #24217, #31968 ) ;
#14702 = EDGE_CURVE ( 'NONE', #19859, #9471, #49004, .T. ) ;
#14703 = EDGE_LOOP ( 'NONE', ( #21673, #2859, #33837, #13050 ) ) ;
#14704 = DIRECTION ( 'NONE',  ( -3.469446951953613696E-16, 0.000000000000000000, -1.000000000000000000 ) ) ;
#14705 = DIRECTION ( 'NONE',  ( -1.000000000000000000, 0.000000000000000000, -0.000000000000000000 ) ) ;
#14706 = VECTOR ( 'NONE', #11670, 39.37007874015748143 ) ;
#14707 = EDGE_CURVE ( 'NONE', #8950, #50349, #15837, .T. ) ;
#14708 = DIRECTION ( 'NONE',  ( -0.01601477604151182663, 0.9998717552508123996, -0.000000000000000000 ) ) ;
#14709 = AXIS2_PLACEMENT_3D ( 'NONE', #19567, #23706, #3079 ) ;
#14710 = ORIENTED_EDGE ( 'NONE', *, *, #32560, .T. ) ;
#14711 = ORIENTED_EDGE ( 'NONE', *, *, #24846, .T. ) ;
#14712 = CARTESIAN_POINT ( 'NONE',  ( -1.363819533518803473, 3.346456692913386100, -0.7874015748031470974 ) ) ;
#14713 = FACE_OUTER_BOUND ( 'NONE', #17149, .T. ) ;
#14714 = CARTESIAN_POINT ( 'NONE',  ( 1.091055626815042645, 3.346456692913386100, 1.259842519685033357 ) ) ;
#14715 = EDGE_CURVE ( 'NONE', #37228, #16522, #16099, .T. ) ;
#14716 = CARTESIAN_POINT ( 'NONE',  ( -1.930190994932096782, 5.905511811023623991, -0.9827944786818715306 ) ) ;
#14717 = ADVANCED_FACE ( 'NONE', ( #20993 ), #44719, .F. ) ;
#14718 = CARTESIAN_POINT ( 'NONE',  ( 1.560669927219590747, 0.000000000000000000, -0.4724409448818889246 ) ) ;
#14719 = CARTESIAN_POINT ( 'NONE',  ( -2.442519317017155078, 3.215267933203563189, -0.3543307086614173040 ) ) ;
#14720 = LINE ( 'NONE', #49784, #50569 ) ;
#14721 = ORIENTED_EDGE ( 'NONE', *, *, #24228, .T. ) ;
#14722 = PLANE ( 'NONE',  #48937 ) ;
#14723 = LINE ( 'NONE', #30475, #16208 ) ;
#14724 = ORIENTED_EDGE ( 'NONE', *, *, #15920, .F. ) ;
#14726 = EDGE_CURVE ( 'NONE', #43424, #27061, #9375, .T. ) ;
#14725 = ORIENTED_EDGE ( 'NONE', *, *, #23803, .F. ) ;
#14727 = DIRECTION ( 'NONE',  ( -0.000000000000000000, 1.000000000000000000, 0.000000000000000000 ) ) ;
#14728 = LINE ( 'NONE', #46191, #41055 ) ;
#14729 = VECTOR ( 'NONE', #46519, 39.37007874015748854 ) ;
#14730 = ORIENTED_EDGE ( 'NONE', *, *, #18150, .T. ) ;
#14731 = EDGE_CURVE ( 'NONE', #24457, #36095, #28255, .T. ) ;
#14732 = B_SPLINE_CURVE_WITH_KNOTS ( 'NONE', 3,
 ( #10875, #34125, #50073, #2626 ),
 .UNSPECIFIED., .F., .F.,
 ( 4, 4 ),
 ( 0.003451782018764085365, 0.004188683298192677484 ),
 .UNSPECIFIED. ) ;
#14733 = EDGE_CURVE ( 'NONE', #13031, #4521, #24867, .T. ) ;
#14734 = EDGE_LOOP ( 'NONE', ( #24219, #32316, #43662, #30331 ) ) ;
#14735 = LINE ( 'NONE', #3362, #36149 ) ;
#14736 = VECTOR ( 'NONE', #28111, 39.37007874015748143 ) ;
#14737 = EDGE_LOOP ( 'NONE', ( #43271, #46879, #49735, #4580 ) ) ;
#14738 = VECTOR ( 'NONE', #1605, 39.37007874015748143 ) ;
#14739 = AXIS2_PLACEMENT_3D ( 'NONE', #44751, #45504, #32919 ) ;
#14740 = CARTESIAN_POINT ( 'NONE',  ( 2.309000164489917406, 1.744884814208895296, 0.2631132722234555410 ) ) ;
#14741 = FACE_OUTER_BOUND ( 'NONE', #50918, .T. ) ;
#14742 = ADVANCED_FACE ( 'NONE', ( #1877 ), #25372, .F. ) ;
#14743 = AXIS2_PLACEMENT_3D ( 'NONE', #42630, #47221, #47737 ) ;
#14744 = ORIENTED_EDGE ( 'NONE', *, *, #38437, .F. ) ;
#14745 = CARTESIAN_POINT ( 'NONE',  ( 2.250827373609354254, 1.648918614562027152, 1.155336271601963505 ) ) ;
#14746 = EDGE_LOOP ( 'NONE', ( #10586, #27132, #31342, #31987 ) ) ;
#14747 = ORIENTED_EDGE ( 'NONE', *, *, #27416, .F. ) ;
#14748 = DIRECTION ( 'NONE',  ( -0.5407162030609373726, -0.6444004775717705469, -0.5407162030609375947 ) ) ;
#14749 = DIRECTION ( 'NONE',  ( 0.000000000000000000, 0.000000000000000000, -1.000000000000000000 ) ) ;
#14750 = CARTESIAN_POINT ( 'NONE',  ( 0.8182917201112824834, 3.346456692913386100, 2.004783788421103718 ) ) ;
#14751 = DIRECTION ( 'NONE',  ( 0.000000000000000000, 0.000000000000000000, 1.000000000000000000 ) ) ;
#14752 = VECTOR ( 'NONE', #13082, 39.37007874015748143 ) ;
#14753 = ORIENTED_EDGE ( 'NONE', *, *, #833, .F. ) ;
#14754 = DIRECTION ( 'NONE',  ( 1.734723475976806848E-16, -0.000000000000000000, 1.000000000000000000 ) ) ;
#14755 = CARTESIAN_POINT ( 'NONE',  ( 0.2727639067037604947, 0.000000000000000000, -1.102362204724405714 ) ) ;
#14756 = DIRECTION ( 'NONE',  ( -0.3930250316539278810, 1.288287287306305776E-16, 0.9195277725514489076 ) ) ;
#14757 = ADVANCED_FACE ( 'NONE', ( #49334 ), #2699, .T. ) ;
#14758 = ORIENTED_EDGE ( 'NONE', *, *, #27839, .F. ) ;
#14759 = DIRECTION ( 'NONE',  ( -0.9998717552508122886, -0.01601477604151182316, 0.000000000000000000 ) ) ;
#14760 = ORIENTED_EDGE ( 'NONE', *, *, #18500, .T. ) ;
#14761 = EDGE_LOOP ( 'NONE', ( #23533, #1999, #27525, #12803 ) ) ;
#14762 = CARTESIAN_POINT ( 'NONE',  ( 0.3960295651987776888, 1.619527252206727441, 2.457915758890707458 ) ) ;
#14763 = EDGE_CURVE ( 'NONE', #24410, #12066, #9116, .T. ) ;
#14764 = AXIS2_PLACEMENT_3D ( 'NONE', #33617, #49306, #25850 ) ;
#14765 = EDGE_CURVE ( 'NONE', #16395, #37702, #5241, .T. ) ;
#14766 = CARTESIAN_POINT ( 'NONE',  ( -1.977237857982436342, 1.610616070542161049, -0.8986314441088352201 ) ) ;
#14767 = LINE ( 'NONE', #11394, #802 ) ;
#14768 = ORIENTED_EDGE ( 'NONE', *, *, #10302, .T. ) ;
#14770 = EDGE_CURVE ( 'NONE', #21615, #7243, #40871, .T. ) ;
#14769 = EDGE_LOOP ( 'NONE', ( #2155, #33112, #45761, #33848 ) ) ;
#14771 = LINE ( 'NONE', #9696, #10615 ) ;
#14772 = CARTESIAN_POINT ( 'NONE',  ( -0.7328193673159020260, 1.696164507524817511, 2.092647490920610309 ) ) ;
#14773 = VERTEX_POINT ( 'NONE', #5756 ) ;
#14774 = CARTESIAN_POINT ( 'NONE',  ( -1.695772546416001836, 1.692832103184166437, -2.417756147381374010 ) ) ;
#14775 = LINE ( 'NONE', #10649, #37488 ) ;
#14776 = VECTOR ( 'NONE', #3969, 39.37007874015748143 ) ;
#14777 = VECTOR ( 'NONE', #35740, 39.37007874015748143 ) ;
#14778 = LINE ( 'NONE', #23026, #23355 ) ;
#14779 = PLANE ( 'NONE',  #45008 ) ;
#14780 = DIRECTION ( 'NONE',  ( -1.000000000000000000, 0.000000000000000000, -0.000000000000000000 ) ) ;
#14781 = ORIENTED_EDGE ( 'NONE', *, *, #5811, .F. ) ;
#14782 = DIRECTION ( 'NONE',  ( 1.734723475976806848E-16, 0.000000000000000000, 1.000000000000000000 ) ) ;
#14783 = FACE_OUTER_BOUND ( 'NONE', #9713, .T. ) ;
#14784 = EDGE_CURVE ( 'NONE', #20320, #18496, #33136, .T. ) ;
#14785 = VECTOR ( 'NONE', #38604, 39.37007874015748143 ) ;
#14786 = DIRECTION ( 'NONE',  ( 1.734723475976806848E-16, -0.000000000000000000, 1.000000000000000000 ) ) ;
#14787 = ORIENTED_EDGE ( 'NONE', *, *, #26645, .T. ) ;
#14788 = CARTESIAN_POINT ( 'NONE',  ( -0.8182917201112819283, 3.346456692913386100, -2.047244094488181343 ) ) ;
#14789 = EDGE_CURVE ( 'NONE', #27908, #7564, #13761, .T. ) ;
#14790 = LINE ( 'NONE', #34663, #35260 ) ;
#14791 = LINE ( 'NONE', #42147, #6582 ) ;
#14792 = VERTEX_POINT ( 'NONE', #32891 ) ;
#14793 = EDGE_CURVE ( 'NONE', #36721, #43798, #48574, .T. ) ;
#14794 = DIRECTION ( 'NONE',  ( 0.000000000000000000, 0.000000000000000000, -1.000000000000000000 ) ) ;
#14795 = EDGE_CURVE ( 'NONE', #30476, #15256, #29504, .T. ) ;
#14796 = EDGE_CURVE ( 'NONE', #12747, #12590, #21503, .T. ) ;
#14797 = VERTEX_POINT ( 'NONE', #41379 ) ;
#14798 = CARTESIAN_POINT ( 'NONE',  ( 0.000000000000000000, 1.574803149606302854, 0.000000000000000000 ) ) ;
#14799 = ORIENTED_EDGE ( 'NONE', *, *, #37536, .T. ) ;
#14800 = CARTESIAN_POINT ( 'NONE',  ( 2.106197740627112402, 0.000000000000000000, 0.7874015748031456541 ) ) ;
#14801 = PLANE ( 'NONE',  #25181 ) ;
#14802 = DIRECTION ( 'NONE',  ( -1.000000000000000000, 0.000000000000000000, -0.000000000000000000 ) ) ;
#14803 = LINE ( 'NONE', #34923, #10364 ) ;
#14804 = CIRCLE ( 'NONE', #26368, 3.033577403570481668 ) ;
#14805 = ORIENTED_EDGE ( 'NONE', *, *, #25225, .F. ) ;
#14806 = VERTEX_POINT ( 'NONE', #20733 ) ;
#14807 = VERTEX_POINT ( 'NONE', #36492 ) ;
#14808 = LINE ( 'NONE', #14553, #48781 ) ;
#14809 = LINE ( 'NONE', #18426, #42000 ) ;
#14810 = VERTEX_POINT ( 'NONE', #6005 ) ;
#14811 = CARTESIAN_POINT ( 'NONE',  ( -2.182111253630085290, 0.000000000000000000, -0.5118110236220464460 ) ) ;
#14812 = CARTESIAN_POINT ( 'NONE',  ( -1.843283979527560623, 1.678378384481335139, -1.157773721536293765 ) ) ;
#14813 = FACE_OUTER_BOUND ( 'NONE', #25410, .T. ) ;
#14814 = VECTOR ( 'NONE', #32044, 39.37007874015748143 ) ;
#14815 = ORIENTED_EDGE ( 'NONE', *, *, #45704, .F. ) ;
#14816 = ORIENTED_EDGE ( 'NONE', *, *, #50750, .T. ) ;
#14817 = CARTESIAN_POINT ( 'NONE',  ( 1.909347346926324462, 0.000000000000000000, -0.7874015748031473194 ) ) ;
#14818 = LINE ( 'NONE', #22559, #42293 ) ;
#14819 = FACE_OUTER_BOUND ( 'NONE', #13387, .T. ) ;
#14820 = ORIENTED_EDGE ( 'NONE', *, *, #527, .T. ) ;
#14821 =( LENGTH_UNIT ( ) NAMED_UNIT ( * ) SI_UNIT ( $, .METRE. ) );
#14822 = FACE_BOUND ( 'NONE', #41696, .T. ) ;
#14823 = ORIENTED_EDGE ( 'NONE', *, *, #20683, .T. ) ;
#14824 = CARTESIAN_POINT ( 'NONE',  ( 2.949046705395496737, 1.666728343919011035, -0.1488625692557980496 ) ) ;
#14825 = ORIENTED_EDGE ( 'NONE', *, *, #21126, .T. ) ;
#14826 = ORIENTED_EDGE ( 'NONE', *, *, #2114, .F. ) ;
#14827 = AXIS2_PLACEMENT_3D ( 'NONE', #4175, #35495, #16388 ) ;
#14828 = LINE ( 'NONE', #2952, #18827 ) ;
#14829 = CARTESIAN_POINT ( 'NONE',  ( 0.07982360342473591996, 1.709180471932028711, 0.000000000000000000 ) ) ;
#14830 = CARTESIAN_POINT ( 'NONE',  ( -1.722324667924217456, 1.550974602593178764, -2.398464901896889767 ) ) ;
#14831 = EDGE_CURVE ( 'NONE', #13249, #20960, #45474, .T. ) ;
#14832 = DIRECTION ( 'NONE',  ( -0.000000000000000000, 1.000000000000000000, -0.000000000000000000 ) ) ;
#14833 = DIRECTION ( 'NONE',  ( -0.9998717552508121775, -0.01601477604151182663, 0.000000000000000000 ) ) ;
#14834 = ORIENTED_EDGE ( 'NONE', *, *, #10399, .F. ) ;
#14835 = ADVANCED_FACE ( 'NONE', ( #24614 ), #40372, .F. ) ;
#14836 = EDGE_CURVE ( 'NONE', #1706, #33976, #13505, .T. ) ;
#14837 = ORIENTED_EDGE ( 'NONE', *, *, #23910, .T. ) ;
#14838 = DIRECTION ( 'NONE',  ( 1.734723475976806848E-16, -0.000000000000000000, 1.000000000000000000 ) ) ;
#14839 = EDGE_CURVE ( 'NONE', #10544, #27409, #11148, .T. ) ;
#14840 = CARTESIAN_POINT ( 'NONE',  ( 2.010517631316623088, 5.905511811023623991, 0.8058170502102370847 ) ) ;
#14841 = VECTOR ( 'NONE', #44270, 39.37007874015748143 ) ;
#14842 = FACE_OUTER_BOUND ( 'NONE', #21013, .T. ) ;
#14843 = DIRECTION ( 'NONE',  ( -1.000000000000000000, 0.000000000000000000, 1.734723475976806848E-16 ) ) ;
#14844 = CARTESIAN_POINT ( 'NONE',  ( -1.984304711380529218, 1.049866565067837820, -0.4024264094840596662 ) ) ;
#14845 = EDGE_LOOP ( 'NONE', ( #32338, #6709, #5389, #4754 ) ) ;
#14846 = LINE ( 'NONE', #22342, #13502 ) ;
#14847 = EDGE_CURVE ( 'NONE', #48407, #22473, #37365, .T. ) ;
#14848 = CARTESIAN_POINT ( 'NONE',  ( -0.8182917201112819283, 0.000000000000000000, -1.732283464566922726 ) ) ;
#14849 = VECTOR ( 'NONE', #42315, 39.37007874015748143 ) ;
#14850 = VERTEX_POINT ( 'NONE', #15274 ) ;
#14851 = DIRECTION ( 'NONE',  ( -0.000000000000000000, 1.000000000000000000, -0.000000000000000000 ) ) ;
#14852 = EDGE_CURVE ( 'NONE', #46686, #13400, #38527, .T. ) ;
#14853 = B_SPLINE_CURVE_WITH_KNOTS ( 'NONE', 3,
 ( #7433, #34051, #3302, #49736 ),
 .UNSPECIFIED., .F., .F.,
 ( 4, 4 ),
 ( 5.977740162239111428E-07, 0.0001168434444380691303 ),
 .UNSPECIFIED. ) ;
#14854 = CIRCLE ( 'NONE', #29706, 2.246510896728926010 ) ;
#14855 = LINE ( 'NONE', #15355, #21217 ) ;
#14856 = DIRECTION ( 'NONE',  ( -0.9749279121818259508, 0.000000000000000000, 0.2225209339563041788 ) ) ;
#14857 = DIRECTION ( 'NONE',  ( -0.9998717552508121775, -0.01601477604151182316, 0.000000000000000000 ) ) ;
#14858 = CARTESIAN_POINT ( 'NONE',  ( -0.8182917201112814842, 3.267716535433071279, 1.102362204724404160 ) ) ;
#14859 = CARTESIAN_POINT ( 'NONE',  ( -0.2727639067037608278, 0.000000000000000000, -1.614173228346451605 ) ) ;
#14860 = EDGE_CURVE ( 'NONE', #9111, #48211, #38279, .T. ) ;
#14861 = ORIENTED_EDGE ( 'NONE', *, *, #18290, .T. ) ;
#14862 = DIRECTION ( 'NONE',  ( -0.9998717552508122886, -0.01601477604151180928, 0.000000000000000000 ) ) ;
#14863 = AXIS2_PLACEMENT_3D ( 'NONE', #3430, #22541, #15301 ) ;
#14864 = ORIENTED_EDGE ( 'NONE', *, *, #24991, .F. ) ;
#14865 = FACE_BOUND ( 'NONE', #33242, .T. ) ;
#14866 = DIRECTION ( 'NONE',  ( -0.01601477604151182663, 0.9998717552508123996, -0.000000000000000000 ) ) ;
#14867 = DIRECTION ( 'NONE',  ( -0.8805955318567391110, 0.000000000000000000, 0.4738686624729965269 ) ) ;
#14868 = ORIENTED_EDGE ( 'NONE', *, *, #37414, .T. ) ;
#14869 = ORIENTED_EDGE ( 'NONE', *, *, #46733, .T. ) ;
#14870 = CARTESIAN_POINT ( 'NONE',  ( -1.909347346926324906, 0.000000000000000000, 1.417322834645662333 ) ) ;
#14871 = LINE ( 'NONE', #26733, #29589 ) ;
#14872 = CARTESIAN_POINT ( 'NONE',  ( -1.091055626815042645, 3.267716535433071279, -7.512581982576723358E-16 ) ) ;
#14873 = DIRECTION ( 'NONE',  ( -1.000000000000000000, 0.000000000000000000, 1.734723475976806848E-16 ) ) ;
#14874 = CARTESIAN_POINT ( 'NONE',  ( 0.8182917201112819283, 0.000000000000000000, -1.299212598425193210 ) ) ;
#14875 = LINE ( 'NONE', #12010, #37203 ) ;
#14876 = ORIENTED_EDGE ( 'NONE', *, *, #47497, .F. ) ;
#14877 = EDGE_LOOP ( 'NONE', ( #42436, #6671, #34879, #40150 ) ) ;
#14878 = DIRECTION ( 'NONE',  ( 1.000000000000000000, 0.000000000000000000, -3.469446951953613696E-16 ) ) ;
#14879 = LINE ( 'NONE', #26742, #19035 ) ;
#14880 = ORIENTED_EDGE ( 'NONE', *, *, #41255, .F. ) ;
#14881 = B_SPLINE_CURVE_WITH_KNOTS ( 'NONE', 3,
 ( #16684, #150, #32698, #15899 ),
 .UNSPECIFIED., .F., .F.,
 ( 4, 4 ),
 ( 0.0002245599449170471845, 0.002724693314481170959 ),
 .UNSPECIFIED. ) ;
#14882 = DIRECTION ( 'NONE',  ( -0.01601477604151182663, 0.9998717552508123996, -0.000000000000000000 ) ) ;
#14883 = ORIENTED_EDGE ( 'NONE', *, *, #19697, .F. ) ;
#14884 = ORIENTED_EDGE ( 'NONE', *, *, #28652, .T. ) ;
#14885 = AXIS2_PLACEMENT_3D ( 'NONE', #36048, #35789, #23652 ) ;
#14886 = VECTOR ( 'NONE', #17101, 39.37007874015748143 ) ;
#14887 = VERTEX_POINT ( 'NONE', #41886 ) ;
#14888 = ORIENTED_EDGE ( 'NONE', *, *, #32106, .T. ) ;
#14889 = CARTESIAN_POINT ( 'NONE',  ( -1.439733046521776583, 0.000000000000000000, -0.9448818897637762948 ) ) ;
#14890 = EDGE_CURVE ( 'NONE', #37147, #26914, #22018, .T. ) ;
#14891 = EDGE_CURVE ( 'NONE', #36899, #22341, #31023, .T. ) ;
#14892 = AXIS2_PLACEMENT_3D ( 'NONE', #14935, #13923, #22431 ) ;
#14893 = LINE ( 'NONE', #3520, #46006 ) ;
#14894 = LINE ( 'NONE', #10514, #8761 ) ;
#14895 = ADVANCED_FACE ( 'NONE', ( #2897 ), #42131, .T. ) ;
#14896 = EDGE_CURVE ( 'NONE', #22491, #7253, #22515, .T. ) ;
#14897 = DIRECTION ( 'NONE',  ( 1.734723475976806848E-16, -0.000000000000000000, 1.000000000000000000 ) ) ;
#14898 = B_SPLINE_CURVE_WITH_KNOTS ( 'NONE', 3,
 ( #36489, #44473, #1108, #9114 ),
 .UNSPECIFIED., .F., .F.,
 ( 4, 4 ),
 ( 0.01473299879128477791, 0.03075082650797690206 ),
 .UNSPECIFIED. ) ;
#14899 = CARTESIAN_POINT ( 'NONE',  ( 0.000000000000000000, 1.595182601976580683, 0.000000000000000000 ) ) ;
#14900 = CARTESIAN_POINT ( 'NONE',  ( 0.000000000000000000, 1.574803149606302854, 0.000000000000000000 ) ) ;
#14901 = ORIENTED_EDGE ( 'NONE', *, *, #10282, .T. ) ;
#14902 = DIRECTION ( 'NONE',  ( 1.000000000000000000, 0.000000000000000000, 0.000000000000000000 ) ) ;
#14903 = LINE ( 'NONE', #42515, #15949 ) ;
#14904 = DIRECTION ( 'NONE',  ( -0.000000000000000000, 1.000000000000000000, -0.000000000000000000 ) ) ;
#14905 = LINE ( 'NONE', #35036, #14141 ) ;
#14906 = ORIENTED_EDGE ( 'NONE', *, *, #38281, .F. ) ;
#14907 = DIRECTION ( 'NONE',  ( 1.734723475976806848E-16, -0.000000000000000000, 1.000000000000000000 ) ) ;
#14908 = EDGE_CURVE ( 'NONE', #15326, #18533, #42260, .T. ) ;
#14909 = CARTESIAN_POINT ( 'NONE',  ( 0.000000000000000000, 3.267716535433071279, -0.03937007874015881204 ) ) ;
#14910 = ORIENTED_EDGE ( 'NONE', *, *, #24504, .T. ) ;
#14911 = LINE ( 'NONE', #9772, #22162 ) ;
#14912 = CARTESIAN_POINT ( 'NONE',  ( -1.091055626815042645, 3.346456692913386100, -7.512581982576723358E-16 ) ) ;
#14913 = EDGE_CURVE ( 'NONE', #27463, #8395, #30523, .T. ) ;
#14914 = PRODUCT ( 'MAT-026', 'MAT-026', '', ( #11137 ) ) ;
#14915 = LINE ( 'NONE', #30919, #19957 ) ;
#14916 = VERTEX_POINT ( 'NONE', #6528 ) ;
#14917 = CARTESIAN_POINT ( 'NONE',  ( 1.306991306359274629, 1.630410611703223545, -1.882644677548868550 ) ) ;
#14918 = PLANE ( 'NONE',  #12669 ) ;
#14919 = AXIS2_PLACEMENT_3D ( 'NONE', #12879, #486, #16234 ) ;
#14920 = FACE_OUTER_BOUND ( 'NONE', #26394, .T. ) ;
#14921 = VECTOR ( 'NONE', #49942, 39.37007874015748143 ) ;
#14922 = LINE ( 'NONE', #11301, #9445 ) ;
#14923 = CARTESIAN_POINT ( 'NONE',  ( 0.000000000000000000, 3.267716535433071279, -0.9842519685039348154 ) ) ;
#14924 = VERTEX_POINT ( 'NONE', #18897 ) ;
#14925 = DIRECTION ( 'NONE',  ( 0.000000000000000000, 0.000000000000000000, -1.000000000000000000 ) ) ;
#14926 = ORIENTED_EDGE ( 'NONE', *, *, #36351, .F. ) ;
#14927 = ORIENTED_EDGE ( 'NONE', *, *, #3465, .F. ) ;
#14928 = CARTESIAN_POINT ( 'NONE',  ( -0.07591351300297277671, 3.346456692913386100, 1.102362204724404160 ) ) ;
#14929 = EDGE_LOOP ( 'NONE', ( #32627, #4088, #47404, #33522 ) ) ;
#14930 = CARTESIAN_POINT ( 'NONE',  ( -1.439733046521776583, 3.346456692913386100, -0.6299212598425177889 ) ) ;
#14931 = VECTOR ( 'NONE', #3759, 39.37007874015748143 ) ;
#14932 = DIRECTION ( 'NONE',  ( -1.000000000000000000, 0.000000000000000000, 0.000000000000000000 ) ) ;
#14933 = EDGE_CURVE ( 'NONE', #30628, #7819, #33229, .T. ) ;
#14934 = VERTEX_POINT ( 'NONE', #49579 ) ;
#14935 = CARTESIAN_POINT ( 'NONE',  ( -0.8182917201112814842, 0.000000000000000000, 1.102362204724404160 ) ) ;
#14936 = DIRECTION ( 'NONE',  ( -0.01601477604151182663, 0.9998717552508123996, -0.000000000000000000 ) ) ;
#14937 = DIRECTION ( 'NONE',  ( -0.000000000000000000, 1.000000000000000000, -0.000000000000000000 ) ) ;
#14938 = VERTEX_POINT ( 'NONE', #25884 ) ;
#14939 = ORIENTED_EDGE ( 'NONE', *, *, #38469, .T. ) ;
#14940 = FACE_OUTER_BOUND ( 'NONE', #2600, .T. ) ;
#14941 = FACE_BOUND ( 'NONE', #1842, .T. ) ;
#14942 = ORIENTED_EDGE ( 'NONE', *, *, #31139, .F. ) ;
#14943 = PLANE ( 'NONE',  #40244 ) ;
#14944 = ORIENTED_EDGE ( 'NONE', *, *, #37836, .F. ) ;
#14945 = VERTEX_POINT ( 'NONE', #50331 ) ;
#14946 = CARTESIAN_POINT ( 'NONE',  ( 1.363819533518803695, 3.267716535433071279, 1.605145679676862835 ) ) ;
#14947 = ADVANCED_FACE ( 'NONE', ( #34898 ), #3536, .F. ) ;
#14948 = DIRECTION ( 'NONE',  ( -0.000000000000000000, 0.000000000000000000, 1.000000000000000000 ) ) ;
#14949 = ORIENTED_EDGE ( 'NONE', *, *, #18580, .T. ) ;
#14950 = VECTOR ( 'NONE', #39708, 39.37007874015748143 ) ;
#14951 = CARTESIAN_POINT ( 'NONE',  ( -1.091055626815042423, 3.267716535433071279, 1.892679809432644143E-16 ) ) ;
#14952 = VERTEX_POINT ( 'NONE', #30013 ) ;
#14953 = DIRECTION ( 'NONE',  ( 5.779879058770898378E-18, 1.000000000000000000, 1.286990067732318227E-16 ) ) ;
#14954 = EDGE_CURVE ( 'NONE', #7296, #21655, #30770, .T. ) ;
#14955 = VECTOR ( 'NONE', #50653, 39.37007874015748143 ) ;
#14956 = LINE ( 'NONE', #30707, #22554 ) ;
#14957 = MECHANICAL_DESIGN_GEOMETRIC_PRESENTATION_REPRESENTATION (  '', ( #8357 ), #16619 ) ;
#14958 = EDGE_CURVE ( 'NONE', #40779, #18488, #7281, .T. ) ;
#14959 = ADVANCED_FACE ( 'NONE', ( #45984 ), #38772, .F. ) ;
#14960 = DIRECTION ( 'NONE',  ( -1.000000000000000000, 0.000000000000000000, 1.734723475976806848E-16 ) ) ;
#14961 = ORIENTED_EDGE ( 'NONE', *, *, #32815, .T. ) ;
#14962 = ORIENTED_EDGE ( 'NONE', *, *, #42264, .T. ) ;
#14963 = VECTOR ( 'NONE', #27997, 39.37007874015748143 ) ;
#14964 = LINE ( 'NONE', #23452, #11271 ) ;
#14965 = LINE ( 'NONE', #19577, #31115 ) ;
#14966 = LINE ( 'NONE', #7226, #38200 ) ;
#14967 = AXIS2_PLACEMENT_3D ( 'NONE', #28383, #37432, #48482 ) ;
#14968 = LINE ( 'NONE', #26828, #34245 ) ;
#14969 = CARTESIAN_POINT ( 'NONE',  ( -2.165354330708661568, 1.574803149606301966, -1.520079223026944511E-17 ) ) ;
#14970 = VECTOR ( 'NONE', #45302, 39.37007874015748143 ) ;
#14971 = CARTESIAN_POINT ( 'NONE',  ( -2.417802884545332542, 3.267716535433071279, -0.3543307086614173040 ) ) ;
#14972 = EDGE_CURVE ( 'NONE', #39122, #9992, #18390, .T. ) ;
#14973 = LINE ( 'NONE', #6215, #14340 ) ;
#14974 = ORIENTED_EDGE ( 'NONE', *, *, #44435, .T. ) ;
#14975 = FACE_OUTER_BOUND ( 'NONE', #14182, .T. ) ;
#14976 = CARTESIAN_POINT ( 'NONE',  ( 1.015142113812069313, 3.267716535433071279, 0.9055118110236164419 ) ) ;
#14977 = EDGE_CURVE ( 'NONE', #5175, #29752, #10648, .T. ) ;
#14978 = ORIENTED_EDGE ( 'NONE', *, *, #14185, .T. ) ;
#14979 = ORIENTED_EDGE ( 'NONE', *, *, #16636, .T. ) ;
#14980 = LINE ( 'NONE', #25388, #39053 ) ;
#14981 = CARTESIAN_POINT ( 'NONE',  ( 0.7423782071083085965, 0.000000000000000000, -0.1968503937007880511 ) ) ;
#14982 = ORIENTED_EDGE ( 'NONE', *, *, #30582, .T. ) ;
#14983 = EDGE_CURVE ( 'NONE', #17597, #4354, #12614, .T. ) ;
#14984 = ORIENTED_EDGE ( 'NONE', *, *, #46387, .T. ) ;
#14985 = LINE ( 'NONE', #49794, #25426 ) ;
#14986 = ADVANCED_FACE ( 'NONE', ( #28347 ), #13421, .T. ) ;
#14987 = ORIENTED_EDGE ( 'NONE', *, *, #41702, .T. ) ;
#14988 = VECTOR ( 'NONE', #43709, 39.37007874015748143 ) ;
#14989 = LINE ( 'NONE', #6231, #38374 ) ;
#14990 = CARTESIAN_POINT ( 'NONE',  ( 0.1968503937007873017, 3.267716535433071279, 0.6299212598425161236 ) ) ;
#14991 = CONICAL_SURFACE ( 'NONE', #40568, 1.850107469027523210, 0.6386652850508578450 ) ;
#14992 = ORIENTED_EDGE ( 'NONE', *, *, #5162, .T. ) ;
#14993 = AXIS2_PLACEMENT_3D ( 'NONE', #577, #25285, #19920 ) ;
#14994 = LINE ( 'NONE', #19857, #37073 ) ;
#14995 = ORIENTED_EDGE ( 'NONE', *, *, #29777, .F. ) ;
#14996 = EDGE_LOOP ( 'NONE', ( #8829, #26218, #44949, #45114 ) ) ;
#14997 = ADVANCED_FACE ( 'NONE', ( #40750 ), #44096, .F. ) ;
#14998 = LINE ( 'NONE', #42851, #12827 ) ;
#15000 = PLANE ( 'NONE',  #6714 ) ;
#14999 = VECTOR ( 'NONE', #39448, 39.37007874015748143 ) ;
#15001 = CARTESIAN_POINT ( 'NONE',  ( 2.255357468390372322, 1.645600431408117847, -0.5652488166673508285 ) ) ;
#15002 = EDGE_CURVE ( 'NONE', #4018, #24951, #24491, .T. ) ;
#15003 = VECTOR ( 'NONE', #50590, 39.37007874015748143 ) ;
#15004 = ORIENTED_EDGE ( 'NONE', *, *, #50525, .F. ) ;
#15005 = CARTESIAN_POINT ( 'NONE',  ( -0.1184164328040565317, 2.755905511811024056, -0.3547750388873516791 ) ) ;
#15006 = DIRECTION ( 'NONE',  ( -0.000000000000000000, 1.000000000000000000, -0.000000000000000000 ) ) ;
#15007 = ORIENTED_EDGE ( 'NONE', *, *, #36607, .F. ) ;
#15008 = DIRECTION ( 'NONE',  ( -3.469446951953613696E-16, 0.000000000000000000, -1.000000000000000000 ) ) ;
#15009 = ORIENTED_EDGE ( 'NONE', *, *, #1463, .F. ) ;
#15010 = ORIENTED_EDGE ( 'NONE', *, *, #24499, .T. ) ;
#15011 = CARTESIAN_POINT ( 'NONE',  ( 0.2727639067037610499, 3.346456692913386100, 1.417322834645662777 ) ) ;
#15012 = EDGE_CURVE ( 'NONE', #28976, #17224, #38535, .T. ) ;
#15013 = DIRECTION ( 'NONE',  ( -0.000000000000000000, 1.000000000000000000, -0.000000000000000000 ) ) ;
#15014 = CARTESIAN_POINT ( 'NONE',  ( -2.047303704428026006, 1.642302236560388540, 0.7169544859399534786 ) ) ;
#15015 = ADVANCED_FACE ( 'NONE', ( #40241 ), #48443, .F. ) ;
#15016 = EDGE_CURVE ( 'NONE', #50839, #45040, #24745, .T. ) ;
#15017 = CARTESIAN_POINT ( 'NONE',  ( 0.5455278134075212115, 0.000000000000000000, -1.259842519685035134 ) ) ;
#15018 = ORIENTED_EDGE ( 'NONE', *, *, #9998, .F. ) ;
#15019 = ORIENTED_EDGE ( 'NONE', *, *, #1770, .F. ) ;
#15020 = DIRECTION ( 'NONE',  ( -1.000000000000000000, -0.000000000000000000, -0.000000000000000000 ) ) ;
#15021 = CARTESIAN_POINT ( 'NONE',  ( -0.7032328421997132706, 1.602112857160477688, -2.363122831868675444 ) ) ;
#15022 = ORIENTED_EDGE ( 'NONE', *, *, #1666, .T. ) ;
#15023 = CARTESIAN_POINT ( 'NONE',  ( 0.08119777152254364916, 1.623385212329073957, 0.000000000000000000 ) ) ;
#15024 = PLANE ( 'NONE',  #45735 ) ;
#15025 = CONICAL_SURFACE ( 'NONE', #48777, 1.850107469027523210, 0.6386652850508578450 ) ;
#15026 = CARTESIAN_POINT ( 'NONE',  ( -2.339241080213612545, 1.682800407567106360, 1.802537235681883843 ) ) ;
#15027 = CARTESIAN_POINT ( 'NONE',  ( 1.528548638478742783, 1.644611471120091872, 2.526375981328617737 ) ) ;
#15029 = DIRECTION ( 'NONE',  ( -0.000000000000000000, -1.000000000000000000, -0.000000000000000000 ) ) ;
#15028 = CIRCLE ( 'NONE', #42221, 2.106299212598425008 ) ;
#15030 = ORIENTED_EDGE ( 'NONE', *, *, #3676, .T. ) ;
#15031 = CARTESIAN_POINT ( 'NONE',  ( -0.7381027496704857249, 1.531192278308824539, -2.859439394060923068 ) ) ;
#15032 = CARTESIAN_POINT ( 'NONE',  ( 0.8182917201112819283, 3.267716535433071279, 0.9055118110236164419 ) ) ;
#15033 = CIRCLE ( 'NONE', #40575, 2.106299212598425008 ) ;
#15034 = CARTESIAN_POINT ( 'NONE',  ( -1.091055626815042201, 3.346456692913386100, 1.259842519685033357 ) ) ;
#15035 = ORIENTED_EDGE ( 'NONE', *, *, #23246, .F. ) ;
#15036 = VECTOR ( 'NONE', #48908, 39.37007874015748143 ) ;
#15037 = FACE_OUTER_BOUND ( 'NONE', #1275, .T. ) ;
#15038 = CARTESIAN_POINT ( 'NONE',  ( -1.091055626815042645, 3.346456692913386100, 1.801691980386209258 ) ) ;
#15039 = CARTESIAN_POINT ( 'NONE',  ( 1.287906020515830141, 3.267716535433071279, 0.6299212598425161236 ) ) ;
#15040 = EDGE_LOOP ( 'NONE', ( #39590, #21110, #47273, #11480 ) ) ;
#15041 = EDGE_CURVE ( 'NONE', #49607, #38635, #28862, .T. ) ;
#15042 = CARTESIAN_POINT ( 'NONE',  ( 0.4696143004045479352, 3.346456692913386100, 0.4724409448818868706 ) ) ;
#15043 = ORIENTED_EDGE ( 'NONE', *, *, #32645, .T. ) ;
#15044 = FACE_OUTER_BOUND ( 'NONE', #9451, .T. ) ;
#15045 = VERTEX_POINT ( 'NONE', #36367 ) ;
#15046 = PLANE ( 'NONE',  #47595 ) ;
#15047 = EDGE_CURVE ( 'NONE', #7771, #7991, #21131, .T. ) ;
#15048 = ORIENTED_EDGE ( 'NONE', *, *, #11561, .T. ) ;
#15049 = LINE ( 'NONE', #50605, #44133 ) ;
#15050 = CARTESIAN_POINT ( 'NONE',  ( -0.3486774197067334380, 3.267716535433071279, 0.6299212598425164567 ) ) ;
#15051 = LINE ( 'NONE', #32594, #28524 ) ;
#15052 = EDGE_CURVE ( 'NONE', #36717, #16462, #44349, .T. ) ;
#15053 = EDGE_CURVE ( 'NONE', #37182, #38821, #48371, .T. ) ;
#15054 = ORIENTED_EDGE ( 'NONE', *, *, #41257, .F. ) ;
#15055 = ORIENTED_EDGE ( 'NONE', *, *, #48701, .T. ) ;
#15056 = ORIENTED_EDGE ( 'NONE', *, *, #41949, .T. ) ;
#15057 = DIRECTION ( 'NONE',  ( -0.1342332658176522420, -1.160734090543305153E-16, -0.9909497617679352555 ) ) ;
#15058 = CARTESIAN_POINT ( 'NONE',  ( -0.4513972801127658641, 3.267716535433071279, -2.401574803149598036 ) ) ;
#15059 = ORIENTED_EDGE ( 'NONE', *, *, #36250, .T. ) ;
#15060 = CARTESIAN_POINT ( 'NONE',  ( 0.1067246931122726866, 0.02962905676920215767, 0.000000000000000000 ) ) ;
#15061 = CARTESIAN_POINT ( 'NONE',  ( 1.560669927219590303, 3.346456692913386100, -1.614173228346452715 ) ) ;
#15062 = DIRECTION ( 'NONE',  ( 0.000000000000000000, -1.000000000000000000, 0.000000000000000000 ) ) ;
#15063 = ORIENTED_EDGE ( 'NONE', *, *, #4398, .F. ) ;
#15064 = VERTEX_POINT ( 'NONE', #19382 ) ;
#15065 = CARTESIAN_POINT ( 'NONE',  ( -1.723687301221637380, 0.000000000000000000, -1.311649477509825745 ) ) ;
#15066 = PLANE ( 'NONE',  #10131 ) ;
#15067 = CARTESIAN_POINT ( 'NONE',  ( -0.7874015748031498729, 0.000000000000000000, -1.138269997360109921E-16 ) ) ;
#15068 = EDGE_CURVE ( 'NONE', #34446, #35684, #5119, .T. ) ;
#15069 = ORIENTED_EDGE ( 'NONE', *, *, #23770, .F. ) ;
#15070 = CARTESIAN_POINT ( 'NONE',  ( -2.708693778652362827, 1.677031621480801649, -1.175591149396500779 ) ) ;
#15071 = VECTOR ( 'NONE', #48673, 39.37007874015748143 ) ;
#15072 = DIRECTION ( 'NONE',  ( -0.000000000000000000, 1.000000000000000000, -0.000000000000000000 ) ) ;
#15073 = ORIENTED_EDGE ( 'NONE', *, *, #12623, .T. ) ;
#15074 = DIRECTION ( 'NONE',  ( -1.000000000000000000, 0.000000000000000000, 0.000000000000000000 ) ) ;
#15075 = ORIENTED_EDGE ( 'NONE', *, *, #39705, .F. ) ;
#15076 = AXIS2_PLACEMENT_3D ( 'NONE', #7578, #23315, #27439 ) ;
#15077 = VERTEX_POINT ( 'NONE', #1247 ) ;
#15078 = DIRECTION ( 'NONE',  ( 1.734723475976806848E-16, -0.000000000000000000, 1.000000000000000000 ) ) ;
#15079 = CARTESIAN_POINT ( 'NONE',  ( 1.871024688710137163, 0.05788755007212831316, 0.5561875852992870239 ) ) ;
#15080 = AXIS2_PLACEMENT_3D ( 'NONE', #17125, #17888, #45221 ) ;
#15081 = ADVANCED_FACE ( 'NONE', ( #17005 ), #32765, .F. ) ;
#15082 = VECTOR ( 'NONE', #30203, 39.37007874015748143 ) ;
#15083 = FACE_OUTER_BOUND ( 'NONE', #14219, .T. ) ;
#15084 = CARTESIAN_POINT ( 'NONE',  ( 0.1968503937007872462, 3.346456692913386100, 0.4330708661417287386 ) ) ;
#15085 = EDGE_CURVE ( 'NONE', #30042, #22568, #9250, .T. ) ;
#15086 = ADVANCED_FACE ( 'NONE', ( #50829 ), #23516, .F. ) ;
#15087 = LINE ( 'NONE', #83, #23024 ) ;
#15088 = ORIENTED_EDGE ( 'NONE', *, *, #32795, .T. ) ;
#15089 = AXIS2_PLACEMENT_3D ( 'NONE', #21836, #41207, #37590 ) ;
#15090 = EDGE_LOOP ( 'NONE', ( #36436, #32057, #12442, #49883 ) ) ;
#15091 = CARTESIAN_POINT ( 'NONE',  ( -1.091055626815042201, 3.346456692913386100, 0.7480314960629874665 ) ) ;
#15092 = CARTESIAN_POINT ( 'NONE',  ( 1.723687301221656032, 6.692913385826772199, -1.311649477509801320 ) ) ;
#15093 = CARTESIAN_POINT ( 'NONE',  ( 1.387241876633648729, 1.574803149606302854, 1.662624236931697475 ) ) ;
#15094 = CARTESIAN_POINT ( 'NONE',  ( -1.847133429833641927, 0.5249316475426858419, -0.3711179595972480261 ) ) ;
#15095 = EDGE_LOOP ( 'NONE', ( #6462, #48137, #48386, #21977, #27658 ) ) ;
#15096 = CARTESIAN_POINT ( 'NONE',  ( -0.5455278134075217666, 3.267716535433071279, 9.463399047163231808E-17 ) ) ;
#15097 = PLANE ( 'NONE',  #47893 ) ;
#15098 = EDGE_LOOP ( 'NONE', ( #10497, #32034, #41101, #7932 ) ) ;
#15099 = CARTESIAN_POINT ( 'NONE',  ( -0.07591351300297284610, 0.000000000000000000, 1.220472440944875281 ) ) ;
#15100 = CARTESIAN_POINT ( 'NONE',  ( 1.738729679588007171, 0.000000000000000000, -0.1273486421339826147 ) ) ;
#15101 = LINE ( 'NONE', #8113, #14785 ) ;
#15102 = CARTESIAN_POINT ( 'NONE',  ( 0.4696143004045478797, 0.000000000000000000, -0.03937007874015908959 ) ) ;
#15103 = PLANE ( 'NONE',  #45593 ) ;
#15104 = FACE_OUTER_BOUND ( 'NONE', #4789, .T. ) ;
#15105 = VECTOR ( 'NONE', #47530, 39.37007874015748143 ) ;
#15106 = ORIENTED_EDGE ( 'NONE', *, *, #25453, .F. ) ;
#15107 = LINE ( 'NONE', #34235, #13973 ) ;
#15108 = EDGE_LOOP ( 'NONE', ( #43546, #1220, #31061, #29800 ) ) ;
#15109 = CARTESIAN_POINT ( 'NONE',  ( 1.833433833923351353, 3.267716535433071279, 0.1181102362204701633 ) ) ;
#15110 = AXIS2_PLACEMENT_3D ( 'NONE', #5940, #21436, #33581 ) ;
#15111 = CONICAL_SURFACE ( 'NONE', #10139, 3.033577403570480779, 1.554780866114618743 ) ;
#15112 = DIRECTION ( 'NONE',  ( -0.000000000000000000, 1.000000000000000000, -0.000000000000000000 ) ) ;
#15113 = CARTESIAN_POINT ( 'NONE',  ( 1.363819533518803251, 3.267716535433071279, -2.365849761790805487E-16 ) ) ;
#15114 = EDGE_CURVE ( 'NONE', #25737, #40030, #1503, .T. ) ;
#15115 = EDGE_CURVE ( 'NONE', #1147, #1290, #31280, .T. ) ;
#15116 = VERTEX_POINT ( 'NONE', #41507 ) ;
#15117 = VERTEX_POINT ( 'NONE', #41263 ) ;
#15118 = CARTESIAN_POINT ( 'NONE',  ( -2.182111253630085290, 3.346456692913386100, -0.5118110236220464460 ) ) ;
#15119 = AXIS2_PLACEMENT_3D ( 'NONE', #49087, #17383, #21259 ) ;
#15120 = CARTESIAN_POINT ( 'NONE',  ( 0.000000000000000000, 3.346456692913386100, 0.000000000000000000 ) ) ;
#15121 = DIRECTION ( 'NONE',  ( 0.000000000000000000, 0.000000000000000000, 1.000000000000000000 ) ) ;
#15122 = DIRECTION ( 'NONE',  ( 0.000000000000000000, 0.000000000000000000, -1.000000000000000000 ) ) ;
#15123 = DIRECTION ( 'NONE',  ( 0.000000000000000000, -1.000000000000000000, 0.000000000000000000 ) ) ;
#15124 = EDGE_CURVE ( 'NONE', #47754, #30246, #6139, .T. ) ;
#15125 = DIRECTION ( 'NONE',  ( -0.5773502691896259531, 0.5773502691896245098, -0.5773502691896270633 ) ) ;
#15126 = VERTEX_POINT ( 'NONE', #9506 ) ;
#15127 = ORIENTED_EDGE ( 'NONE', *, *, #17932, .T. ) ;
#15128 = CARTESIAN_POINT ( 'NONE',  ( 0.7423782071083092626, 0.000000000000000000, 1.574803149606291974 ) ) ;
#15129 = CARTESIAN_POINT ( 'NONE',  ( -0.8182917201112814842, 3.346456692913386100, 1.732283464566921172 ) ) ;
#15130 = VERTEX_POINT ( 'NONE', #2523 ) ;
#15131 = CARTESIAN_POINT ( 'NONE',  ( -0.7303501086101937823, 6.692913385826772199, 2.086068174627930816 ) ) ;
#15132 = EDGE_LOOP ( 'NONE', ( #15856, #29459, #30793, #4086 ) ) ;
#15133 = VERTEX_POINT ( 'NONE', #5631 ) ;
#15134 = EDGE_CURVE ( 'NONE', #48433, #7184, #18139, .T. ) ;
#15135 = EDGE_CURVE ( 'NONE', #16989, #19095, #25254, .T. ) ;
#15136 = ORIENTED_EDGE ( 'NONE', *, *, #35823, .F. ) ;
#15137 = ORIENTED_EDGE ( 'NONE', *, *, #33572, .F. ) ;
#15138 = LINE ( 'NONE', #42003, #20289 ) ;
#15139 = EDGE_CURVE ( 'NONE', #42832, #47610, #21632, .T. ) ;
#15140 = VECTOR ( 'NONE', #36728, 39.37007874015748143 ) ;
#15141 = ADVANCED_FACE ( 'NONE', ( #49458 ), #29117, .F. ) ;
#15142 = CONICAL_SURFACE ( 'NONE', #13528, 2.165354330708661568, 0.2617993877991570129 ) ;
#15143 = FACE_OUTER_BOUND ( 'NONE', #35708, .T. ) ;
#15145 = ADVANCED_FACE ( 'NONE', ( #1750 ), #10264, .F. ) ;
#15144 = B_SPLINE_CURVE_WITH_KNOTS ( 'NONE', 3,
 ( #21961, #25568, #2587, #48767 ),
 .UNSPECIFIED., .F., .F.,
 ( 4, 4 ),
 ( 0.001281067059624506604, 0.003781316473414019635 ),
 .UNSPECIFIED. ) ;
#15146 = CARTESIAN_POINT ( 'NONE',  ( -2.823445274216743073, 1.573787237234608005, 0.8656477926280277124 ) ) ;
#15147 = CARTESIAN_POINT ( 'NONE',  ( -2.271515265785818194, 1.047404546102530754, 1.166468901101386901 ) ) ;
#15148 = AXIS2_PLACEMENT_3D ( 'NONE', #6271, #14015, #29761 ) ;
#15149 = PLANE ( 'NONE',  #30545 ) ;
#15150 = CARTESIAN_POINT ( 'NONE',  ( -4.268512490100411402E-16, 0.000000000000000000, -2.401574803149598480 ) ) ;
#15151 = CARTESIAN_POINT ( 'NONE',  ( 1.630393911741433000, 1.635590496292660179, -1.626902725537468619 ) ) ;
#15152 = AXIS2_PLACEMENT_3D ( 'NONE', #16041, #28157, #32058 ) ;
#15153 = ORIENTED_EDGE ( 'NONE', *, *, #9257, .F. ) ;
#15154 = DIRECTION ( 'NONE',  ( -1.000000000000000000, 0.000000000000000000, -0.000000000000000000 ) ) ;
#15155 = DIRECTION ( 'NONE',  ( -0.1342332658176667026, -0.000000000000000000, 0.9909497617679331460 ) ) ;
#15156 = CARTESIAN_POINT ( 'NONE',  ( 1.833433833923351353, 3.346456692913386100, 0.1181102362204701633 ) ) ;
#15157 = DIRECTION ( 'NONE',  ( 1.000000000000000000, -0.000000000000000000, -0.000000000000000000 ) ) ;
#15158 = VERTEX_POINT ( 'NONE', #6399 ) ;
#15159 = DIRECTION ( 'NONE',  ( -1.000000000000000000, 0.000000000000000000, 1.734723475976806848E-16 ) ) ;
#15160 = CARTESIAN_POINT ( 'NONE',  ( -0.5455278134075214336, 0.000000000000000000, -1.574803149606293529 ) ) ;
#15161 = EDGE_LOOP ( 'NONE', ( #19167, #16420, #43671, #15748 ) ) ;
#15162 = CARTESIAN_POINT ( 'NONE',  ( 0.08119777152254364916, 1.623385212329073957, 0.000000000000000000 ) ) ;
#15163 = CARTESIAN_POINT ( 'NONE',  ( 0.000000000000000000, 0.000000000000000000, 0.000000000000000000 ) ) ;
#15164 = FACE_OUTER_BOUND ( 'NONE', #38555, .T. ) ;
#15165 = VERTEX_POINT ( 'NONE', #22146 ) ;
#15166 = CARTESIAN_POINT ( 'NONE',  ( -0.6214413264104945434, 0.000000000000000000, -0.9842519685039342603 ) ) ;
#15167 = CARTESIAN_POINT ( 'NONE',  ( 0.000000000000000000, 6.692913385826772199, 0.000000000000000000 ) ) ;
#15168 = DIRECTION ( 'NONE',  ( -1.000000000000000000, -0.000000000000000000, -0.000000000000000000 ) ) ;
#15169 = DIRECTION ( 'NONE',  ( -1.000000000000000000, -0.000000000000000000, -0.000000000000000000 ) ) ;
#15170 = LINE ( 'NONE', #12835, #45716 ) ;
#15171 = EDGE_LOOP ( 'NONE', ( #24340, #7613, #14217, #36446 ) ) ;
#15172 = CIRCLE ( 'NONE', #5260, 2.164630168518208109 ) ;
#15173 = EDGE_CURVE ( 'NONE', #41147, #41613, #47075, .T. ) ;
#15174 = ORIENTED_EDGE ( 'NONE', *, *, #24575, .F. ) ;
#15175 = VERTEX_POINT ( 'NONE', #21386 ) ;
#15176 = AXIS2_PLACEMENT_3D ( 'NONE', #16426, #12034, #47619 ) ;
#15177 = EDGE_CURVE ( 'NONE', #20686, #15727, #45354, .T. ) ;
#15178 = DIRECTION ( 'NONE',  ( -0.000000000000000000, 1.000000000000000000, -0.000000000000000000 ) ) ;
#15179 = ORIENTED_EDGE ( 'NONE', *, *, #36290, .T. ) ;
#15180 = FACE_OUTER_BOUND ( 'NONE', #30778, .T. ) ;
#15181 = VECTOR ( 'NONE', #41223, 39.37007874015748143 ) ;
#15182 = PLANE ( 'NONE',  #36799 ) ;
#15183 = EDGE_LOOP ( 'NONE', ( #25334, #48440, #7080, #43407 ) ) ;
#15184 = EDGE_CURVE ( 'NONE', #24477, #7825, #37903, .T. ) ;
#15185 = AXIS2_PLACEMENT_3D ( 'NONE', #20235, #16381, #47826 ) ;
#15186 = VECTOR ( 'NONE', #43589, 39.37007874015748143 ) ;
#15187 = CARTESIAN_POINT ( 'NONE',  ( -2.277873973731454171, 5.905511811023623991, 1.879489153247634992 ) ) ;
#15188 = CARTESIAN_POINT ( 'NONE',  ( 0.000000000000000000, 3.267716535433071279, -0.1968503937007886062 ) ) ;
#15189 = VECTOR ( 'NONE', #44364, 39.37007874015748143 ) ;
#15190 = VERTEX_POINT ( 'NONE', #13636 ) ;
#15191 = ORIENTED_EDGE ( 'NONE', *, *, #29603, .T. ) ;
#15192 = CARTESIAN_POINT ( 'NONE',  ( 1.461782879395301160, 5.905511811023623991, -1.598346982901808211 ) ) ;
#15193 = FACE_BOUND ( 'NONE', #6475, .T. ) ;
#15194 = ORIENTED_EDGE ( 'NONE', *, *, #13576, .T. ) ;
#15195 = PLANE ( 'NONE',  #37748 ) ;
#15196 = EDGE_CURVE ( 'NONE', #15817, #8923, #30139, .T. ) ;
#15197 = VERTEX_POINT ( 'NONE', #25756 ) ;
#15198 = ORIENTED_EDGE ( 'NONE', *, *, #33400, .F. ) ;
#15199 = CARTESIAN_POINT ( 'NONE',  ( -0.5484938307913003186, 0.5249316475426858419, -1.802438616188773990 ) ) ;
#15200 = CARTESIAN_POINT ( 'NONE',  ( 1.780101451746606722, 1.205361022782829114E-17, 1.234002060668519585 ) ) ;
#15201 = EDGE_CURVE ( 'NONE', #13274, #22175, #17759, .T. ) ;
#15202 = ORIENTED_EDGE ( 'NONE', *, *, #14958, .F. ) ;
#15203 = DIRECTION ( 'NONE',  ( -0.000000000000000000, 1.000000000000000000, -0.000000000000000000 ) ) ;
#15204 = ORIENTED_EDGE ( 'NONE', *, *, #9528, .T. ) ;
#15205 = DIRECTION ( 'NONE',  ( 0.000000000000000000, 0.000000000000000000, 1.000000000000000000 ) ) ;
#15206 = DIRECTION ( 'NONE',  ( -0.9998717552508122886, -0.01601477604151181275, 0.000000000000000000 ) ) ;
#15207 = CARTESIAN_POINT ( 'NONE',  ( -1.780101451746625152, 5.905511811023623991, 1.234002060668494716 ) ) ;
#15208 = ORIENTED_EDGE ( 'NONE', *, *, #48197, .T. ) ;
#15209 = VERTEX_POINT ( 'NONE', #37649 ) ;
#15210 = PRODUCT_DEFINITION_FORMATION_WITH_SPECIFIED_SOURCE ( 'ANY', '', #43784, .NOT_KNOWN. ) ;
#15211 = PLANE ( 'NONE',  #14592 ) ;
#15212 = LINE ( 'NONE', #4107, #10512 ) ;
#15213 = VECTOR ( 'NONE', #26389, 39.37007874015748143 ) ;
#15214 = CARTESIAN_POINT ( 'NONE',  ( 0.8069532150559728390, 6.692913385826772199, -2.010061882867131722 ) ) ;
#15215 = VECTOR ( 'NONE', #29335, 39.37007874015748143 ) ;
#15216 = EDGE_CURVE ( 'NONE', #1801, #12300, #2266, .T. ) ;
#15217 = CARTESIAN_POINT ( 'NONE',  ( 0.2510238314733705400, 1.613497360050089036, -2.240096307734528835 ) ) ;
#15218 = AXIS2_PLACEMENT_3D ( 'NONE', #39426, #50984, #30419 ) ;
#15219 = FACE_OUTER_BOUND ( 'NONE', #49949, .T. ) ;
#15220 = CONICAL_SURFACE ( 'NONE', #12753, 2.246510896728926010, 0.01601546068027819014 ) ;
#15221 = CARTESIAN_POINT ( 'NONE',  ( 0.04921259842519689481, 1.205361022782829114E-17, -2.165433070866142007 ) ) ;
#15222 = DIRECTION ( 'NONE',  ( -0.9998717552508121775, -0.01601477604151182663, 0.000000000000000000 ) ) ;
#15223 = AXIS2_PLACEMENT_3D ( 'NONE', #15980, #19588, #15480 ) ;
#15224 = VERTEX_POINT ( 'NONE', #10520 ) ;
#15225 = DIRECTION ( 'NONE',  ( 0.000000000000000000, 1.000000000000000000, 0.000000000000000000 ) ) ;
#15226 = CARTESIAN_POINT ( 'NONE',  ( -0.03497847339001228933, 2.755905511811024056, 1.180584302963952226 ) ) ;
#15227 = ORIENTED_EDGE ( 'NONE', *, *, #41545, .T. ) ;
#15228 = ORIENTED_EDGE ( 'NONE', *, *, #31435, .T. ) ;
#15229 = LINE ( 'NONE', #23988, #48928 ) ;
#15230 = LINE ( 'NONE', #30979, #10532 ) ;
#15231 = ORIENTED_EDGE ( 'NONE', *, *, #41481, .T. ) ;
#15232 = CARTESIAN_POINT ( 'NONE',  ( 1.871024688710137163, 0.05788755007212831316, 0.5561875852992870239 ) ) ;
#15233 = EDGE_CURVE ( 'NONE', #44818, #19371, #34867, .T. ) ;
#15234 = VERTEX_POINT ( 'NONE', #22396 ) ;
#15235 = CARTESIAN_POINT ( 'NONE',  ( -2.182111253630085290, 3.346456692913386100, 0.6299212598425164567 ) ) ;
#15236 = ORIENTED_EDGE ( 'NONE', *, *, #22020, .F. ) ;
#15237 = EDGE_CURVE ( 'NONE', #22113, #37228, #33017, .T. ) ;
#15238 = CARTESIAN_POINT ( 'NONE',  ( -0.2727639067037602172, 3.346456692913386100, 2.047244094488179567 ) ) ;
#15239 = CARTESIAN_POINT ( 'NONE',  ( 1.287906020515830141, 3.267716535433071279, -4.468321617281355077E-16 ) ) ;
#15240 = EDGE_CURVE ( 'NONE', #19363, #43652, #44852, .T. ) ;
#15241 = EDGE_CURVE ( 'NONE', #22479, #35392, #38897, .T. ) ;
#15242 = VERTEX_POINT ( 'NONE', #46863 ) ;
#15243 = FACE_OUTER_BOUND ( 'NONE', #29667, .T. ) ;
#15244 = AXIS2_PLACEMENT_3D ( 'NONE', #44158, #27898, #11650 ) ;
#15245 = ORIENTED_EDGE ( 'NONE', *, *, #24712, .T. ) ;
#15246 = EDGE_LOOP ( 'NONE', ( #11885, #24819, #8315, #44542 ) ) ;
#15247 = VECTOR ( 'NONE', #5439, 39.37007874015748143 ) ;
#15248 = CARTESIAN_POINT ( 'NONE',  ( -0.5756566573089003658, 1.611847391933241669, 2.896516654582634853 ) ) ;
#15249 = CARTESIAN_POINT ( 'NONE',  ( -1.863748091109392213, 3.267716535433071279, -1.102362204724405492 ) ) ;
#15250 = CARTESIAN_POINT ( 'NONE',  ( -0.9156248155784967313, -0.6299212598425202314, 1.033395398741681293 ) ) ;
#15251 = VECTOR ( 'NONE', #22609, 39.37007874015748143 ) ;
#15252 = ORIENTED_EDGE ( 'NONE', *, *, #1917, .T. ) ;
#15253 = LINE ( 'NONE', #11130, #31991 ) ;
#15254 = EDGE_CURVE ( 'NONE', #3461, #15126, #3788, .T. ) ;
#15255 = LINE ( 'NONE', #42613, #20887 ) ;
#15256 = VERTEX_POINT ( 'NONE', #31408 ) ;
#15257 = DIRECTION ( 'NONE',  ( -1.000000000000000000, 0.000000000000000000, 0.000000000000000000 ) ) ;
#15258 = CIRCLE ( 'NONE', #47353, 2.165354330708661568 ) ;
#15259 = EDGE_CURVE ( 'NONE', #32429, #20197, #35285, .T. ) ;
#15260 = ORIENTED_EDGE ( 'NONE', *, *, #24324, .F. ) ;
#15261 = ORIENTED_EDGE ( 'NONE', *, *, #34069, .F. ) ;
#15262 = ORIENTED_EDGE ( 'NONE', *, *, #21437, .F. ) ;
#15263 = CARTESIAN_POINT ( 'NONE',  ( 0.000000000000000000, 3.267716535433071279, 0.000000000000000000 ) ) ;
#15264 = PLANE ( 'NONE',  #26638 ) ;
#15265 = SHAPE_REPRESENTATION ( 'Back Cover', ( #26741 ), #3635 ) ;
#15266 = ADVANCED_FACE ( 'NONE', ( #50966 ), #1066, .T. ) ;
#15267 = CARTESIAN_POINT ( 'NONE',  ( 0.000000000000000000, 3.267716535433071279, -0.3149606299212593941 ) ) ;
#15268 = CARTESIAN_POINT ( 'NONE',  ( -0.2727639067037607723, 3.346456692913386100, -0.7874015748031470974 ) ) ;
#15269 = EDGE_LOOP ( 'NONE', ( #24836, #26494, #23562, #5196 ) ) ;
#15270 = ORIENTED_EDGE ( 'NONE', *, *, #29122, .F. ) ;
#15271 = CARTESIAN_POINT ( 'NONE',  ( -1.331808205664968492, 0.000000000000000000, 1.125026879082024367 ) ) ;
#15272 = CARTESIAN_POINT ( 'NONE',  ( 0.000000000000000000, 3.267716535433071279, 0.1181102362204698858 ) ) ;
#15273 = VERTEX_POINT ( 'NONE', #42763 ) ;
#15274 = CARTESIAN_POINT ( 'NONE',  ( -0.6214413264104945434, 3.267716535433071279, -0.6692913385826760875 ) ) ;
#15275 = EDGE_CURVE ( 'NONE', #20943, #21582, #42255, .T. ) ;
#15276 = CARTESIAN_POINT ( 'NONE',  ( -1.636583440222564301, 3.346456692913386100, -0.3149606299212592275 ) ) ;
#15277 = CARTESIAN_POINT ( 'NONE',  ( 0.5455278134075216556, 3.267716535433071279, 2.034427629037600660 ) ) ;
#15278 = CARTESIAN_POINT ( 'NONE',  ( 1.472219874544873131, 1.643743200001983151, 2.560030851058970214 ) ) ;
#15279 = CARTESIAN_POINT ( 'NONE',  ( 1.015142113812069091, 3.267716535433071279, -2.222792731763669760 ) ) ;
#15280 = EDGE_LOOP ( 'NONE', ( #27056, #7889, #26178, #648 ) ) ;
#15281 = VECTOR ( 'NONE', #46865, 39.37007874015748143 ) ;
#15282 = FACE_OUTER_BOUND ( 'NONE', #36550, .T. ) ;
#15283 = DIRECTION ( 'NONE',  ( -1.000000000000000000, 0.000000000000000000, 0.000000000000000000 ) ) ;
#15284 = VECTOR ( 'NONE', #28642, 39.37007874015748143 ) ;
#15285 = EDGE_CURVE ( 'NONE', #383, #17591, #50706, .T. ) ;
#15286 = AXIS2_PLACEMENT_3D ( 'NONE', #6489, #3110, #26848 ) ;
#15287 = VERTEX_POINT ( 'NONE', #47108 ) ;
#15288 = PLANE ( 'NONE',  #49596 ) ;
#15289 = FACE_OUTER_BOUND ( 'NONE', #434, .T. ) ;
#15290 = LINE ( 'NONE', #35166, #3247 ) ;
#15291 = VECTOR ( 'NONE', #27615, 39.37007874015748143 ) ;
#15292 = ORIENTED_EDGE ( 'NONE', *, *, #22581, .F. ) ;
#15293 = AXIS2_PLACEMENT_3D ( 'NONE', #10420, #26169, #45503 ) ;
#15294 = ORIENTED_EDGE ( 'NONE', *, *, #35249, .F. ) ;
#15295 = DIRECTION ( 'NONE',  ( 3.586865599282270385E-17, -1.000000000000000000, 1.103923720497139891E-16 ) ) ;
#15296 = ORIENTED_EDGE ( 'NONE', *, *, #11, .F. ) ;
#15297 = LINE ( 'NONE', #39040, #5625 ) ;
#15298 = ORIENTED_EDGE ( 'NONE', *, *, #41563, .T. ) ;
#15299 = EDGE_CURVE ( 'NONE', #40355, #8503, #43008, .T. ) ;
#15300 = DIRECTION ( 'NONE',  ( -1.000000000000000000, -0.000000000000000000, -0.000000000000000000 ) ) ;
#15301 = DIRECTION ( 'NONE',  ( 1.734723475976806848E-16, 0.000000000000000000, 1.000000000000000000 ) ) ;
#15302 = CARTESIAN_POINT ( 'NONE',  ( -0.8182917201112819283, 3.267716535433071279, -2.047244094488181343 ) ) ;
#15303 = EDGE_CURVE ( 'NONE', #7498, #19545, #23657, .T. ) ;
#15304 = ORIENTED_EDGE ( 'NONE', *, *, #35534, .F. ) ;
#15305 = ORIENTED_EDGE ( 'NONE', *, *, #45428, .T. ) ;
#15306 = VERTEX_POINT ( 'NONE', #11531 ) ;
#15307 = FACE_OUTER_BOUND ( 'NONE', #14104, .T. ) ;
#15308 = DIRECTION ( 'NONE',  ( -1.000000000000000000, 0.000000000000000000, -0.000000000000000000 ) ) ;
#15309 = ORIENTED_EDGE ( 'NONE', *, *, #5065, .T. ) ;
#15310 = ORIENTED_EDGE ( 'NONE', *, *, #41453, .T. ) ;
#15311 = DIRECTION ( 'NONE',  ( -0.000000000000000000, 1.000000000000000000, -0.000000000000000000 ) ) ;
#15312 = LINE ( 'NONE', #6565, #15367 ) ;
#15313 = CARTESIAN_POINT ( 'NONE',  ( 1.871024688710137163, 0.05788755007212831316, 0.5561875852992870239 ) ) ;
#15314 = ORIENTED_EDGE ( 'NONE', *, *, #44369, .F. ) ;
#15315 = VERTEX_POINT ( 'NONE', #38653 ) ;
#15316 = CARTESIAN_POINT ( 'NONE',  ( -0.8942052331142552601, 3.267716535433071279, -0.6299212598425177889 ) ) ;
#15317 = CARTESIAN_POINT ( 'NONE',  ( 0.2430652128771965126, 6.692913385826772199, -2.151668812760857197 ) ) ;
#15318 = DIRECTION ( 'NONE',  ( 1.000000000000000000, -0.000000000000000000, 0.000000000000000000 ) ) ;
#15319 = EDGE_LOOP ( 'NONE', ( #15310, #46189, #17852, #16222 ) ) ;
#15320 = CARTESIAN_POINT ( 'NONE',  ( 2.106197740627111958, 3.267716535433071279, -7.307341331430321661E-16 ) ) ;
#15321 = DIRECTION ( 'NONE',  ( 1.000000000000000000, 0.000000000000000000, 0.000000000000000000 ) ) ;
#15322 = VECTOR ( 'NONE', #46740, 39.37007874015748854 ) ;
#15323 = VERTEX_POINT ( 'NONE', #3029 ) ;
#15324 = AXIS2_PLACEMENT_3D ( 'NONE', #29167, #44906, #22453 ) ;
#15325 = LINE ( 'NONE', #26687, #34859 ) ;
#15326 = VERTEX_POINT ( 'NONE', #14649 ) ;
#15327 = ORIENTED_EDGE ( 'NONE', *, *, #41409, .T. ) ;
#15328 = CARTESIAN_POINT ( 'NONE',  ( 1.015142113812069313, 3.267716535433071279, 1.102362204724403938 ) ) ;
#15329 = CARTESIAN_POINT ( 'NONE',  ( -2.150793259809249847, 1.575027863729615341, -0.2506944975021367372 ) ) ;
#15330 = AXIS2_PLACEMENT_3D ( 'NONE', #23998, #7492, #19349 ) ;
#15331 = DIRECTION ( 'NONE',  ( -3.469446951953613696E-16, 0.000000000000000000, -1.000000000000000000 ) ) ;
#15332 = AXIS2_PLACEMENT_3D ( 'NONE', #28200, #9357, #40352 ) ;
#15333 = EDGE_CURVE ( 'NONE', #13884, #18498, #3531, .T. ) ;
#15334 = LINE ( 'NONE', #30833, #3023 ) ;
#15335 = LINE ( 'NONE', #30834, #39492 ) ;
#15336 = ORIENTED_EDGE ( 'NONE', *, *, #14055, .F. ) ;
#15337 = ORIENTED_EDGE ( 'NONE', *, *, #27647, .T. ) ;
#15338 = VECTOR ( 'NONE', #26042, 39.37007874015748143 ) ;
#15339 = ORIENTED_EDGE ( 'NONE', *, *, #28389, .T. ) ;
#15340 = DIRECTION ( 'NONE',  ( -0.000000000000000000, 1.000000000000000000, -0.000000000000000000 ) ) ;
#15341 = EDGE_CURVE ( 'NONE', #31898, #34706, #15412, .T. ) ;
#15342 = DIRECTION ( 'NONE',  ( -1.156482317317871478E-16, 0.000000000000000000, -1.000000000000000000 ) ) ;
#15343 = ADVANCED_FACE ( 'NONE', ( #34276 ), #23397, .F. ) ;
#15344 = EDGE_CURVE ( 'NONE', #17266, #2383, #49966, .T. ) ;
#15345 = CARTESIAN_POINT ( 'NONE',  ( 1.636583440222563857, 0.000000000000000000, 0.4330708661417290162 ) ) ;
#15346 = FACE_OUTER_BOUND ( 'NONE', #28509, .T. ) ;
#15347 = CARTESIAN_POINT ( 'NONE',  ( 0.5455278134075217666, 3.346456692913386100, 1.574803149606291974 ) ) ;
#15348 = ORIENTED_EDGE ( 'NONE', *, *, #10596, .F. ) ;
#15349 = LINE ( 'NONE', #3217, #20901 ) ;
#15350 = EDGE_CURVE ( 'NONE', #22912, #19510, #30396, .T. ) ;
#15351 = CARTESIAN_POINT ( 'NONE',  ( -2.182111253630085290, 3.346456692913386100, -0.3149606299212589500 ) ) ;
#15352 = EDGE_CURVE ( 'NONE', #12933, #15273, #10770, .T. ) ;
#15353 = VERTEX_POINT ( 'NONE', #50457 ) ;
#15354 = CARTESIAN_POINT ( 'NONE',  ( -0.1516021625288302144, 1.672665368615215975, -2.233444876663337908 ) ) ;
#15355 = CARTESIAN_POINT ( 'NONE',  ( 0.8182917201112821504, 3.267716535433071279, -1.419509857074483539E-16 ) ) ;
#15356 = CARTESIAN_POINT ( 'NONE',  ( -1.221295136473707243, 0.000000000000000000, 1.323086612934683215 ) ) ;
#15357 = VECTOR ( 'NONE', #8611, 39.37007874015748143 ) ;
#15358 = DIRECTION ( 'NONE',  ( 1.734723475976806848E-16, 0.000000000000000000, 1.000000000000000000 ) ) ;
#15359 = LINE ( 'NONE', #19471, #43245 ) ;
#15360 = CARTESIAN_POINT ( 'NONE',  ( 2.695799277629594037, 1.453624836071520265, -1.205759334241453651 ) ) ;
#15361 = AXIS2_PLACEMENT_3D ( 'NONE', #48684, #17492, #41250 ) ;
#15362 = VECTOR ( 'NONE', #8164, 39.37007874015748143 ) ;
#15363 = VERTEX_POINT ( 'NONE', #30648 ) ;
#15364 = FACE_OUTER_BOUND ( 'NONE', #14734, .T. ) ;
#15365 = ORIENTED_EDGE ( 'NONE', *, *, #11516, .T. ) ;
#15366 = PLANE ( 'NONE',  #41054 ) ;
#15367 = VECTOR ( 'NONE', #22307, 39.37007874015748143 ) ;
#15368 = ADVANCED_FACE ( 'NONE', ( #46362 ), #11026, .F. ) ;
#15369 = LINE ( 'NONE', #42219, #36709 ) ;
#15370 = CARTESIAN_POINT ( 'NONE',  ( -1.363819533518803029, 3.346456692913386100, 0.1574803149606287811 ) ) ;
#15371 = CONICAL_SURFACE ( 'NONE', #36013, 3.483074324928249421, 1.244861948955335196 ) ;
#15372 = EDGE_CURVE ( 'NONE', #43170, #49343, #19017, .T. ) ;
#15373 = AXIS2_PLACEMENT_3D ( 'NONE', #22871, #15123, #30876 ) ;
#15374 = ORIENTED_EDGE ( 'NONE', *, *, #41773, .T. ) ;
#15375 = ORIENTED_EDGE ( 'NONE', *, *, #8889, .T. ) ;
#15376 = CARTESIAN_POINT ( 'NONE',  ( -1.023703982469668539, 0.003911508537882584999, -1.492733126648604136 ) ) ;
#15377 = EDGE_CURVE ( 'NONE', #35545, #10279, #23329, .T. ) ;
#15378 = CARTESIAN_POINT ( 'NONE',  ( 2.083268748869757658, 3.346456692913386100, 0.5905511811023582691 ) ) ;
#15379 = LINE ( 'NONE', #46582, #14339 ) ;
#15380 = DIRECTION ( 'NONE',  ( 1.734723475976806848E-16, -0.000000000000000000, 1.000000000000000000 ) ) ;
#15381 = CARTESIAN_POINT ( 'NONE',  ( 0.3136974817028393425, 1.724153038295522800, -2.936457595020219635 ) ) ;
#15382 = CARTESIAN_POINT ( 'NONE',  ( -1.695772546416001836, 1.692832103184166437, -2.417756147381374010 ) ) ;
#15383 = EDGE_LOOP ( 'NONE', ( #36199, #50338, #11956, #6323 ) ) ;
#15384 = ORIENTED_EDGE ( 'NONE', *, *, #28234, .T. ) ;
#15385 = LINE ( 'NONE', #42983, #44715 ) ;
#15386 = CARTESIAN_POINT ( 'NONE',  ( -0.2727639067037607723, 3.346456692913386100, 0.1574803149606283648 ) ) ;
#15387 = ORIENTED_EDGE ( 'NONE', *, *, #46450, .F. ) ;
#15388 = CARTESIAN_POINT ( 'NONE',  ( -0.5455278134075214336, 3.267716535433071279, -1.456692913385822630 ) ) ;
#15389 = ORIENTED_EDGE ( 'NONE', *, *, #4236, .T. ) ;
#15390 = VERTEX_POINT ( 'NONE', #8936 ) ;
#15391 = B_SPLINE_CURVE_WITH_KNOTS ( 'NONE', 3,
 ( #32073, #5660, #21407, #47763 ),
 .UNSPECIFIED., .F., .F.,
 ( 4, 4 ),
 ( 0.001762245066137694887, 0.04551044212210949430 ),
 .UNSPECIFIED. ) ;
#15392 = VECTOR ( 'NONE', #6906, 39.37007874015748143 ) ;
#15393 = ORIENTED_EDGE ( 'NONE', *, *, #41242, .T. ) ;
#15394 = ORIENTED_EDGE ( 'NONE', *, *, #7683, .F. ) ;
#15395 = LINE ( 'NONE', #19253, #12076 ) ;
#15396 = ORIENTED_EDGE ( 'NONE', *, *, #10049, .F. ) ;
#15397 = CIRCLE ( 'NONE', #28582, 2.165354330708661568 ) ;
#15398 = VECTOR ( 'NONE', #14838, 39.37007874015748143 ) ;
#15399 = B_SPLINE_CURVE_WITH_KNOTS ( 'NONE', 3,
 ( #19014, #42511, #50455, #4045 ),
 .UNSPECIFIED., .F., .F.,
 ( 4, 4 ),
 ( 2.472935563822449734E-07, 0.01679640739751839945 ),
 .UNSPECIFIED. ) ;
#15400 = CARTESIAN_POINT ( 'NONE',  ( 1.015142113812069313, 3.346456692913386100, -0.7874015748031473194 ) ) ;
#15401 = DIRECTION ( 'NONE',  ( -1.000000000000000000, 0.000000000000000000, 1.734723475976806848E-16 ) ) ;
#15402 = CARTESIAN_POINT ( 'NONE',  ( -1.636583440222564301, 0.000000000000000000, -0.8267716535433052849 ) ) ;
#15403 = ADVANCED_FACE ( 'NONE', ( #28807 ), #28266, .T. ) ;
#15404 = AXIS2_PLACEMENT_3D ( 'NONE', #27632, #46721, #15763 ) ;
#15405 = ADVANCED_FACE ( 'NONE', ( #155 ), #16171, .F. ) ;
#15406 = CARTESIAN_POINT ( 'NONE',  ( -0.2480359799030329715, 2.755905511811024056, 0.2799391584775194342 ) ) ;
#15407 = ADVANCED_FACE ( 'NONE', ( #31667 ), #35718, .T. ) ;
#15408 = AXIS2_PLACEMENT_3D ( 'NONE', #16657, #32410, #48102 ) ;
#15409 = CARTESIAN_POINT ( 'NONE',  ( 0.000000000000000000, 0.000000000000000000, -2.165354330708661568 ) ) ;
#15410 = CARTESIAN_POINT ( 'NONE',  ( 2.288146023452536149, 0.5219625294164390583, -0.05349855421841626796 ) ) ;
#15411 = VERTEX_POINT ( 'NONE', #40444 ) ;
#15412 = LINE ( 'NONE', #7656, #1887 ) ;
#15413 = CARTESIAN_POINT ( 'NONE',  ( -1.936656578200692369, 1.644074453030845762, 0.9862737574026090304 ) ) ;
#15414 = CARTESIAN_POINT ( 'NONE',  ( 1.214590356376888280, 1.727355838235203667, 1.936932008856820930 ) ) ;
#15415 = CARTESIAN_POINT ( 'NONE',  ( 1.236813753895252166, 1.640077341046696890, -2.681693691597563767 ) ) ;
#15416 = EDGE_LOOP ( 'NONE', ( #36043, #28591, #47098, #5262 ) ) ;
#15417 = CARTESIAN_POINT ( 'NONE',  ( -1.536664496436148184E-16, 0.000000000000000000, 0.1181102362204701633 ) ) ;
#15418 = CARTESIAN_POINT ( 'NONE',  ( 0.2646829987306325571, 0.000000000000000000, -2.940868978332396910 ) ) ;
#15419 = ORIENTED_EDGE ( 'NONE', *, *, #41833, .F. ) ;
#15420 = CARTESIAN_POINT ( 'NONE',  ( -1.363819533518803029, 0.000000000000000000, 0.4724409448818871482 ) ) ;
#15421 = DIRECTION ( 'NONE',  ( 0.000000000000000000, 0.000000000000000000, -1.000000000000000000 ) ) ;
#15422 = LINE ( 'NONE', #31419, #38129 ) ;
#15423 = ADVANCED_FACE ( 'NONE', ( #23917 ), #24939, .T. ) ;
#15424 = ORIENTED_EDGE ( 'NONE', *, *, #39447, .T. ) ;
#15425 = CARTESIAN_POINT ( 'NONE',  ( -0.2708302372837931293, 1.608962593404075214, -2.460163500185826635 ) ) ;
#15426 = DIRECTION ( 'NONE',  ( -0.9998717552508121775, -0.01601477604151182316, 0.000000000000000000 ) ) ;
#15427 = EDGE_CURVE ( 'NONE', #17840, #2919, #36310, .T. ) ;
#15428 = PLANE ( 'NONE',  #15218 ) ;
#15429 = DIRECTION ( 'NONE',  ( 1.000000000000000000, 0.000000000000000000, 0.000000000000000000 ) ) ;
#15430 = ORIENTED_EDGE ( 'NONE', *, *, #9107, .T. ) ;
#15431 = CIRCLE ( 'NONE', #47513, 2.164630168518208109 ) ;
#15432 = EDGE_CURVE ( 'NONE', #22927, #13982, #16689, .T. ) ;
#15433 = VECTOR ( 'NONE', #21325, 39.37007874015748143 ) ;
#15434 = ORIENTED_EDGE ( 'NONE', *, *, #10366, .F. ) ;
#15435 = VERTEX_POINT ( 'NONE', #1192 ) ;
#15436 = EDGE_CURVE ( 'NONE', #20856, #11610, #27452, .T. ) ;
#15437 = CARTESIAN_POINT ( 'NONE',  ( -0.8942052331142547050, 0.000000000000000000, 0.9448818897637749625 ) ) ;
#15438 = EDGE_CURVE ( 'NONE', #972, #1849, #289, .T. ) ;
#15439 = ORIENTED_EDGE ( 'NONE', *, *, #6521, .F. ) ;
#15440 = LINE ( 'NONE', #43550, #15542 ) ;
#15441 = CARTESIAN_POINT ( 'NONE',  ( -1.636583440222564301, 0.000000000000000000, 1.574803149606291530 ) ) ;
#15442 = ORIENTED_EDGE ( 'NONE', *, *, #72, .T. ) ;
#15443 = DIRECTION ( 'NONE',  ( -3.469446951953613696E-16, 0.000000000000000000, -1.000000000000000000 ) ) ;
#15444 = ORIENTED_EDGE ( 'NONE', *, *, #7624, .F. ) ;
#15445 = FACE_OUTER_BOUND ( 'NONE', #13347, .T. ) ;
#15446 = ORIENTED_EDGE ( 'NONE', *, *, #11761, .F. ) ;
#15447 = ORIENTED_EDGE ( 'NONE', *, *, #6762, .F. ) ;
#15448 = LINE ( 'NONE', #47405, #28173 ) ;
#15449 = ORIENTED_EDGE ( 'NONE', *, *, #27515, .F. ) ;
#15450 = CIRCLE ( 'NONE', #40294, 2.244934639244525076 ) ;
#15451 = FACE_OUTER_BOUND ( 'NONE', #17706, .T. ) ;
#15452 = ORIENTED_EDGE ( 'NONE', *, *, #42857, .T. ) ;
#15453 = VERTEX_POINT ( 'NONE', #12301 ) ;
#15454 = CARTESIAN_POINT ( 'NONE',  ( -1.166969139818015977, 0.000000000000000000, -1.732283464566922726 ) ) ;
#15455 = CARTESIAN_POINT ( 'NONE',  ( -1.905671854841497481, 1.591126119768930147, 2.256015092822653223 ) ) ;
#15456 = EDGE_LOOP ( 'NONE', ( #38456, #11324, #23619 ) ) ;
#15457 = B_SPLINE_CURVE_WITH_KNOTS ( 'NONE', 3,
 ( #6318, #29554, #9680, #33443 ),
 .UNSPECIFIED., .F., .F.,
 ( 4, 4 ),
 ( 1.069002736119642924E-05, 0.002510697369532217862 ),
 .UNSPECIFIED. ) ;
#15458 = FACE_OUTER_BOUND ( 'NONE', #15943, .T. ) ;
#15459 = ORIENTED_EDGE ( 'NONE', *, *, #41091, .F. ) ;
#15460 = PLANE ( 'NONE',  #44973 ) ;
#15461 = FACE_OUTER_BOUND ( 'NONE', #31434, .T. ) ;
#15462 = AXIS2_PLACEMENT_3D ( 'NONE', #36472, #33377, #45205 ) ;
#15463 = VECTOR ( 'NONE', #23730, 39.37007874015748143 ) ;
#15464 = DIRECTION ( 'NONE',  ( 1.000000000000000000, 0.000000000000000000, -3.469446951953613696E-16 ) ) ;
#15465 = ORIENTED_EDGE ( 'NONE', *, *, #2755, .T. ) ;
#15466 = VERTEX_POINT ( 'NONE', #48138 ) ;
#15467 = EDGE_CURVE ( 'NONE', #12919, #36525, #4553, .T. ) ;
#15468 = CARTESIAN_POINT ( 'NONE',  ( 0.5469786881612729301, 0.03668053021573630668, -1.796948620166157307 ) ) ;
#15469 = DIRECTION ( 'NONE',  ( -4.561975526775755056E-17, -1.000000000000000000, 1.067327232801816862E-16 ) ) ;
#15470 = ADVANCED_FACE ( 'NONE', ( #12041 ), #12551, .F. ) ;
#15471 = DIRECTION ( 'NONE',  ( -0.3513748240813434620, 0.000000000000000000, 0.9362348706397368714 ) ) ;
#15472 = VECTOR ( 'NONE', #50502, 39.37007874015748143 ) ;
#15473 = CARTESIAN_POINT ( 'NONE',  ( 2.152441353505198940, 1.205361022782829114E-17, -0.2419059403264799679 ) ) ;
#15474 = ADVANCED_FACE ( 'NONE', ( #12816 ), #418, .F. ) ;
#15475 = DIRECTION ( 'NONE',  ( 1.142080616180681165E-16, -1.000000000000000000, -2.072570748943160811E-17 ) ) ;
#15476 = FACE_OUTER_BOUND ( 'NONE', #15246, .T. ) ;
#15477 = ORIENTED_EDGE ( 'NONE', *, *, #10476, .F. ) ;
#15478 = CARTESIAN_POINT ( 'NONE',  ( -1.091055626815042645, 0.000000000000000000, -0.6299212598425177889 ) ) ;
#15479 = ORIENTED_EDGE ( 'NONE', *, *, #14243, .T. ) ;
#15480 = DIRECTION ( 'NONE',  ( 0.000000000000000000, 0.000000000000000000, -1.000000000000000000 ) ) ;
#15481 = AXIS2_PLACEMENT_3D ( 'NONE', #50649, #10965, #3981 ) ;
#15482 = EDGE_LOOP ( 'NONE', ( #264, #44647, #13917, #41430 ) ) ;
#15483 = ORIENTED_EDGE ( 'NONE', *, *, #28866, .T. ) ;
#15484 = CARTESIAN_POINT ( 'NONE',  ( -0.3486774197067339376, 3.346456692913386100, 2.204724409448808764 ) ) ;
#15485 = CARTESIAN_POINT ( 'NONE',  ( 0.5455278134075211005, 3.267716535433071279, -0.1968503937007880511 ) ) ;
#15486 = EDGE_CURVE ( 'NONE', #10410, #16704, #8427, .T. ) ;
#15487 = EDGE_LOOP ( 'NONE', ( #30754, #25053, #28007, #6346 ) ) ;
#15488 = CARTESIAN_POINT ( 'NONE',  ( -0.5455278134075211005, 3.267716535433071279, 9.463399047163219482E-17 ) ) ;
#15489 = EDGE_CURVE ( 'NONE', #31373, #3078, #18400, .T. ) ;
#15490 = ORIENTED_EDGE ( 'NONE', *, *, #3458, .T. ) ;
#15491 = DIRECTION ( 'NONE',  ( 1.734723475976806848E-16, 0.000000000000000000, 1.000000000000000000 ) ) ;
#15492 = ORIENTED_EDGE ( 'NONE', *, *, #29759, .T. ) ;
#15493 = PLANE ( 'NONE',  #24397 ) ;
#15494 = DIRECTION ( 'NONE',  ( -0.000000000000000000, 1.000000000000000000, -0.000000000000000000 ) ) ;
#15495 = VECTOR ( 'NONE', #20510, 39.37007874015748143 ) ;
#15496 = CIRCLE ( 'NONE', #2312, 2.246510896728926010 ) ;
#15497 = VERTEX_POINT ( 'NONE', #47876 ) ;
#15498 = CARTESIAN_POINT ( 'NONE',  ( 2.182111253630085290, 3.346456692913386100, -0.5118110236220471121 ) ) ;
#15499 = VERTEX_POINT ( 'NONE', #28290 ) ;
#15500 = VERTEX_POINT ( 'NONE', #44037 ) ;
#15501 = LINE ( 'NONE', #20119, #8691 ) ;
#15502 = CARTESIAN_POINT ( 'NONE',  ( 0.7308738700548030875, -2.448952757038419718E-16, 2.087463732006447081 ) ) ;
#15503 = LINE ( 'NONE', #10868, #47421 ) ;
#15504 = AXIS2_PLACEMENT_3D ( 'NONE', #13679, #5677, #21679 ) ;
#15505 = VERTEX_POINT ( 'NONE', #20555 ) ;
#15506 = AXIS2_PLACEMENT_3D ( 'NONE', #48784, #13465, #5719 ) ;
#15507 = DIRECTION ( 'NONE',  ( -0.000000000000000000, -1.000000000000000000, -0.000000000000000000 ) ) ;
#15508 = DIRECTION ( 'NONE',  ( -0.000000000000000000, 0.000000000000000000, 1.000000000000000000 ) ) ;
#15509 = ORIENTED_EDGE ( 'NONE', *, *, #20955, .T. ) ;
#15510 = AXIS2_PLACEMENT_3D ( 'NONE', #6699, #34576, #14699 ) ;
#15511 = DIRECTION ( 'NONE',  ( -0.000000000000000000, 1.000000000000000000, -0.000000000000000000 ) ) ;
#15512 = EDGE_LOOP ( 'NONE', ( #33763, #1541, #50946, #27897, #51003, #47122 ) ) ;
#15513 = ORIENTED_EDGE ( 'NONE', *, *, #16762, .T. ) ;
#15514 = CIRCLE ( 'NONE', #32866, 1.850107469027523432 ) ;
#15515 = EDGE_LOOP ( 'NONE', ( #38532, #29207, #8780, #41100 ) ) ;
#15516 = DIRECTION ( 'NONE',  ( 1.734723475976806848E-16, -0.000000000000000000, 1.000000000000000000 ) ) ;
#15517 = PLANE ( 'NONE',  #37386 ) ;
#15518 = DIRECTION ( 'NONE',  ( -1.000000000000000000, 0.000000000000000000, 1.734723475976806848E-16 ) ) ;
#15519 = LINE ( 'NONE', #43120, #27990 ) ;
#15520 = ORIENTED_EDGE ( 'NONE', *, *, #22543, .F. ) ;
#15521 = EDGE_LOOP ( 'NONE', ( #41654, #33896, #16260, #33156 ) ) ;
#15522 = EDGE_CURVE ( 'NONE', #41844, #9230, #934, .T. ) ;
#15523 =( NAMED_UNIT ( * ) SI_UNIT ( $, .STERADIAN. ) SOLID_ANGLE_UNIT ( ) );
#15524 = EDGE_CURVE ( 'NONE', #13212, #13391, #48267, .T. ) ;
#15525 = CARTESIAN_POINT ( 'NONE',  ( 0.4696143004045484903, 0.000000000000000000, 1.102362204724404160 ) ) ;
#15526 = ORIENTED_EDGE ( 'NONE', *, *, #6783, .T. ) ;
#15527 = DIRECTION ( 'NONE',  ( 1.000000000000000000, 0.000000000000000000, 0.000000000000000000 ) ) ;
#15528 = LINE ( 'NONE', #47995, #22660 ) ;
#15529 = EDGE_CURVE ( 'NONE', #33353, #47061, #13583, .T. ) ;
#15530 = PRODUCT_RELATED_PRODUCT_CATEGORY ( 'part', '', ( #43784 ) ) ;
#15531 = AXIS2_PLACEMENT_3D ( 'NONE', #33551, #13918, #40065 ) ;
#15532 = ADVANCED_FACE ( 'NONE', ( #33970, #17957 ), #9959, .F. ) ;
#15533 = FACE_OUTER_BOUND ( 'NONE', #23358, .T. ) ;
#15534 = DIRECTION ( 'NONE',  ( -0.000000000000000000, 0.000000000000000000, 1.000000000000000000 ) ) ;
#15535 = CARTESIAN_POINT ( 'NONE',  ( 0.000000000000000000, 0.000000000000000000, -2.874015748031496731 ) ) ;
#15536 = EDGE_LOOP ( 'NONE', ( #5578, #29290, #33422, #19462 ) ) ;
#15537 = DIRECTION ( 'NONE',  ( -0.01601477604151182663, 0.9998717552508123996, -0.000000000000000000 ) ) ;
#15538 = CARTESIAN_POINT ( 'NONE',  ( 0.1067246931122726866, 0.02962905676920215767, 0.000000000000000000 ) ) ;
#15539 = VECTOR ( 'NONE', #36480, 39.37007874015748143 ) ;
#15540 = VERTEX_POINT ( 'NONE', #29056 ) ;
#15541 = ORIENTED_EDGE ( 'NONE', *, *, #12415, .T. ) ;
#15543 = CARTESIAN_POINT ( 'NONE',  ( 0.000000000000000000, 3.267716535433071279, -2.047244094488181343 ) ) ;
#15542 = VECTOR ( 'NONE', #16903, 39.37007874015748143 ) ;
#15544 = PLANE ( 'NONE',  #31915 ) ;
#15545 = EDGE_CURVE ( 'NONE', #24313, #45537, #5317, .T. ) ;
#15546 = ORIENTED_EDGE ( 'NONE', *, *, #3295, .T. ) ;
#15547 = VECTOR ( 'NONE', #43821, 39.37007874015748143 ) ;
#15548 = ADVANCED_FACE ( 'NONE', ( #30088 ), #49656, .F. ) ;
#15549 = ORIENTED_EDGE ( 'NONE', *, *, #48840, .F. ) ;
#15550 = LINE ( 'NONE', #32070, #13059 ) ;
#15551 = EDGE_LOOP ( 'NONE', ( #18171, #2151, #29318, #8973, #25134, #8595, #27695, #42772, #30319, #8155, #15932, #23707, #10124 ) ) ;
#15552 = VECTOR ( 'NONE', #4302, 39.37007874015748143 ) ;
#15553 = LINE ( 'NONE', #7800, #31982 ) ;
#15554 = ORIENTED_EDGE ( 'NONE', *, *, #30839, .F. ) ;
#15555 = DIRECTION ( 'NONE',  ( -0.000000000000000000, 1.000000000000000000, -0.000000000000000000 ) ) ;
#15557 = AXIS2_PLACEMENT_3D ( 'NONE', #17503, #33263, #48949 ) ;
#15556 = PLANE ( 'NONE',  #8253 ) ;
#15558 = CARTESIAN_POINT ( 'NONE',  ( -1.738729679588005617, 0.000000000000000000, -0.1273486421340072894 ) ) ;
#15559 = EDGE_LOOP ( 'NONE', ( #36134, #40167, #15888, #47646 ) ) ;
#15560 = EDGE_LOOP ( 'NONE', ( #84, #32477, #32390, #37298 ) ) ;
#15561 = ORIENTED_EDGE ( 'NONE', *, *, #44271, .F. ) ;
#15562 = LINE ( 'NONE', #47260, #35627 ) ;
#15563 = CARTESIAN_POINT ( 'NONE',  ( 0.000000000000000000, 0.000000000000000000, 0.000000000000000000 ) ) ;
#15564 = ORIENTED_EDGE ( 'NONE', *, *, #17698, .F. ) ;
#15565 = ORIENTED_EDGE ( 'NONE', *, *, #25445, .T. ) ;
#15566 = PLANE ( 'NONE',  #7472 ) ;
#15567 = DIRECTION ( 'NONE',  ( -0.000000000000000000, 0.000000000000000000, 1.000000000000000000 ) ) ;
#15568 = CARTESIAN_POINT ( 'NONE',  ( -2.182111253630085290, 3.346456692913386100, 0.3149606299212578953 ) ) ;
#15569 = ADVANCED_FACE ( 'NONE', ( #1954 ), #44795, .F. ) ;
#15570 = EDGE_LOOP ( 'NONE', ( #21627, #19285, #20650, #24517 ) ) ;
#15571 = ORIENTED_EDGE ( 'NONE', *, *, #16053, .T. ) ;
#15572 = CARTESIAN_POINT ( 'NONE',  ( -0.2727639067037608278, 3.267716535433071279, -1.614173228346451605 ) ) ;
#15573 = DIRECTION ( 'NONE',  ( -1.000000000000000000, 0.000000000000000000, 1.734723475976806848E-16 ) ) ;
#15574 = VECTOR ( 'NONE', #34497, 39.37007874015748143 ) ;
#15575 = DIRECTION ( 'NONE',  ( -0.000000000000000000, 1.000000000000000000, -0.000000000000000000 ) ) ;
#15576 = ORIENTED_EDGE ( 'NONE', *, *, #14076, .T. ) ;
#15577 = PLANE ( 'NONE',  #2645 ) ;
#15578 = CARTESIAN_POINT ( 'NONE',  ( 2.182111253630085290, 3.346456692913386100, 0.3149606299212573401 ) ) ;
#15579 = ORIENTED_EDGE ( 'NONE', *, *, #23681, .F. ) ;
#15580 = DIRECTION ( 'NONE',  ( 0.000000000000000000, 0.000000000000000000, -1.000000000000000000 ) ) ;
#15581 = ORIENTED_EDGE ( 'NONE', *, *, #28972, .T. ) ;
#15582 = EDGE_LOOP ( 'NONE', ( #9603, #25182, #21470 ) ) ;
#15583 = CARTESIAN_POINT ( 'NONE',  ( 1.363819533518803251, 3.346456692913386100, -0.1574803149606304187 ) ) ;
#15584 = CARTESIAN_POINT ( 'NONE',  ( 1.985331756560078986, 0.01929593017201648025, 0.5933282030623656667 ) ) ;
#15585 = AXIS2_PLACEMENT_3D ( 'NONE', #21566, #37326, #17690 ) ;
#15586 = DIRECTION ( 'NONE',  ( 0.000000000000000000, 0.000000000000000000, -1.000000000000000000 ) ) ;
#15587 = CARTESIAN_POINT ( 'NONE',  ( 0.8067290215917983787, 1.574803149606302854, 2.009464521518182334 ) ) ;
#15589 = FACE_OUTER_BOUND ( 'NONE', #13241, .T. ) ;
#15588 = VECTOR ( 'NONE', #3905, 39.37007874015748143 ) ;
#15590 = ORIENTED_EDGE ( 'NONE', *, *, #47528, .F. ) ;
#15591 = VERTEX_POINT ( 'NONE', #37850 ) ;
#15592 = VECTOR ( 'NONE', #24886, 39.37007874015748143 ) ;
#15593 = ORIENTED_EDGE ( 'NONE', *, *, #36468, .F. ) ;
#15594 = CARTESIAN_POINT ( 'NONE',  ( 2.182111253630085290, 0.000000000000000000, 0.6299212598425161236 ) ) ;
#15595 = DIRECTION ( 'NONE',  ( -3.469446951953613696E-16, 0.000000000000000000, -1.000000000000000000 ) ) ;
#15596 = ADVANCED_FACE ( 'NONE', ( #36822 ), #17199, .F. ) ;
#15597 = ADVANCED_FACE ( 'NONE', ( #29581 ), #13832, .F. ) ;
#15598 = LINE ( 'NONE', #18463, #34419 ) ;
#15599 = PLANE ( 'NONE',  #50869 ) ;
#15600 = EDGE_LOOP ( 'NONE', ( #20903, #10561, #26975, #12192 ) ) ;
#15601 = CARTESIAN_POINT ( 'NONE',  ( -0.04921259842519708910, 1.718497255264965551, 2.952755905511811108 ) ) ;
#15602 = CARTESIAN_POINT ( 'NONE',  ( -0.5455278134075208785, 3.346456692913386100, 0.4330708661417290162 ) ) ;
#15603 = EDGE_LOOP ( 'NONE', ( #49381, #7488, #38351, #6171 ) ) ;
#15604 = FACE_OUTER_BOUND ( 'NONE', #26407, .T. ) ;
#15605 = LINE ( 'NONE', #47053, #50810 ) ;
#15606 = DIRECTION ( 'NONE',  ( 1.558091277195270436E-17, -1.000000000000000000, -1.150229170499806500E-16 ) ) ;
#15607 = VECTOR ( 'NONE', #19674, 39.37007874015748143 ) ;
#15608 = ORIENTED_EDGE ( 'NONE', *, *, #3776, .T. ) ;
#15609 = CARTESIAN_POINT ( 'NONE',  ( -2.100227814008681637, 1.588094595312779855, -2.076109931251943763 ) ) ;
#15610 = CARTESIAN_POINT ( 'NONE',  ( -2.437180031585919782, 0.000000000000000000, -1.667735833703134274 ) ) ;
#15611 = CARTESIAN_POINT ( 'NONE',  ( -2.142325647309101022, 3.267716535433071279, -0.3149606299212589500 ) ) ;
#15612 = VERTEX_POINT ( 'NONE', #13326 ) ;
#15613 = DIRECTION ( 'NONE',  ( -1.000000000000000000, 0.000000000000000000, 0.000000000000000000 ) ) ;
#15614 = ORIENTED_EDGE ( 'NONE', *, *, #19065, .F. ) ;
#15615 = CARTESIAN_POINT ( 'NONE',  ( -1.195183497228115035E-16, 3.346456692913386100, -0.6299212598425177889 ) ) ;
#15616 = CIRCLE ( 'NONE', #45300, 2.165354330708661568 ) ;
#15617 = DIRECTION ( 'NONE',  ( -3.469446951953613696E-16, 0.000000000000000000, -1.000000000000000000 ) ) ;
#15618 = DIRECTION ( 'NONE',  ( 1.734723475976806848E-16, -0.000000000000000000, 1.000000000000000000 ) ) ;
#15619 = ADVANCED_FACE ( 'NONE', ( #6076 ), #33210, .F. ) ;
#15620 = VECTOR ( 'NONE', #46816, 39.37007874015748143 ) ;
#15621 = ORIENTED_EDGE ( 'NONE', *, *, #14610, .T. ) ;
#15622 = ORIENTED_EDGE ( 'NONE', *, *, #39092, .F. ) ;
#15623 = LINE ( 'NONE', #18742, #44643 ) ;
#15624 = CARTESIAN_POINT ( 'NONE',  ( 1.786266331718541878, 0.01831036388897721787, 1.017116489302096083 ) ) ;
#15625 = EDGE_LOOP ( 'NONE', ( #43506, #10109, #33643, #24566 ) ) ;
#15626 = CARTESIAN_POINT ( 'NONE',  ( -1.363819533518803473, 0.000000000000000000, -0.1574803149606300023 ) ) ;
#15627 = CARTESIAN_POINT ( 'NONE',  ( -0.2727639067037602727, 0.000000000000000000, 0.9055118110236167750 ) ) ;
#15628 = VECTOR ( 'NONE', #24896, 39.37007874015748143 ) ;
#15629 = CARTESIAN_POINT ( 'NONE',  ( 0.2927555892279174454, 1.720075335370203407, -2.703774112429984111 ) ) ;
#15630 = EDGE_CURVE ( 'NONE', #11815, #21618, #40950, .T. ) ;
#15631 = CARTESIAN_POINT ( 'NONE',  ( 1.287906020515829919, 3.267716535433071279, -2.076684646723067296 ) ) ;
#15632 = ORIENTED_EDGE ( 'NONE', *, *, #23638, .T. ) ;
#15633 = ORIENTED_EDGE ( 'NONE', *, *, #3357, .F. ) ;
#15634 = LINE ( 'NONE', #31385, #1873 ) ;
#15635 = FACE_OUTER_BOUND ( 'NONE', #8386, .T. ) ;
#15636 = ORIENTED_EDGE ( 'NONE', *, *, #22411, .F. ) ;
#15637 = ADVANCED_FACE ( 'NONE', ( #21328 ), #30741, .T. ) ;
#15638 = CARTESIAN_POINT ( 'NONE',  ( -0.07591351300297305427, 3.267716535433071279, 2.633779063002558971E-17 ) ) ;
#15639 = EDGE_LOOP ( 'NONE', ( #49313, #50860, #5237, #41916 ) ) ;
#15640 = ORIENTED_EDGE ( 'NONE', *, *, #38495, .F. ) ;
#15641 = CARTESIAN_POINT ( 'NONE',  ( 1.015142113812069979, 0.000000000000000000, 1.732283464566921172 ) ) ;
#15642 = EDGE_CURVE ( 'NONE', #26109, #34644, #24151, .T. ) ;
#15643 = AXIS2_PLACEMENT_3D ( 'NONE', #44125, #25287, #41045 ) ;
#15644 = ORIENTED_EDGE ( 'NONE', *, *, #32460, .F. ) ;
#15645 = ORIENTED_EDGE ( 'NONE', *, *, #37118, .T. ) ;
#15646 = CARTESIAN_POINT ( 'NONE',  ( -1.091055626815042201, 0.000000000000000000, 1.574803149606291974 ) ) ;
#15647 = ORIENTED_EDGE ( 'NONE', *, *, #20496, .T. ) ;
#15648 = DIRECTION ( 'NONE',  ( -0.000000000000000000, 1.000000000000000000, -0.000000000000000000 ) ) ;
#15649 = LINE ( 'NONE', #26756, #17834 ) ;
#15650 = CARTESIAN_POINT ( 'NONE',  ( -0.2155737599805752913, 0.01633517799311254987, -1.846213753763441545 ) ) ;
#15651 = EDGE_CURVE ( 'NONE', #26854, #31614, #2214, .T. ) ;
#15652 = VECTOR ( 'NONE', #13125, 39.37007874015748143 ) ;
#15653 = FACE_OUTER_BOUND ( 'NONE', #4825, .T. ) ;
#15654 = EDGE_CURVE ( 'NONE', #21553, #8462, #22091, .T. ) ;
#15655 = EDGE_CURVE ( 'NONE', #48919, #44707, #49408, .T. ) ;
#15656 = DIRECTION ( 'NONE',  ( 1.000000000000000000, 0.000000000000000000, 0.000000000000000000 ) ) ;
#15657 = CARTESIAN_POINT ( 'NONE',  ( 1.787005229743228396, 1.641566817664441791, -1.776638477264515181 ) ) ;
#15658 = EDGE_LOOP ( 'NONE', ( #31121, #21864, #4202, #36364 ) ) ;
#15659 = CARTESIAN_POINT ( 'NONE',  ( -1.166969139818015755, 0.000000000000000000, -0.03937007874015868020 ) ) ;
#15660 = VECTOR ( 'NONE', #29467, 39.37007874015748143 ) ;
#15661 = DIRECTION ( 'NONE',  ( -1.729310098864894520E-17, 1.000000000000000000, -1.276627980444842972E-16 ) ) ;
#15662 = DIRECTION ( 'NONE',  ( -3.469446951953613696E-16, 0.000000000000000000, -1.000000000000000000 ) ) ;
#15663 = ORIENTED_EDGE ( 'NONE', *, *, #25858, .T. ) ;
#15664 = DIRECTION ( 'NONE',  ( -3.469446951953613696E-16, 0.000000000000000000, -1.000000000000000000 ) ) ;
#15665 = VERTEX_POINT ( 'NONE', #23336 ) ;
#15666 = LINE ( 'NONE', #425, #21317 ) ;
#15667 = CARTESIAN_POINT ( 'NONE',  ( -1.629664903723128777, 0.001228770104821741253, -0.6430327822565008455 ) ) ;
#15668 = PLANE ( 'NONE',  #36455 ) ;
#15669 = VERTEX_POINT ( 'NONE', #38844 ) ;
#15670 = CARTESIAN_POINT ( 'NONE',  ( 2.500827540798396420, 1.754748926069762405, -1.122424414593431674 ) ) ;
#15671 = CARTESIAN_POINT ( 'NONE',  ( 0.08139965876239094178, 1.610780518492231694, 0.000000000000000000 ) ) ;
#15672 = DIRECTION ( 'NONE',  ( 1.241861098869884156E-16, 1.000000000000000000, 3.427318860986280993E-17 ) ) ;
#15673 = CARTESIAN_POINT ( 'NONE',  ( -0.3486774197067334935, 3.267716535433071279, 1.692913385826762873 ) ) ;
#15674 = ORIENTED_EDGE ( 'NONE', *, *, #50503, .T. ) ;
#15675 = EDGE_CURVE ( 'NONE', #32615, #10700, #2972, .T. ) ;
#15676 = ORIENTED_EDGE ( 'NONE', *, *, #14733, .F. ) ;
#15677 = ORIENTED_EDGE ( 'NONE', *, *, #47918, .T. ) ;
#15678 = DIRECTION ( 'NONE',  ( 1.000000000000000000, 0.000000000000000000, 0.000000000000000000 ) ) ;
#15679 = ORIENTED_EDGE ( 'NONE', *, *, #38686, .T. ) ;
#15680 = CARTESIAN_POINT ( 'NONE',  ( 0.04921259842519683236, 0.5238019749767087729, 2.217183491882336543 ) ) ;
#15681 = FACE_OUTER_BOUND ( 'NONE', #47960, .T. ) ;
#15682 = ORIENTED_EDGE ( 'NONE', *, *, #25840, .F. ) ;
#15683 = EDGE_CURVE ( 'NONE', #19556, #35330, #42457, .T. ) ;
#15684 = VECTOR ( 'NONE', #7904, 39.37007874015748143 ) ;
#15685 = CARTESIAN_POINT ( 'NONE',  ( 0.4696143004045479352, 0.000000000000000000, -0.1574803149606298636 ) ) ;
#15686 = AXIS2_PLACEMENT_3D ( 'NONE', #24348, #40360, #5233 ) ;
#15687 = ADVANCED_FACE ( 'NONE', ( #34472 ), #18467, .F. ) ;
#15688 = VERTEX_POINT ( 'NONE', #35225 ) ;
#15689 = CARTESIAN_POINT ( 'NONE',  ( 0.2727639067037604392, 3.267716535433071279, 0.5905511811023579360 ) ) ;
#15690 = EDGE_CURVE ( 'NONE', #42820, #38377, #25543, .T. ) ;
#15691 = CARTESIAN_POINT ( 'NONE',  ( 2.273698311726526811, 0.5219991175371894165, 0.2583313113525125271 ) ) ;
#15692 = ORIENTED_EDGE ( 'NONE', *, *, #16544, .F. ) ;
#15693 = ORIENTED_EDGE ( 'NONE', *, *, #35532, .T. ) ;
#15694 = LINE ( 'NONE', #15192, #28991 ) ;
#15695 = ORIENTED_EDGE ( 'NONE', *, *, #44122, .T. ) ;
#15696 = VECTOR ( 'NONE', #6175, 39.37007874015748143 ) ;
#15697 = PLANE ( 'NONE',  #5633 ) ;
#15698 = ORIENTED_EDGE ( 'NONE', *, *, #16557, .T. ) ;
#15699 = ORIENTED_EDGE ( 'NONE', *, *, #22505, .T. ) ;
#15700 = ADVANCED_FACE ( 'NONE', ( #30341 ), #26958, .F. ) ;
#15701 = LINE ( 'NONE', #2824, #28241 ) ;
#15702 = DIRECTION ( 'NONE',  ( 1.000000000000000000, 0.000000000000000000, -3.469446951953613696E-16 ) ) ;
#15703 = ORIENTED_EDGE ( 'NONE', *, *, #47431, .T. ) ;
#15704 = ADVANCED_FACE ( 'NONE', ( #49906 ), #14310, .T. ) ;
#15705 = PLANE ( 'NONE',  #22122 ) ;
#15706 = VERTEX_POINT ( 'NONE', #46556 ) ;
#15707 = CARTESIAN_POINT ( 'NONE',  ( -0.2727639067037602727, 3.346456692913386100, 1.220472440944875281 ) ) ;
#15708 = DIRECTION ( 'NONE',  ( 0.000000000000000000, -1.000000000000000000, 0.000000000000000000 ) ) ;
#15710 = EDGE_CURVE ( 'NONE', #27748, #13176, #6844, .T. ) ;
#15709 = CARTESIAN_POINT ( 'NONE',  ( -0.8182917201112819283, 3.267716535433071279, -1.732283464566922726 ) ) ;
#15711 = EDGE_CURVE ( 'NONE', #13982, #36614, #9371, .T. ) ;
#15712 = VERTEX_POINT ( 'NONE', #10967 ) ;
#15713 = VERTEX_POINT ( 'NONE', #50905 ) ;
#15714 = CARTESIAN_POINT ( 'NONE',  ( 0.8182917201112824834, 0.000000000000000000, 2.047244094488179567 ) ) ;
#15715 = LINE ( 'NONE', #38715, #46729 ) ;
#15716 = EDGE_CURVE ( 'NONE', #34643, #22357, #10734, .T. ) ;
#15717 = DIRECTION ( 'NONE',  ( 1.000000000000000000, -0.000000000000000000, 0.000000000000000000 ) ) ;
#15718 = DIRECTION ( 'NONE',  ( -0.000000000000000000, 1.000000000000000000, -0.000000000000000000 ) ) ;
#15719 = CARTESIAN_POINT ( 'NONE',  ( 1.091055626815043311, 3.346456692913386100, 1.574803149606291974 ) ) ;
#15720 = AXIS2_PLACEMENT_3D ( 'NONE', #6597, #43389, #10963 ) ;
#15721 = VECTOR ( 'NONE', #27792, 39.37007874015748143 ) ;
#15722 = DIRECTION ( 'NONE',  ( -0.01601477604151182663, 0.9998717552508123996, -0.000000000000000000 ) ) ;
#15723 = ORIENTED_EDGE ( 'NONE', *, *, #22928, .F. ) ;
#15724 = LINE ( 'NONE', #38966, #44065 ) ;
#15725 = ORIENTED_EDGE ( 'NONE', *, *, #31699, .T. ) ;
#15726 = DIRECTION ( 'NONE',  ( -1.000000000000000000, 0.000000000000000000, 1.734723475976806848E-16 ) ) ;
#15727 = VERTEX_POINT ( 'NONE', #14594 ) ;
#15728 = DIRECTION ( 'NONE',  ( 3.986037398843765983E-20, 1.000000000000000000, 1.160734090543304660E-16 ) ) ;
#15729 = CARTESIAN_POINT ( 'NONE',  ( 1.306991306359274629, 1.630410611703223545, -1.882644677548868550 ) ) ;
#15730 = ORIENTED_EDGE ( 'NONE', *, *, #3396, .T. ) ;
#15731 = DIRECTION ( 'NONE',  ( -0.000000000000000000, -1.000000000000000000, -0.000000000000000000 ) ) ;
#15732 = VERTEX_POINT ( 'NONE', #46060 ) ;
#15733 = LINE ( 'NONE', #27347, #5638 ) ;
#15734 = ORIENTED_EDGE ( 'NONE', *, *, #10579, .F. ) ;
#15735 = FACE_OUTER_BOUND ( 'NONE', #26421, .T. ) ;
#15736 = DIRECTION ( 'NONE',  ( -0.000000000000000000, -1.000000000000000000, -0.000000000000000000 ) ) ;
#15737 = EDGE_CURVE ( 'NONE', #3517, #11390, #18965, .T. ) ;
#15738 = ORIENTED_EDGE ( 'NONE', *, *, #19461, .F. ) ;
#15739 = EDGE_CURVE ( 'NONE', #33931, #18423, #15349, .T. ) ;
#15740 = CARTESIAN_POINT ( 'NONE',  ( -1.599172890215280196, 1.205361022782829114E-17, 1.460879300779170498 ) ) ;
#15741 = ORIENTED_EDGE ( 'NONE', *, *, #31782, .T. ) ;
#15742 = ORIENTED_EDGE ( 'NONE', *, *, #11557, .F. ) ;
#15743 = PRODUCT_DEFINITION_SHAPE ( 'NONE', 'NONE',  #51057 ) ;
#15744 = CARTESIAN_POINT ( 'NONE',  ( -1.363819533518803473, 0.000000000000000000, -0.9842519685039344823 ) ) ;
#15745 = DIRECTION ( 'NONE',  ( -3.469446951953613696E-16, 0.000000000000000000, -1.000000000000000000 ) ) ;
#15746 = DIRECTION ( 'NONE',  ( 0.000000000000000000, 0.000000000000000000, -1.000000000000000000 ) ) ;
#15747 = VECTOR ( 'NONE', #24748, 39.37007874015748143 ) ;
#15748 = ORIENTED_EDGE ( 'NONE', *, *, #8032, .T. ) ;
#15749 = CONICAL_SURFACE ( 'NONE', #26484, 3.483074324928249421, 1.244861948955335196 ) ;
#15750 = LINE ( 'NONE', #47206, #8918 ) ;
#15751 = DIRECTION ( 'NONE',  ( 0.000000000000000000, -1.000000000000000000, 0.000000000000000000 ) ) ;
#15752 = EDGE_LOOP ( 'NONE', ( #13081, #39307, #50289, #10900 ) ) ;
#15753 = CARTESIAN_POINT ( 'NONE',  ( 0.000000000000000000, 3.346456692913386100, 0.000000000000000000 ) ) ;
#15754 = ORIENTED_EDGE ( 'NONE', *, *, #37063, .T. ) ;
#15755 = VERTEX_POINT ( 'NONE', #31351 ) ;
#15756 = VECTOR ( 'NONE', #44762, 39.37007874015748854 ) ;
#15757 = EDGE_CURVE ( 'NONE', #2547, #8994, #7101, .T. ) ;
#15758 = APPLICATION_PROTOCOL_DEFINITION ( 'draft international standard', 'automotive_design', 1998, #7464 ) ;
#15759 = ORIENTED_EDGE ( 'NONE', *, *, #7600, .T. ) ;
#15760 = DIRECTION ( 'NONE',  ( -0.000000000000000000, -1.000000000000000000, -0.000000000000000000 ) ) ;
#15761 = CARTESIAN_POINT ( 'NONE',  ( 1.818390528211208945, 3.267716535433071279, 1.062992125984245639 ) ) ;
#15762 = EDGE_CURVE ( 'NONE', #27808, #12583, #47046, .T. ) ;
#15763 = DIRECTION ( 'NONE',  ( 0.000000000000000000, 0.000000000000000000, -1.000000000000000000 ) ) ;
#15764 = FACE_OUTER_BOUND ( 'NONE', #46938, .T. ) ;
#15765 = EDGE_CURVE ( 'NONE', #351, #35551, #14846, .T. ) ;
#15766 = EDGE_LOOP ( 'NONE', ( #35418, #18180, #31543, #47560, #50732 ) ) ;
#15767 = ORIENTED_EDGE ( 'NONE', *, *, #22505, .F. ) ;
#15768 = CARTESIAN_POINT ( 'NONE',  ( 1.091055626815042645, 3.346456692913386100, 0.7480314960629872445 ) ) ;
#15769 = EDGE_CURVE ( 'NONE', #21408, #33697, #13848, .T. ) ;
#15770 = DIRECTION ( 'NONE',  ( -1.000000000000000000, 0.000000000000000000, 0.000000000000000000 ) ) ;
#15771 = ORIENTED_EDGE ( 'NONE', *, *, #7528, .T. ) ;
#15772 = CARTESIAN_POINT ( 'NONE',  ( 0.1968503937007873017, 3.267716535433071279, -0.3149606299212591165 ) ) ;
#15773 = CARTESIAN_POINT ( 'NONE',  ( -1.441820560696044584, 0.5249316475426859530, 1.212758804667590784 ) ) ;
#15774 = CARTESIAN_POINT ( 'NONE',  ( -0.3739466299075467348, 2.755905511811024056, -1.120342228065320134 ) ) ;
#15775 = LINE ( 'NONE', #31534, #16163 ) ;
#15776 = LINE ( 'NONE', #11907, #24591 ) ;
#15777 = ORIENTED_EDGE ( 'NONE', *, *, #14211, .T. ) ;
#15778 = LINE ( 'NONE', #29710, #24257 ) ;
#15779 = CARTESIAN_POINT ( 'NONE',  ( -1.985260859929297572, 3.346456692913386100, -0.3149606299212589500 ) ) ;
#15780 = EDGE_LOOP ( 'NONE', ( #9800, #3908, #8516, #43812 ) ) ;
#15781 = VECTOR ( 'NONE', #48642, 39.37007874015748143 ) ;
#15782 = VERTEX_POINT ( 'NONE', #22845 ) ;
#15783 = CARTESIAN_POINT ( 'NONE',  ( 2.106197740627112402, 0.000000000000000000, 1.102362204724403938 ) ) ;
#15784 = VECTOR ( 'NONE', #28784, 39.37007874015748143 ) ;
#15785 = CARTESIAN_POINT ( 'NONE',  ( -1.377952755905512472, 0.000000000000000000, -2.845674993400276405E-16 ) ) ;
#15786 = DIRECTION ( 'NONE',  ( -0.000000000000000000, 1.000000000000000000, -0.000000000000000000 ) ) ;
#15787 = ORIENTED_EDGE ( 'NONE', *, *, #17363, .T. ) ;
#15788 = AXIS2_PLACEMENT_3D ( 'NONE', #17920, #40652, #21286 ) ;
#15789 = VERTEX_POINT ( 'NONE', #8105 ) ;
#15790 = DIRECTION ( 'NONE',  ( 0.000000000000000000, 0.000000000000000000, -1.000000000000000000 ) ) ;
#15791 = VECTOR ( 'NONE', #30943, 39.37007874015748143 ) ;
#15792 = VERTEX_POINT ( 'NONE', #4230 ) ;
#15793 = CARTESIAN_POINT ( 'NONE',  ( 0.9432913529151772947, 1.723010488186151878, -2.072188145589165753 ) ) ;
#15794 = EDGE_LOOP ( 'NONE', ( #40090, #39766, #14311, #49133 ) ) ;
#15795 = CARTESIAN_POINT ( 'NONE',  ( 0.000000000000000000, 6.692913385826772199, 0.000000000000000000 ) ) ;
#15796 = CARTESIAN_POINT ( 'NONE',  ( 0.7423782071083087075, 3.346456692913386100, -1.259842519685035134 ) ) ;
#15797 = DIRECTION ( 'NONE',  ( 0.000000000000000000, 0.000000000000000000, 1.000000000000000000 ) ) ;
#15798 = ORIENTED_EDGE ( 'NONE', *, *, #22713, .F. ) ;
#15799 = ADVANCED_FACE ( 'NONE', ( #47561 ), #25028, .T. ) ;
#15800 = ORIENTED_EDGE ( 'NONE', *, *, #9243, .F. ) ;
#15801 = ORIENTED_EDGE ( 'NONE', *, *, #43267, .T. ) ;
#15802 = CARTESIAN_POINT ( 'NONE',  ( -1.675814739737315540, 1.582635513994296250, 1.399362935606387470 ) ) ;
#15803 = CARTESIAN_POINT ( 'NONE',  ( -1.166969139818016199, 0.000000000000000000, 1.535433070866133232 ) ) ;
#15804 = EDGE_CURVE ( 'NONE', #13670, #47197, #43458, .T. ) ;
#15805 = ORIENTED_EDGE ( 'NONE', *, *, #39347, .T. ) ;
#15806 = EDGE_LOOP ( 'NONE', ( #12950, #11329, #35898, #17308 ) ) ;
#15807 = DIRECTION ( 'NONE',  ( -0.000000000000000000, 1.000000000000000000, -0.000000000000000000 ) ) ;
#15808 = LINE ( 'NONE', #8325, #3718 ) ;
#15809 = LINE ( 'NONE', #15568, #40964 ) ;
#15810 = ADVANCED_FACE ( 'NONE', ( #20225 ), #36501, .F. ) ;
#15811 = ORIENTED_EDGE ( 'NONE', *, *, #37187, .T. ) ;
#15812 = ORIENTED_EDGE ( 'NONE', *, *, #27716, .F. ) ;
#15813 = CARTESIAN_POINT ( 'NONE',  ( 0.7117868624172632996, 0.000000000000000000, -1.591464117667681366 ) ) ;
#15814 = CARTESIAN_POINT ( 'NONE',  ( 0.4373159485544403369, 1.722342034578614012, 2.685422482927756427 ) ) ;
#15815 = DIRECTION ( 'NONE',  ( -0.000000000000000000, 1.000000000000000000, -0.000000000000000000 ) ) ;
#15816 = EDGE_CURVE ( 'NONE', #10053, #7713, #23361, .T. ) ;
#15817 = VERTEX_POINT ( 'NONE', #39600 ) ;
#15818 = LINE ( 'NONE', #7826, #45477 ) ;
#15819 = FACE_OUTER_BOUND ( 'NONE', #1422, .T. ) ;
#15820 = ORIENTED_EDGE ( 'NONE', *, *, #8440, .T. ) ;
#15821 = DIRECTION ( 'NONE',  ( -0.000000000000000000, 1.000000000000000000, -0.000000000000000000 ) ) ;
#15822 = ORIENTED_EDGE ( 'NONE', *, *, #11138, .F. ) ;
#15823 = EDGE_LOOP ( 'NONE', ( #19672, #3591, #21340, #29872 ) ) ;
#15824 = CARTESIAN_POINT ( 'NONE',  ( -1.790681247139289889, 1.679220913509628543, -1.240985722462402352 ) ) ;
#15825 = DIRECTION ( 'NONE',  ( 1.000000000000000000, 0.000000000000000000, 0.000000000000000000 ) ) ;
#15827 = VECTOR ( 'NONE', #44703, 39.37007874015748143 ) ;
#15826 = FACE_OUTER_BOUND ( 'NONE', #19001, .T. ) ;
#15828 = ADVANCED_FACE ( 'NONE', ( #24367 ), #40380, .F. ) ;
#15829 = CARTESIAN_POINT ( 'NONE',  ( 0.8182917201112819283, 3.346456692913386100, 0.2755905511810994302 ) ) ;
#15830 = DIRECTION ( 'NONE',  ( -0.01601477604151182663, 0.9998717552508123996, -0.000000000000000000 ) ) ;
#15831 = ORIENTED_EDGE ( 'NONE', *, *, #235, .T. ) ;
#15832 = ORIENTED_EDGE ( 'NONE', *, *, #38457, .T. ) ;
#15833 = VECTOR ( 'NONE', #2811, 39.37007874015748143 ) ;
#15834 = EDGE_CURVE ( 'NONE', #619, #42300, #353, .T. ) ;
#15835 = AXIS2_PLACEMENT_3D ( 'NONE', #16152, #27499, #35770 ) ;
#15836 = ORIENTED_EDGE ( 'NONE', *, *, #15114, .F. ) ;
#15837 = LINE ( 'NONE', #11970, #42590 ) ;
#15838 = PLANE ( 'NONE',  #35008 ) ;
#15839 = DIRECTION ( 'NONE',  ( -3.469446951953613696E-16, 0.000000000000000000, -1.000000000000000000 ) ) ;
#15840 = CARTESIAN_POINT ( 'NONE',  ( -1.942732458483407365, 0.000000000000000000, 2.223636218514596585 ) ) ;
#15841 = ORIENTED_EDGE ( 'NONE', *, *, #50894, .T. ) ;
#15842 = DIRECTION ( 'NONE',  ( -0.000000000000000000, 1.000000000000000000, 0.000000000000000000 ) ) ;
#15843 = EDGE_CURVE ( 'NONE', #43721, #41731, #31866, .T. ) ;
#15844 = DIRECTION ( 'NONE',  ( 0.000000000000000000, 0.000000000000000000, -1.000000000000000000 ) ) ;
#15845 = ORIENTED_EDGE ( 'NONE', *, *, #31089, .F. ) ;
#15846 = CARTESIAN_POINT ( 'NONE',  ( 0.000000000000000000, 3.267716535433071279, 1.692913385826762873 ) ) ;
#15847 = CARTESIAN_POINT ( 'NONE',  ( -1.091055626815042201, 3.267716535433071279, 1.377952755905504256 ) ) ;
#15848 = DIRECTION ( 'NONE',  ( -0.000000000000000000, -1.000000000000000000, -0.000000000000000000 ) ) ;
#15849 = EDGE_LOOP ( 'NONE', ( #31977, #9898, #43007, #42963 ) ) ;
#15850 = CARTESIAN_POINT ( 'NONE',  ( 1.091055626815042423, 3.346456692913386100, -2.086614173228339641 ) ) ;
#15851 = DIRECTION ( 'NONE',  ( -0.000000000000000000, 1.000000000000000000, -0.000000000000000000 ) ) ;
#15852 = B_SPLINE_CURVE_WITH_KNOTS ( 'NONE', 3,
 ( #14812, #50867, #26673, #7064 ),
 .UNSPECIFIED., .F., .F.,
 ( 4, 4 ),
 ( 0.01101059834352955021, 0.03073596030694578790 ),
 .UNSPECIFIED. ) ;
#15853 = CARTESIAN_POINT ( 'NONE',  ( -1.536664496436148184E-16, 3.346456692913386100, -0.8267716535433052849 ) ) ;
#15854 = VERTEX_POINT ( 'NONE', #12235 ) ;
#15855 = CARTESIAN_POINT ( 'NONE',  ( -1.712496953225537188, 0.000000000000000000, -0.1574803149606297248 ) ) ;
#15856 = ORIENTED_EDGE ( 'NONE', *, *, #40681, .T. ) ;
#15857 = DIRECTION ( 'NONE',  ( 0.000000000000000000, -1.000000000000000000, 0.000000000000000000 ) ) ;
#15858 = AXIS2_PLACEMENT_3D ( 'NONE', #13178, #24788, #32546 ) ;
#15859 = DIRECTION ( 'NONE',  ( -3.469446951953613696E-16, 0.000000000000000000, -1.000000000000000000 ) ) ;
#15860 = LINE ( 'NONE', #36011, #48572 ) ;
#15861 = LINE ( 'NONE', #50421, #12806 ) ;
#15862 = CIRCLE ( 'NONE', #50453, 2.165354330708661568 ) ;
#15863 = ORIENTED_EDGE ( 'NONE', *, *, #32373, .F. ) ;
#15864 = ORIENTED_EDGE ( 'NONE', *, *, #28274, .T. ) ;
#15865 = CARTESIAN_POINT ( 'NONE',  ( 1.560669927219590525, 3.346456692913386100, -0.03937007874015908959 ) ) ;
#15866 = CARTESIAN_POINT ( 'NONE',  ( 0.8182917201112822614, 3.267716535433071279, -1.419509857074483785E-16 ) ) ;
#15867 = EDGE_CURVE ( 'NONE', #21112, #9779, #8871, .T. ) ;
#15868 = ORIENTED_EDGE ( 'NONE', *, *, #13434, .F. ) ;
#15869 = VECTOR ( 'NONE', #32353, 39.37007874015748143 ) ;
#15870 = DIRECTION ( 'NONE',  ( -3.469446951953613696E-16, 0.000000000000000000, -1.000000000000000000 ) ) ;
#15871 = FACE_OUTER_BOUND ( 'NONE', #46592, .T. ) ;
#15872 = DIRECTION ( 'NONE',  ( -3.469446951953613696E-16, 0.000000000000000000, -1.000000000000000000 ) ) ;
#15873 = ADVANCED_FACE ( 'NONE', ( #23593 ), #8615, .F. ) ;
#15874 = VECTOR ( 'NONE', #26880, 39.37007874015748143 ) ;
#15875 = CARTESIAN_POINT ( 'NONE',  ( 1.930190994932111215, 1.205361022782829114E-17, -0.9827944786818438860 ) ) ;
#15876 = AXIS2_PLACEMENT_3D ( 'NONE', #25059, #28924, #44660 ) ;
#15877 = ORIENTED_EDGE ( 'NONE', *, *, #46509, .F. ) ;
#15878 = ORIENTED_EDGE ( 'NONE', *, *, #11893, .T. ) ;
#15879 = EDGE_CURVE ( 'NONE', #34103, #49753, #4998, .T. ) ;
#15880 = ORIENTED_EDGE ( 'NONE', *, *, #15184, .F. ) ;
#15881 = PLANE ( 'NONE',  #34058 ) ;
#15882 = FACE_OUTER_BOUND ( 'NONE', #4940, .T. ) ;
#15883 = EDGE_CURVE ( 'NONE', #35559, #47517, #4747, .T. ) ;
#15884 = DIRECTION ( 'NONE',  ( -0.000000000000000000, 0.000000000000000000, 1.000000000000000000 ) ) ;
#15885 = EDGE_LOOP ( 'NONE', ( #33064, #17851, #2880, #16040 ) ) ;
#15886 = CARTESIAN_POINT ( 'NONE',  ( -1.659559921305661101, 0.5251570559280069883, 1.386400150466028158 ) ) ;
#15887 = ORIENTED_EDGE ( 'NONE', *, *, #44796, .T. ) ;
#15888 = ORIENTED_EDGE ( 'NONE', *, *, #48885, .T. ) ;
#15889 = CARTESIAN_POINT ( 'NONE',  ( 0.000000000000000000, 3.267716535433071279, 0.3149606299212577287 ) ) ;
#15890 = ADVANCED_FACE ( 'NONE', ( #20490 ), #1968, .T. ) ;
#15891 = VERTEX_POINT ( 'NONE', #47302 ) ;
#15892 = VERTEX_POINT ( 'NONE', #32124 ) ;
#15893 = DIRECTION ( 'NONE',  ( -0.000000000000000000, 1.000000000000000000, -0.000000000000000000 ) ) ;
#15894 = ORIENTED_EDGE ( 'NONE', *, *, #14784, .F. ) ;
#15895 = DIMENSIONAL_EXPONENTS ( 1.000000000000000000, 0.000000000000000000, 0.000000000000000000, 0.000000000000000000, 0.000000000000000000, 0.000000000000000000, 0.000000000000000000 ) ;
#15896 = EDGE_CURVE ( 'NONE', #19400, #15497, #43135, .T. ) ;
#15897 = CARTESIAN_POINT ( 'NONE',  ( 1.833433833923350909, 3.346456692913386100, 1.152076279655074087 ) ) ;
#15898 = CARTESIAN_POINT ( 'NONE',  ( 0.3491433680425106156, 0.5228997897064754374, 2.199551517448510740 ) ) ;
#15899 = CARTESIAN_POINT ( 'NONE',  ( -1.613060539954027872, 1.682065834201676324, -1.474157253483306507 ) ) ;
#15900 = ADVANCED_FACE ( 'NONE', ( #3983 ), #16626, .T. ) ;
#15901 = DIRECTION ( 'NONE',  ( 0.000000000000000000, 1.000000000000000000, 0.000000000000000000 ) ) ;
#15902 = VECTOR ( 'NONE', #42174, 39.37007874015748143 ) ;
#15903 = CARTESIAN_POINT ( 'NONE',  ( -1.636583440222564301, 3.346456692913386100, -0.6299212598425177889 ) ) ;
#15904 = DIRECTION ( 'NONE',  ( 1.000000000000000000, 0.000000000000000000, 0.000000000000000000 ) ) ;
#15905 = EDGE_LOOP ( 'NONE', ( #5074, #8339, #12020, #1918 ) ) ;
#15906 = CARTESIAN_POINT ( 'NONE',  ( 1.325491792074623643, 1.485765544018708750, -2.638988599164732385 ) ) ;
#15907 = DIRECTION ( 'NONE',  ( 1.000000000000000000, 0.000000000000000000, -3.469446951953613696E-16 ) ) ;
#15908 = EDGE_CURVE ( 'NONE', #31838, #8862, #32640, .T. ) ;
#15909 = FACE_OUTER_BOUND ( 'NONE', #39208, .T. ) ;
#15910 = VECTOR ( 'NONE', #18324, 39.37007874015748143 ) ;
#15911 = VECTOR ( 'NONE', #42077, 39.37007874015748143 ) ;
#15912 = EDGE_LOOP ( 'NONE', ( #5691, #12947, #43049, #24065 ) ) ;
#15913 = CARTESIAN_POINT ( 'NONE',  ( 1.191741137761282321, 0.03104109646116221324, -1.556565482633349928 ) ) ;
#15914 = CARTESIAN_POINT ( 'NONE',  ( 1.325491792074623643, 0.000000000000000000, -2.638988599164732385 ) ) ;
#15915 = ORIENTED_EDGE ( 'NONE', *, *, #29590, .F. ) ;
#15916 = DIRECTION ( 'NONE',  ( -3.469446951953613696E-16, 0.000000000000000000, -1.000000000000000000 ) ) ;
#15917 = CARTESIAN_POINT ( 'NONE',  ( -1.076323050859473884, 0.5246904699002969963, 1.897411179605189790 ) ) ;
#15918 = CARTESIAN_POINT ( 'NONE',  ( -1.695772546416001836, 1.594396608463251486, -2.417756147381374010 ) ) ;
#15919 = VECTOR ( 'NONE', #19521, 39.37007874015748143 ) ;
#15920 = EDGE_CURVE ( 'NONE', #12848, #28528, #11721, .T. ) ;
#15921 = CARTESIAN_POINT ( 'NONE',  ( 0.04921259842519689481, 1.205361022782829114E-17, 1.934165248549660987 ) ) ;
#15922 = ORIENTED_EDGE ( 'NONE', *, *, #18628, .T. ) ;
#15923 = LINE ( 'NONE', #47382, #32216 ) ;
#15924 = EDGE_CURVE ( 'NONE', #36052, #32045, #17637, .T. ) ;
#15925 = LINE ( 'NONE', #4066, #29181 ) ;
#15926 = DIRECTION ( 'NONE',  ( -0.7071067811865483499, 0.7071067811865466846, 8.177564888978005264E-17 ) ) ;
#15927 = DIRECTION ( 'NONE',  ( 1.000000000000000000, 0.000000000000000000, -3.469446951953613696E-16 ) ) ;
#15928 = ORIENTED_EDGE ( 'NONE', *, *, #6860, .T. ) ;
#15929 = ORIENTED_EDGE ( 'NONE', *, *, #9724, .T. ) ;
#15930 = ORIENTED_EDGE ( 'NONE', *, *, #27422, .F. ) ;
#15931 = CARTESIAN_POINT ( 'NONE',  ( 0.000000000000000000, 1.172985819482486924, -0.9842519685039369248 ) ) ;
#15932 = ORIENTED_EDGE ( 'NONE', *, *, #28067, .F. ) ;
#15933 = CARTESIAN_POINT ( 'NONE',  ( 4.821444091131312140E-17, 10.31496062992126284, 0.3937007874015748254 ) ) ;
#15934 = DIRECTION ( 'NONE',  ( -0.000000000000000000, 0.000000000000000000, 1.000000000000000000 ) ) ;
#15935 = ORIENTED_EDGE ( 'NONE', *, *, #47947, .T. ) ;
#15936 = EDGE_CURVE ( 'NONE', #38951, #1805, #3578, .T. ) ;
#15937 = LINE ( 'NONE', #31698, #18979 ) ;
#15938 = ORIENTED_EDGE ( 'NONE', *, *, #49366, .F. ) ;
#15939 = CARTESIAN_POINT ( 'NONE',  ( 2.106197740627111514, 3.346456692913386100, -1.102362204724406602 ) ) ;
#15940 = EDGE_CURVE ( 'NONE', #6661, #25341, #45483, .T. ) ;
#15941 = VECTOR ( 'NONE', #13680, 39.37007874015748143 ) ;
#15942 = CARTESIAN_POINT ( 'NONE',  ( 1.520337605863835151, 3.240842057052200964, -1.929133858267710666 ) ) ;
#15943 = EDGE_LOOP ( 'NONE', ( #14350, #22266, #5007, #18645 ) ) ;
#15944 = ORIENTED_EDGE ( 'NONE', *, *, #8855, .F. ) ;
#15945 = DIRECTION ( 'NONE',  ( -1.000000000000000000, 0.000000000000000000, -0.000000000000000000 ) ) ;
#15946 = AXIS2_PLACEMENT_3D ( 'NONE', #2482, #34232, #14093 ) ;
#15947 = ORIENTED_EDGE ( 'NONE', *, *, #4932, .F. ) ;
#15948 = VECTOR ( 'NONE', #4011, 39.37007874015748143 ) ;
#15949 = VECTOR ( 'NONE', #866, 39.37007874015748143 ) ;
#15950 = CARTESIAN_POINT ( 'NONE',  ( 1.560669927219590303, 3.267716535433071279, -1.880327210325009046 ) ) ;
#15951 = ORIENTED_EDGE ( 'NONE', *, *, #40246, .T. ) ;
#15952 = VERTEX_POINT ( 'NONE', #1379 ) ;
#15953 = ADVANCED_FACE ( 'NONE', ( #6276 ), #13768, .F. ) ;
#15954 = DIRECTION ( 'NONE',  ( 1.776356839400250149E-14, 0.000000000000000000, 1.000000000000000000 ) ) ;
#15955 = AXIS2_PLACEMENT_3D ( 'NONE', #41960, #26708, #38099 ) ;
#15956 = CARTESIAN_POINT ( 'NONE',  ( -0.04921259842519701277, 1.049866565877818125, 2.024102350102944037 ) ) ;
#15957 = ORIENTED_EDGE ( 'NONE', *, *, #14318, .F. ) ;
#15958 = DIRECTION ( 'NONE',  ( -0.01601477604151182663, 0.9998717552508123996, -0.000000000000000000 ) ) ;
#15959 = ORIENTED_EDGE ( 'NONE', *, *, #1372, .F. ) ;
#15960 = PLANE ( 'NONE',  #45849 ) ;
#15961 = CARTESIAN_POINT ( 'NONE',  ( -1.636583440222563635, 3.267716535433071279, 0.7480314960629874665 ) ) ;
#15962 = EDGE_CURVE ( 'NONE', #46993, #33556, #29513, .T. ) ;
#15963 = LINE ( 'NONE', #47677, #13196 ) ;
#15964 = ORIENTED_EDGE ( 'NONE', *, *, #42397, .T. ) ;
#15965 = ORIENTED_EDGE ( 'NONE', *, *, #37937, .F. ) ;
#15966 = LINE ( 'NONE', #43326, #8796 ) ;
#15967 = FACE_OUTER_BOUND ( 'NONE', #28315, .T. ) ;
#15968 = FACE_OUTER_BOUND ( 'NONE', #29193, .T. ) ;
#15969 = DIRECTION ( 'NONE',  ( 1.000000000000000000, -0.000000000000000000, 0.000000000000000000 ) ) ;
#15970 = EDGE_CURVE ( 'NONE', #45742, #38443, #41452, .T. ) ;
#15971 = LINE ( 'NONE', #5124, #44570 ) ;
#15972 = EDGE_CURVE ( 'NONE', #32098, #43573, #22027, .T. ) ;
#15973 = LINE ( 'NONE', #32249, #41644 ) ;
#15974 = ORIENTED_EDGE ( 'NONE', *, *, #16125, .F. ) ;
#15975 = EDGE_CURVE ( 'NONE', #27834, #38248, #9895, .T. ) ;
#15976 = B_SPLINE_CURVE_WITH_KNOTS ( 'NONE', 3,
 ( #23075, #46533, #30572, #50631 ),
 .UNSPECIFIED., .F., .F.,
 ( 4, 4 ),
 ( 3.552899504225758744E-07, 0.04838472165043559980 ),
 .UNSPECIFIED. ) ;
#15977 = DIRECTION ( 'NONE',  ( -1.118904554427325505E-16, -1.000000000000000000, 3.087980359898369198E-17 ) ) ;
#15978 = AXIS2_PLACEMENT_3D ( 'NONE', #45036, #37829, #18193 ) ;
#15979 = VERTEX_POINT ( 'NONE', #17894 ) ;
#15980 = CARTESIAN_POINT ( 'NONE',  ( 0.002207914879453961969, 5.905511811023623991, 0.04916304461325442243 ) ) ;
#15981 = AXIS2_PLACEMENT_3D ( 'NONE', #8165, #23907, #39658 ) ;
#15982 = ADVANCED_FACE ( 'NONE', ( #48830 ), #25634, .T. ) ;
#15983 = AXIS2_PLACEMENT_3D ( 'NONE', #40258, #40766, #4883 ) ;
#15984 = ORIENTED_EDGE ( 'NONE', *, *, #27488, .F. ) ;
#15985 = AXIS2_PLACEMENT_3D ( 'NONE', #8628, #3737, #39613 ) ;
#15987 = AXIS2_PLACEMENT_3D ( 'NONE', #43132, #549, #43391 ) ;
#15986 = CARTESIAN_POINT ( 'NONE',  ( 0.4506430153629077950, 0.03513753811042658048, -1.817852439337431569 ) ) ;
#15988 = DIRECTION ( 'NONE',  ( 1.000000000000000000, 0.000000000000000000, 0.000000000000000000 ) ) ;
#15989 = CARTESIAN_POINT ( 'NONE',  ( -2.455254038445241704, 1.582553845862669784, -1.640354883688478038 ) ) ;
#15990 = ORIENTED_EDGE ( 'NONE', *, *, #48206, .F. ) ;
#15991 = VECTOR ( 'NONE', #16300, 39.37007874015748143 ) ;
#15992 = CARTESIAN_POINT ( 'NONE',  ( 0.8451757313534469240, 1.655822191538975918, 2.111905413333155401 ) ) ;
#15993 = ORIENTED_EDGE ( 'NONE', *, *, #43708, .F. ) ;
#15994 = DIRECTION ( 'NONE',  ( -0.000000000000000000, 1.000000000000000000, -0.000000000000000000 ) ) ;
#15995 = EDGE_LOOP ( 'NONE', ( #10346, #19563, #9988, #40840 ) ) ;
#15996 = EDGE_CURVE ( 'NONE', #15197, #17350, #22565, .T. ) ;
#15997 = LINE ( 'NONE', #4131, #40916 ) ;
#15998 = CARTESIAN_POINT ( 'NONE',  ( -1.202103464817552592, 0.5249316475426857309, 1.450716273920663824 ) ) ;
#15999 = EDGE_CURVE ( 'NONE', #6103, #36932, #21509, .T. ) ;
#16000 = ORIENTED_EDGE ( 'NONE', *, *, #4406, .T. ) ;
#16001 = CARTESIAN_POINT ( 'NONE',  ( 2.182111253630085290, 3.346456692913386100, -0.3149606299212596716 ) ) ;
#16002 = EDGE_CURVE ( 'NONE', #5956, #14009, #37524, .T. ) ;
#16003 = ORIENTED_EDGE ( 'NONE', *, *, #29109, .F. ) ;
#16004 = VERTEX_POINT ( 'NONE', #49344 ) ;
#16005 = DIRECTION ( 'NONE',  ( -0.000000000000000000, 1.000000000000000000, -0.000000000000000000 ) ) ;
#16006 = LINE ( 'NONE', #31764, #10029 ) ;
#16007 = CARTESIAN_POINT ( 'NONE',  ( 0.5455278134075217666, 3.267716535433071279, 2.204724409448808764 ) ) ;
#16008 = ORIENTED_EDGE ( 'NONE', *, *, #30209, .T. ) ;
#16009 = CARTESIAN_POINT ( 'NONE',  ( -0.8182917201112819283, 0.000000000000000000, -1.299212598425193210 ) ) ;
#16010 = DIRECTION ( 'NONE',  ( -0.000000000000000000, -1.000000000000000000, -0.000000000000000000 ) ) ;
#16011 = ORIENTED_EDGE ( 'NONE', *, *, #29953, .F. ) ;
#16012 = CARTESIAN_POINT ( 'NONE',  ( 0.4696143004045479352, 3.267716535433071279, 0.4724409448818868706 ) ) ;
#16013 =( GEOMETRIC_REPRESENTATION_CONTEXT ( 3 ) GLOBAL_UNCERTAINTY_ASSIGNED_CONTEXT ( ( #9178 ) ) GLOBAL_UNIT_ASSIGNED_CONTEXT ( ( #50817, #2887, #34633 ) ) REPRESENTATION_CONTEXT ( 'NONE', 'WORKASPACE' ) );
#16014 = VECTOR ( 'NONE', #22019, 39.37007874015748143 ) ;
#16015 = EDGE_LOOP ( 'NONE', ( #19407, #24069, #12023, #4155, #46929, #34101, #33587, #2893, #41249, #6371, #11399, #31648, #45473 ) ) ;
#16016 = CIRCLE ( 'NONE', #44865, 0.3937007874015748254 ) ;
#16017 = ORIENTED_EDGE ( 'NONE', *, *, #42499, .T. ) ;
#16018 = SHAPE_DEFINITION_REPRESENTATION ( #12912, #34429 ) ;
#16019 = AXIS2_PLACEMENT_3D ( 'NONE', #21147, #48215, #20883 ) ;
#16020 = ORIENTED_EDGE ( 'NONE', *, *, #43768, .T. ) ;
#16021 = CARTESIAN_POINT ( 'NONE',  ( -0.7148041136150271591, 6.692913385826772199, -2.044646019095620382 ) ) ;
#16022 = VECTOR ( 'NONE', #44606, 39.37007874015748143 ) ;
#16023 = PLANE ( 'NONE',  #6859 ) ;
#16024 = CYLINDRICAL_SURFACE ( 'NONE', #41570, 0.3937007874015748254 ) ;
#16025 = CARTESIAN_POINT ( 'NONE',  ( 0.4696143004045478797, 3.346456692913386100, -0.03937007874015908959 ) ) ;
#16026 = ORIENTED_EDGE ( 'NONE', *, *, #39666, .T. ) ;
#16027 = ORIENTED_EDGE ( 'NONE', *, *, #41186, .F. ) ;
#16028 = AXIS2_PLACEMENT_3D ( 'NONE', #11232, #29650, #30602 ) ;
#16029 = LENGTH_MEASURE_WITH_UNIT ( LENGTH_MEASURE( 0.02539999999999999897 ), #23262 );
#16030 = DIRECTION ( 'NONE',  ( -6.104789737168038204E-17, 1.000000000000000000, -1.134460028949771622E-16 ) ) ;
#16031 = B_SPLINE_CURVE_WITH_KNOTS ( 'NONE', 3,
 ( #24236, #32241, #13129, #29114 ),
 .UNSPECIFIED., .F., .F.,
 ( 4, 4 ),
 ( 2.894122015862211124E-07, 0.01950060374906107188 ),
 .UNSPECIFIED. ) ;
#16032 = VERTEX_POINT ( 'NONE', #48327 ) ;
#16033 = DIRECTION ( 'NONE',  ( 0.5508969814521065267, 9.684980370528620210E-17, -0.8345732537212999791 ) ) ;
#16034 = DIRECTION ( 'NONE',  ( -3.469446951953613696E-16, 0.000000000000000000, -1.000000000000000000 ) ) ;
#16035 = EDGE_CURVE ( 'NONE', #27306, #38137, #29250, .T. ) ;
#16036 = EDGE_CURVE ( 'NONE', #40614, #42095, #5764, .T. ) ;
#16037 = CARTESIAN_POINT ( 'NONE',  ( -0.3486774197067338266, 3.267716535433071279, 1.209717811016578585E-16 ) ) ;
#16038 = EDGE_CURVE ( 'NONE', #45493, #13751, #13007, .T. ) ;
#16039 = LINE ( 'NONE', #19386, #33547 ) ;
#16040 = ORIENTED_EDGE ( 'NONE', *, *, #20932, .T. ) ;
#16041 = CARTESIAN_POINT ( 'NONE',  ( -0.8182917201112819283, 0.000000000000000000, 0.1574803149606285035 ) ) ;
#16042 = LINE ( 'NONE', #16817, #16992 ) ;
#16043 = ORIENTED_EDGE ( 'NONE', *, *, #32959, .T. ) ;
#16044 = ORIENTED_EDGE ( 'NONE', *, *, #46632, .T. ) ;
#16045 = LINE ( 'NONE', #20160, #47943 ) ;
#16046 = CARTESIAN_POINT ( 'NONE',  ( -1.909347346926324906, 3.267716535433071279, -0.4724409448818884805 ) ) ;
#16047 = DIRECTION ( 'NONE',  ( -3.469446951953613696E-16, 0.000000000000000000, -1.000000000000000000 ) ) ;
#16048 = ORIENTED_EDGE ( 'NONE', *, *, #40143, .T. ) ;
#16049 = VECTOR ( 'NONE', #47686, 39.37007874015748854 ) ;
#16050 = VERTEX_POINT ( 'NONE', #9124 ) ;
#16051 = AXIS2_PLACEMENT_3D ( 'NONE', #39524, #38769, #3653 ) ;
#16052 = FACE_OUTER_BOUND ( 'NONE', #47264, .T. ) ;
#16054 = VERTEX_POINT ( 'NONE', #36757 ) ;
#16053 = EDGE_CURVE ( 'NONE', #42475, #40629, #24878, .T. ) ;
#16055 = DIRECTION ( 'NONE',  ( -1.000000000000000000, -0.000000000000000000, -0.000000000000000000 ) ) ;
#16056 = VECTOR ( 'NONE', #47833, 39.37007874015748143 ) ;
#16057 = EDGE_LOOP ( 'NONE', ( #39133, #40809, #8794, #20164 ) ) ;
#16058 = CARTESIAN_POINT ( 'NONE',  ( -0.2727639067037607723, 0.000000000000000000, -0.1574803149606301411 ) ) ;
#16059 = EDGE_CURVE ( 'NONE', #28931, #3036, #32900, .T. ) ;
#16060 = LINE ( 'NONE', #27161, #36277 ) ;
#16061 = CARTESIAN_POINT ( 'NONE',  ( 0.1968503937007878568, 3.346456692913386100, 1.889763779527550369 ) ) ;
#16062 = EDGE_CURVE ( 'NONE', #2854, #10877, #25129, .T. ) ;
#16063 = ORIENTED_EDGE ( 'NONE', *, *, #39951, .T. ) ;
#16064 = ORIENTED_EDGE ( 'NONE', *, *, #31922, .T. ) ;
#16065 = ORIENTED_EDGE ( 'NONE', *, *, #22656, .T. ) ;
#16066 = DIRECTION ( 'NONE',  ( -0.000000000000000000, 1.000000000000000000, -0.000000000000000000 ) ) ;
#16067 = AXIS2_PLACEMENT_3D ( 'NONE', #15263, #34885, #50568 ) ;
#16068 = CARTESIAN_POINT ( 'NONE',  ( 0.08119777152254364916, 1.623385212329073957, 0.000000000000000000 ) ) ;
#16070 = ORIENTED_EDGE ( 'NONE', *, *, #691, .F. ) ;
#16069 = ADVANCED_FACE ( 'NONE', ( #45736 ), #22783, .F. ) ;
#16071 = ORIENTED_EDGE ( 'NONE', *, *, #2845, .F. ) ;
#16072 = CARTESIAN_POINT ( 'NONE',  ( -1.093343507848659524, 0.007001814219102117827, -1.421132763804449306 ) ) ;
#16073 = DIRECTION ( 'NONE',  ( 1.000000000000000000, -0.000000000000000000, 0.000000000000000000 ) ) ;
#16074 = CARTESIAN_POINT ( 'NONE',  ( -0.7148041136150268260, 5.905511811023623991, -2.044646019095619938 ) ) ;
#16075 = ORIENTED_EDGE ( 'NONE', *, *, #30650, .F. ) ;
#16076 = VERTEX_POINT ( 'NONE', #46241 ) ;
#16077 = PLANE ( 'NONE',  #43576 ) ;
#16078 = LINE ( 'NONE', #16336, #1912 ) ;
#16079 = CARTESIAN_POINT ( 'NONE',  ( 1.636583440222563635, 3.346456692913386100, -1.259842519685035800 ) ) ;
#16080 = ORIENTED_EDGE ( 'NONE', *, *, #16782, .T. ) ;
#16081 = B_SPLINE_CURVE_WITH_KNOTS ( 'NONE', 3,
 ( #41804, #26803, #37941, #42053 ),
 .UNSPECIFIED., .F., .F.,
 ( 4, 4 ),
 ( 2.008389287922521166E-07, 0.01785224886139480382 ),
 .UNSPECIFIED. ) ;
#16082 = FACE_OUTER_BOUND ( 'NONE', #16923, .T. ) ;
#16083 = CARTESIAN_POINT ( 'NONE',  ( -0.5455278134075214336, 0.000000000000000000, -1.456692913385822630 ) ) ;
#16084 = VERTEX_POINT ( 'NONE', #11155 ) ;
#16085 = CARTESIAN_POINT ( 'NONE',  ( 0.7423782071083085965, 3.346456692913386100, -0.8267716535433055070 ) ) ;
#16086 = ORIENTED_EDGE ( 'NONE', *, *, #16320, .T. ) ;
#16087 = ORIENTED_EDGE ( 'NONE', *, *, #5644, .T. ) ;
#16088 = CARTESIAN_POINT ( 'NONE',  ( 1.139183960333101098, 3.267716535433071279, -1.771653543307081691 ) ) ;
#16089 = SHAPE_REPRESENTATION_RELATIONSHIP ( 'NONE' , 'NONE' ,  #15265, #18129 ) ;
#16090 = CARTESIAN_POINT ( 'NONE',  ( 0.1968503937007878568, 0.000000000000000000, 1.259842519685033357 ) ) ;
#16091 = CARTESIAN_POINT ( 'NONE',  ( 1.902660579019252562, 1.639951345248664039, -1.314902632263422966 ) ) ;
#16092 = CARTESIAN_POINT ( 'NONE',  ( 1.636583440222563857, 3.267716535433071279, -2.839019714148966584E-16 ) ) ;
#16093 = EDGE_LOOP ( 'NONE', ( #8073, #35046, #44492, #23777 ) ) ;
#16094 = ORIENTED_EDGE ( 'NONE', *, *, #27462, .F. ) ;
#16095 = AXIS2_PLACEMENT_3D ( 'NONE', #18017, #45605, #22648 ) ;
#16096 = AXIS2_PLACEMENT_3D ( 'NONE', #16702, #28303, #32197 ) ;
#16097 = AXIS2_PLACEMENT_3D ( 'NONE', #11595, #15722, #27333 ) ;
#16098 = EDGE_LOOP ( 'NONE', ( #5861, #28246, #12985, #19751 ) ) ;
#16099 = LINE ( 'NONE', #27966, #11272 ) ;
#16100 = CARTESIAN_POINT ( 'NONE',  ( -1.091055626815042645, 3.346456692913386100, -0.1968503937007881899 ) ) ;
#16101 = VECTOR ( 'NONE', #42098, 39.37007874015748143 ) ;
#16102 = EDGE_CURVE ( 'NONE', #3556, #49445, #50098, .T. ) ;
#16103 = DIRECTION ( 'NONE',  ( 0.000000000000000000, 1.160734090543304660E-16, -1.000000000000000000 ) ) ;
#16104 = PLANE ( 'NONE',  #50042 ) ;
#16105 = AXIS2_PLACEMENT_3D ( 'NONE', #11496, #31119, #7618 ) ;
#16106 = ORIENTED_EDGE ( 'NONE', *, *, #44701, .F. ) ;
#16107 = EDGE_CURVE ( 'NONE', #2753, #25164, #39030, .T. ) ;
#16108 = CARTESIAN_POINT ( 'NONE',  ( -0.8949303405208601792, 6.692913385826772199, -1.971765468592543202 ) ) ;
#16109 = DIRECTION ( 'NONE',  ( -0.7818314824680221431, 0.000000000000000000, -0.6234898018587431423 ) ) ;
#16110 = EDGE_CURVE ( 'NONE', #10637, #48582, #38533, .T. ) ;
#16111 = ORIENTED_EDGE ( 'NONE', *, *, #41006, .F. ) ;
#16112 = PLANE ( 'NONE',  #12490 ) ;
#16113 = FACE_OUTER_BOUND ( 'NONE', #4210, .T. ) ;
#16114 = LINE ( 'NONE', #5255, #31258 ) ;
#16115 = ORIENTED_EDGE ( 'NONE', *, *, #10997, .T. ) ;
#16116 = CARTESIAN_POINT ( 'NONE',  ( 0.8182917201112824834, 0.000000000000000000, 2.047244094488179567 ) ) ;
#16117 = DIRECTION ( 'NONE',  ( 1.000000000000000000, 0.000000000000000000, 0.000000000000000000 ) ) ;
#16118 = PLANE ( 'NONE',  #15985 ) ;
#16119 = ORIENTED_EDGE ( 'NONE', *, *, #50720, .T. ) ;
#16120 = CARTESIAN_POINT ( 'NONE',  ( 1.091055626815042423, 3.346456692913386100, -1.889763779527552368 ) ) ;
#16121 = CARTESIAN_POINT ( 'NONE',  ( -0.5455278134075214336, 0.000000000000000000, -1.259842519685035134 ) ) ;
#16122 = EDGE_LOOP ( 'NONE', ( #2291, #9685, #42177, #35618 ) ) ;
#16123 = LINE ( 'NONE', #4506, #652 ) ;
#16124 = CARTESIAN_POINT ( 'NONE',  ( 0.1968503937007878568, 0.000000000000000000, 0.9448818897637749625 ) ) ;
#16125 = EDGE_CURVE ( 'NONE', #18551, #47200, #27146, .T. ) ;
#16126 = CARTESIAN_POINT ( 'NONE',  ( 1.636583440222563857, 3.267716535433071279, -2.839019714148966584E-16 ) ) ;
#16127 = LINE ( 'NONE', #21025, #7046 ) ;
#16128 = ORIENTED_EDGE ( 'NONE', *, *, #11323, .T. ) ;
#16129 = ORIENTED_EDGE ( 'NONE', *, *, #35985, .F. ) ;
#16130 = PLANE ( 'NONE',  #3420 ) ;
#16131 = CONICAL_SURFACE ( 'NONE', #9540, 2.244934639244524632, 1.554780866114618743 ) ;
#16132 = CARTESIAN_POINT ( 'NONE',  ( 1.836342932631641167, 0.000000000000000000, 1.044063857347276469 ) ) ;
#16133 = VECTOR ( 'NONE', #46318, 39.37007874015748143 ) ;
#16134 = ADVANCED_FACE ( 'NONE', ( #15282 ), #42886, .F. ) ;
#16135 = ORIENTED_EDGE ( 'NONE', *, *, #34832, .F. ) ;
#16136 = CARTESIAN_POINT ( 'NONE',  ( 1.305557278495039775, 1.728812839972934334, -1.880670907523083191 ) ) ;
#16137 = DIRECTION ( 'NONE',  ( -3.469446951953613696E-16, 0.000000000000000000, -1.000000000000000000 ) ) ;
#16138 = DIRECTION ( 'NONE',  ( 1.734723475976806848E-16, -0.000000000000000000, 1.000000000000000000 ) ) ;
#16139 = B_SPLINE_CURVE_WITH_KNOTS ( 'NONE', 3,
 ( #39656, #2894, #32955, #29312 ),
 .UNSPECIFIED., .F., .F.,
 ( 4, 4 ),
 ( 0.1211775127643062444, 0.1625894504277921315 ),
 .UNSPECIFIED. ) ;
#16140 = AXIS2_PLACEMENT_3D ( 'NONE', #47706, #7740, #35115 ) ;
#16141 = LINE ( 'NONE', #16399, #33919 ) ;
#16142 = VERTEX_POINT ( 'NONE', #10659 ) ;
#16143 = VERTEX_POINT ( 'NONE', #14530 ) ;
#16144 = VERTEX_POINT ( 'NONE', #6778 ) ;
#16145 = DIRECTION ( 'NONE',  ( -0.01601477604151182663, 0.9998717552508123996, -0.000000000000000000 ) ) ;
#16146 = VECTOR ( 'NONE', #6055, 39.37007874015748143 ) ;
#16147 = DIRECTION ( 'NONE',  ( 0.9195277725514544587, 0.000000000000000000, -0.3930250316539147803 ) ) ;
#16148 = LINE ( 'NONE', #31908, #47079 ) ;
#16150 = AXIS2_PLACEMENT_3D ( 'NONE', #34805, #34311, #46391 ) ;
#16149 = FACE_BOUND ( 'NONE', #41005, .T. ) ;
#16151 = ORIENTED_EDGE ( 'NONE', *, *, #50160, .F. ) ;
#16152 = CARTESIAN_POINT ( 'NONE',  ( -2.182111253630085290, 0.000000000000000000, 0.1181102362204704270 ) ) ;
#16153 = EDGE_LOOP ( 'NONE', ( #6822, #19662, #30290, #30422, #13804 ) ) ;
#16154 = ORIENTED_EDGE ( 'NONE', *, *, #36448, .F. ) ;
#16155 = CARTESIAN_POINT ( 'NONE',  ( 0.002207914879453961969, 5.905511811023623991, 0.04916304461325442243 ) ) ;
#16156 = VERTEX_POINT ( 'NONE', #7534 ) ;
#16157 = EDGE_LOOP ( 'NONE', ( #16734, #7165, #35816, #1470 ) ) ;
#16158 = DIRECTION ( 'NONE',  ( -1.045785279492548401E-16, -1.000000000000000000, 5.036236473261409814E-17 ) ) ;
#16159 = ORIENTED_EDGE ( 'NONE', *, *, #15438, .T. ) ;
#16160 = FACE_OUTER_BOUND ( 'NONE', #6013, .T. ) ;
#16161 = DIRECTION ( 'NONE',  ( -0.08963930890342654279, 0.000000000000000000, -0.9959742939952397345 ) ) ;
#16162 = LINE ( 'NONE', #32435, #39091 ) ;
#16163 = VECTOR ( 'NONE', #32056, 39.37007874015748143 ) ;
#16164 = DIRECTION ( 'NONE',  ( -3.469446951953613696E-16, 0.000000000000000000, -1.000000000000000000 ) ) ;
#16165 = EDGE_CURVE ( 'NONE', #17400, #34114, #11408, .T. ) ;
#16166 = CARTESIAN_POINT ( 'NONE',  ( -0.8942052331142552601, 0.000000000000000000, -7.512581982576723358E-16 ) ) ;
#16167 = DIRECTION ( 'NONE',  ( 1.000000000000000000, -0.000000000000000000, 0.000000000000000000 ) ) ;
#16168 = VECTOR ( 'NONE', #9641, 39.37007874015748143 ) ;
#16169 = ORIENTED_EDGE ( 'NONE', *, *, #49969, .T. ) ;
#16170 = ADVANCED_FACE ( 'NONE', ( #23274 ), #3661, .F. ) ;
#16171 = PLANE ( 'NONE',  #16748 ) ;
#16172 = VECTOR ( 'NONE', #48690, 39.37007874015748143 ) ;
#16173 = DIRECTION ( 'NONE',  ( -3.469446951953613696E-16, 0.000000000000000000, -1.000000000000000000 ) ) ;
#16174 = VECTOR ( 'NONE', #36466, 39.37007874015748143 ) ;
#16175 = DIRECTION ( 'NONE',  ( -0.9998717552508122886, -0.01601477604151182316, 0.000000000000000000 ) ) ;
#16176 = EDGE_CURVE ( 'NONE', #41557, #37198, #18402, .T. ) ;
#16177 = ORIENTED_EDGE ( 'NONE', *, *, #14726, .F. ) ;
#16178 = CARTESIAN_POINT ( 'NONE',  ( 1.363819533518803251, 0.000000000000000000, 0.1574803149606283648 ) ) ;
#16179 = EDGE_CURVE ( 'NONE', #3361, #44517, #26395, .T. ) ;
#16180 = CARTESIAN_POINT ( 'NONE',  ( 1.034308760555261886, 1.626043101691516890, -2.034340803895991812 ) ) ;
#16181 = ORIENTED_EDGE ( 'NONE', *, *, #10579, .T. ) ;
#16182 = FACE_OUTER_BOUND ( 'NONE', #12366, .T. ) ;
#16183 = VECTOR ( 'NONE', #29995, 39.37007874015748143 ) ;
#16184 = EDGE_CURVE ( 'NONE', #30042, #49974, #18660, .T. ) ;
#16185 = LINE ( 'NONE', #17455, #17615 ) ;
#16186 = DIRECTION ( 'NONE',  ( -0.9998717552508122886, -0.01601477604151185785, 0.000000000000000000 ) ) ;
#16187 = VECTOR ( 'NONE', #47651, 39.37007874015748143 ) ;
#16188 = CARTESIAN_POINT ( 'NONE',  ( -1.500342777408262496, 0.001329947905571405567, -0.9314002160103560524 ) ) ;
#16189 = ORIENTED_EDGE ( 'NONE', *, *, #28916, .T. ) ;
#16190 = CARTESIAN_POINT ( 'NONE',  ( 2.305855796294430160, 1.748229977355783005, -1.039089491665910359 ) ) ;
#16191 = LINE ( 'NONE', #38673, #1992 ) ;
#16192 = CARTESIAN_POINT ( 'NONE',  ( 0.5455278134075216556, 0.000000000000000000, 2.007874015748021268 ) ) ;
#16193 = EDGE_CURVE ( 'NONE', #17447, #48287, #22278, .T. ) ;
#16194 = PLANE ( 'NONE',  #30928 ) ;
#16195 = VERTEX_POINT ( 'NONE', #15031 ) ;
#16196 = ORIENTED_EDGE ( 'NONE', *, *, #12340, .T. ) ;
#16197 = CARTESIAN_POINT ( 'NONE',  ( 0.000000000000000000, 3.267716535433071279, 1.535433070866133232 ) ) ;
#16198 = ORIENTED_EDGE ( 'NONE', *, *, #44567, .F. ) ;
#16199 = EDGE_CURVE ( 'NONE', #44259, #21303, #35327, .T. ) ;
#16200 = DIRECTION ( 'NONE',  ( -1.000000000000000000, 0.000000000000000000, 1.734723475976806848E-16 ) ) ;
#16201 = EDGE_LOOP ( 'NONE', ( #18273, #36802, #44339, #34799 ) ) ;
#16202 = FACE_OUTER_BOUND ( 'NONE', #17933, .T. ) ;
#16203 = VERTEX_POINT ( 'NONE', #46490 ) ;
#16204 = ADVANCED_FACE ( 'NONE', ( #30276 ), #49591, .F. ) ;
#16205 = CARTESIAN_POINT ( 'NONE',  ( 0.000000000000000000, 3.346456692913386100, 0.000000000000000000 ) ) ;
#16206 = VECTOR ( 'NONE', #26275, 39.37007874015748143 ) ;
#16207 = FACE_OUTER_BOUND ( 'NONE', #44739, .T. ) ;
#16208 = VECTOR ( 'NONE', #38228, 39.37007874015748143 ) ;
#16209 = EDGE_LOOP ( 'NONE', ( #45195, #19747, #11897, #32402 ) ) ;
#16210 = VECTOR ( 'NONE', #28472, 39.37007874015748143 ) ;
#16211 = CARTESIAN_POINT ( 'NONE',  ( 0.1067246931122726866, 0.02962905676920215767, 0.000000000000000000 ) ) ;
#16212 = VERTEX_POINT ( 'NONE', #38288 ) ;
#16213 = B_SPLINE_CURVE_WITH_KNOTS ( 'NONE', 3,
 ( #25575, #32574, #48263, #41333 ),
 .UNSPECIFIED., .F., .F.,
 ( 4, 4 ),
 ( 0.001512128760873999826, 0.004012308088711828702 ),
 .UNSPECIFIED. ) ;
#16214 = EDGE_CURVE ( 'NONE', #18782, #49800, #3407, .T. ) ;
#16215 = DIRECTION ( 'NONE',  ( -0.5128992774059071280, 0.000000000000000000, 0.8584487936018655452 ) ) ;
#16216 = AXIS2_PLACEMENT_3D ( 'NONE', #41946, #31085, #46788 ) ;
#16217 = ORIENTED_EDGE ( 'NONE', *, *, #43855, .T. ) ;
#16218 = ORIENTED_EDGE ( 'NONE', *, *, #38733, .F. ) ;
#16219 = CARTESIAN_POINT ( 'NONE',  ( 1.287906020515829919, 3.267716535433071279, -1.259842519685035134 ) ) ;
#16220 = CONICAL_SURFACE ( 'NONE', #47495, 1.850107469027523210, 0.6386652850508578450 ) ;
#16221 = CARTESIAN_POINT ( 'NONE',  ( -0.5284761224300580373, 1.574803149606302854, -2.099874368989736784 ) ) ;
#16222 = ORIENTED_EDGE ( 'NONE', *, *, #40079, .F. ) ;
#16223 = DIRECTION ( 'NONE',  ( 0.000000000000000000, 0.000000000000000000, 1.000000000000000000 ) ) ;
#16224 = ORIENTED_EDGE ( 'NONE', *, *, #33665, .F. ) ;
#16225 = CARTESIAN_POINT ( 'NONE',  ( 2.106197740627111958, 3.346456692913386100, 0.5905511811023582691 ) ) ;
#16226 = DIRECTION ( 'NONE',  ( 0.000000000000000000, 1.160734090543304660E-16, -1.000000000000000000 ) ) ;
#16227 = CARTESIAN_POINT ( 'NONE',  ( 0.002207914879453961535, 2.455437289341238936E-16, -2.115467123904954505 ) ) ;
#16228 = ORIENTED_EDGE ( 'NONE', *, *, #1438, .T. ) ;
#16229 = EDGE_LOOP ( 'NONE', ( #28738, #5462, #25113, #31691 ) ) ;
#16230 = DIRECTION ( 'NONE',  ( 1.734723475976806848E-16, -0.000000000000000000, 1.000000000000000000 ) ) ;
#16231 = CARTESIAN_POINT ( 'NONE',  ( 1.882988517681382756, 6.692913385826772199, 1.069164917025817951 ) ) ;
#16232 = FACE_OUTER_BOUND ( 'NONE', #14688, .T. ) ;
#16233 = LINE ( 'NONE', #16751, #35076 ) ;
#16234 = DIRECTION ( 'NONE',  ( 7.097135778201508621E-17, 1.000000000000000000, 1.075170113095020677E-16 ) ) ;
#16235 = ADVANCED_FACE ( 'NONE', ( #12682 ), #48002, .F. ) ;
#16236 = CARTESIAN_POINT ( 'NONE',  ( 1.084824920504545324E-16, 2.755905511811023612, 0.8858267716535433989 ) ) ;
#16237 = ORIENTED_EDGE ( 'NONE', *, *, #14365, .F. ) ;
#16238 = VECTOR ( 'NONE', #19216, 39.37007874015748143 ) ;
#16239 = EDGE_CURVE ( 'NONE', #41806, #286, #50835, .T. ) ;
#16240 = DIRECTION ( 'NONE',  ( -3.469446951953613696E-16, 0.000000000000000000, -1.000000000000000000 ) ) ;
#16241 = DIMENSIONAL_EXPONENTS ( 1.000000000000000000, 0.000000000000000000, 0.000000000000000000, 0.000000000000000000, 0.000000000000000000, 0.000000000000000000, 0.000000000000000000 ) ;
#16242 = ORIENTED_EDGE ( 'NONE', *, *, #2609, .T. ) ;
#16243 = VECTOR ( 'NONE', #12355, 39.37007874015748143 ) ;
#16244 = PLANE ( 'NONE',  #2039 ) ;
#16245 = EDGE_LOOP ( 'NONE', ( #15153, #42120, #46059, #21967 ) ) ;
#16246 = CARTESIAN_POINT ( 'NONE',  ( -1.091055626815042645, 0.000000000000000000, -1.456692913385822186 ) ) ;
#16247 = DIRECTION ( 'NONE',  ( -0.000000000000000000, 0.000000000000000000, 1.000000000000000000 ) ) ;
#16248 = LINE ( 'NONE', #8502, #39137 ) ;
#16249 = VECTOR ( 'NONE', #37000, 39.37007874015748143 ) ;
#16250 = ORIENTED_EDGE ( 'NONE', *, *, #22026, .T. ) ;
#16251 = CARTESIAN_POINT ( 'NONE',  ( 1.287906020515830141, 3.346456692913386100, -0.6299212598425181220 ) ) ;
#16252 = ORIENTED_EDGE ( 'NONE', *, *, #28848, .F. ) ;
#16253 = CARTESIAN_POINT ( 'NONE',  ( 0.5455278134075208785, 3.346456692913386100, -1.574803149606293529 ) ) ;
#16254 = VERTEX_POINT ( 'NONE', #11909 ) ;
#16255 = DIRECTION ( 'NONE',  ( 1.734723475976806848E-16, -0.000000000000000000, 1.000000000000000000 ) ) ;
#16256 = DIRECTION ( 'NONE',  ( 0.000000000000000000, 0.000000000000000000, -1.000000000000000000 ) ) ;
#16257 = EDGE_CURVE ( 'NONE', #24019, #8765, #43649, .T. ) ;
#16258 = CARTESIAN_POINT ( 'NONE',  ( 1.064142702668988694, 0.000000000000000000, -1.380941303491905359 ) ) ;
#16259 = ORIENTED_EDGE ( 'NONE', *, *, #47366, .F. ) ;
#16260 = ORIENTED_EDGE ( 'NONE', *, *, #47463, .T. ) ;
#16261 = DIRECTION ( 'NONE',  ( -0.000000000000000000, 1.000000000000000000, -0.000000000000000000 ) ) ;
#16262 = DIRECTION ( 'NONE',  ( 1.000000000000000000, -0.000000000000000000, 0.000000000000000000 ) ) ;
#16263 = FACE_BOUND ( 'NONE', #37251, .T. ) ;
#16264 = EDGE_CURVE ( 'NONE', #34259, #35717, #287, .T. ) ;
#16265 = DIRECTION ( 'NONE',  ( -1.000000000000000000, 0.000000000000000000, -0.000000000000000000 ) ) ;
#16266 = PLANE ( 'NONE',  #7691 ) ;
#16267 = VECTOR ( 'NONE', #10182, 39.37007874015748143 ) ;
#16268 = EDGE_CURVE ( 'NONE', #1395, #20168, #7787, .T. ) ;
#16269 = AXIS2_PLACEMENT_3D ( 'NONE', #4370, #16247, #28367 ) ;
#16270 = VERTEX_POINT ( 'NONE', #32312 ) ;
#16271 = CARTESIAN_POINT ( 'NONE',  ( -1.929629134066536134, 6.692913385826772199, 0.9824921284572121216 ) ) ;
#16272 = VECTOR ( 'NONE', #43005, 39.37007874015748854 ) ;
#16273 = ADVANCED_FACE ( 'NONE', ( #8293 ), #39789, .F. ) ;
#16274 = ORIENTED_EDGE ( 'NONE', *, *, #49487, .F. ) ;
#16275 = ORIENTED_EDGE ( 'NONE', *, *, #1533, .F. ) ;
#16276 = SHAPE_DEFINITION_REPRESENTATION ( #7500, #50198 ) ;
#16278 = ADVANCED_FACE ( 'NONE', ( #19390 ), #24557, .T. ) ;
#16277 = ORIENTED_EDGE ( 'NONE', *, *, #10668, .T. ) ;
#16279 = CARTESIAN_POINT ( 'NONE',  ( -1.166969139818016199, 3.267716535433071279, -1.614173228346451605 ) ) ;
#16280 = LINE ( 'NONE', #28400, #9323 ) ;
#16281 = DIRECTION ( 'NONE',  ( 1.734723475976806848E-16, 0.000000000000000000, 1.000000000000000000 ) ) ;
#16282 = LINE ( 'NONE', #23772, #14814 ) ;
#16283 = VERTEX_POINT ( 'NONE', #27906 ) ;
#16284 = EDGE_LOOP ( 'NONE', ( #2067, #32269, #47045, #38098, #48559 ) ) ;
#16285 = DIRECTION ( 'NONE',  ( -1.105928667600717569E-16, 1.000000000000000000, -6.607616187506203079E-17 ) ) ;
#16286 = CARTESIAN_POINT ( 'NONE',  ( -0.3136974817027967100, 1.615928078135840051, -2.936457595020224520 ) ) ;
#16287 = CARTESIAN_POINT ( 'NONE',  ( 1.091055626815042423, 3.346456692913386100, -1.771653543307081691 ) ) ;
#16288 = VECTOR ( 'NONE', #5314, 39.37007874015748143 ) ;
#16289 = ORIENTED_EDGE ( 'NONE', *, *, #26443, .F. ) ;
#16290 = DIRECTION ( 'NONE',  ( 1.000000000000000000, -0.000000000000000000, 0.000000000000000000 ) ) ;
#16291 = DIRECTION ( 'NONE',  ( -0.000000000000000000, 1.000000000000000000, -0.000000000000000000 ) ) ;
#16292 = ADVANCED_FACE ( 'NONE', ( #12166 ), #20157, .F. ) ;
#16293 = DIRECTION ( 'NONE',  ( 0.000000000000000000, 0.000000000000000000, -1.000000000000000000 ) ) ;
#16294 = EDGE_CURVE ( 'NONE', #45764, #39732, #43903, .T. ) ;
#16295 = EDGE_CURVE ( 'NONE', #27405, #5605, #22973, .T. ) ;
#16296 = DIRECTION ( 'NONE',  ( -3.469446951953613696E-16, 0.000000000000000000, -1.000000000000000000 ) ) ;
#16297 = DIRECTION ( 'NONE',  ( 0.9009688679024154823, 0.000000000000000000, 0.4338837391175656699 ) ) ;
#16298 = ORIENTED_EDGE ( 'NONE', *, *, #32265, .F. ) ;
#16299 = ADVANCED_FACE ( 'NONE', ( #8037 ), #7735, .T. ) ;
#16300 = DIRECTION ( 'NONE',  ( 1.000000000000000000, 0.000000000000000000, 0.000000000000000000 ) ) ;
#16301 = CARTESIAN_POINT ( 'NONE',  ( 0.4696143004045478797, 3.346456692913386100, -1.614173228346451605 ) ) ;
#16302 = ORIENTED_EDGE ( 'NONE', *, *, #12858, .T. ) ;
#16303 = EDGE_LOOP ( 'NONE', ( #16761, #13876, #19762, #44928 ) ) ;
#16304 = CARTESIAN_POINT ( 'NONE',  ( -0.5455278134075214336, 3.346456692913386100, -1.574803149606293529 ) ) ;
#16305 = CARTESIAN_POINT ( 'NONE',  ( -2.134236802639925656, 5.905511811023623991, -2.040539317874611402 ) ) ;
#16306 = DIRECTION ( 'NONE',  ( 1.000000000000000000, 0.000000000000000000, 0.000000000000000000 ) ) ;
#16307 = VECTOR ( 'NONE', #26971, 39.37007874015748143 ) ;
#16308 = ORIENTED_EDGE ( 'NONE', *, *, #7180, .T. ) ;
#16309 = AXIS2_PLACEMENT_3D ( 'NONE', #35741, #40397, #372 ) ;
#16310 = EDGE_CURVE ( 'NONE', #41937, #11420, #4684, .T. ) ;
#16311 = VERTEX_POINT ( 'NONE', #39533 ) ;
#16312 = LINE ( 'NONE', #27661, #26240 ) ;
#16313 = CONICAL_SURFACE ( 'NONE', #15504, 2.246510896728926010, 0.01601546068027819014 ) ;
#16314 = VERTEX_POINT ( 'NONE', #3917 ) ;
#16315 = DIRECTION ( 'NONE',  ( -0.9998717552508122886, -0.01601477604151185785, 0.000000000000000000 ) ) ;
#16316 = VERTEX_POINT ( 'NONE', #27393 ) ;
#16317 = CARTESIAN_POINT ( 'NONE',  ( 0.000000000000000000, 1.574803149606302854, 0.000000000000000000 ) ) ;
#16318 = FACE_OUTER_BOUND ( 'NONE', #46004, .T. ) ;
#16319 = DIRECTION ( 'NONE',  ( 1.000000000000000000, 0.000000000000000000, -3.469446951953613696E-16 ) ) ;
#16320 = EDGE_CURVE ( 'NONE', #25880, #49218, #31797, .T. ) ;
#16321 = VECTOR ( 'NONE', #39196, 39.37007874015748143 ) ;
#16322 = ORIENTED_EDGE ( 'NONE', *, *, #33271, .F. ) ;
#16323 = VERTEX_POINT ( 'NONE', #35162 ) ;
#16324 = EDGE_LOOP ( 'NONE', ( #20186, #1175, #27423, #45907 ) ) ;
#16325 = DIRECTION ( 'NONE',  ( 1.000000000000000000, 0.000000000000000000, -3.469446951953613696E-16 ) ) ;
#16326 = ORIENTED_EDGE ( 'NONE', *, *, #12867, .F. ) ;
#16327 = ORIENTED_EDGE ( 'NONE', *, *, #35937, .F. ) ;
#16328 = DIRECTION ( 'NONE',  ( -3.469446951953613696E-16, 0.000000000000000000, -1.000000000000000000 ) ) ;
#16329 = DIRECTION ( 'NONE',  ( -0.9998717552508122886, -0.01601477604151180928, 0.000000000000000000 ) ) ;
#16330 = LINE ( 'NONE', #47525, #3836 ) ;
#16331 = VECTOR ( 'NONE', #999, 39.37007874015748143 ) ;
#16332 = EDGE_CURVE ( 'NONE', #22069, #23247, #46983, .T. ) ;
#16333 = EDGE_LOOP ( 'NONE', ( #3188, #36838 ) ) ;
#16334 = ADVANCED_FACE ( 'NONE', ( #19645 ), #39070, .F. ) ;
#16335 = CARTESIAN_POINT ( 'NONE',  ( -0.01640406435879156535, 1.718999825676433835, 2.952755905511811108 ) ) ;
#16336 = CARTESIAN_POINT ( 'NONE',  ( 1.779568955232893712, 6.692913385826772199, -1.233650562797287353 ) ) ;
#16337 = FACE_OUTER_BOUND ( 'NONE', #29547, .T. ) ;
#16338 = EDGE_CURVE ( 'NONE', #33355, #3033, #15778, .T. ) ;
#16339 = EDGE_LOOP ( 'NONE', ( #46037, #14868, #31450, #15127 ) ) ;
#16340 = DIRECTION ( 'NONE',  ( 1.734723475976806848E-16, -0.000000000000000000, 1.000000000000000000 ) ) ;
#16341 = EDGE_CURVE ( 'NONE', #4498, #50396, #44669, .T. ) ;
#16342 = CARTESIAN_POINT ( 'NONE',  ( 1.015142113812069313, 3.346456692913386100, -1.299212598425193210 ) ) ;
#16343 = ORIENTED_EDGE ( 'NONE', *, *, #13961, .F. ) ;
#16344 = CARTESIAN_POINT ( 'NONE',  ( 0.000000000000000000, 3.346456692913386100, -2.874015748031496731 ) ) ;
#16345 = VERTEX_POINT ( 'NONE', #13454 ) ;
#16346 = VERTEX_POINT ( 'NONE', #28932 ) ;
#16347 = CARTESIAN_POINT ( 'NONE',  ( -0.7874015748031498729, 0.000000000000000000, -1.138269997360109921E-16 ) ) ;
#16348 = CARTESIAN_POINT ( 'NONE',  ( -0.07591351300297277671, 3.346456692913386100, 0.7874015748031456541 ) ) ;
#16349 = CARTESIAN_POINT ( 'NONE',  ( -0.9845150457423005319, 0.000000000000000000, -1.438794182654565601 ) ) ;
#16350 = VECTOR ( 'NONE', #24458, 39.37007874015748143 ) ;
#16351 = DIRECTION ( 'NONE',  ( -0.9998717552508122886, -0.01601477604151181275, 0.000000000000000000 ) ) ;
#16352 = EDGE_CURVE ( 'NONE', #18551, #42223, #16816, .T. ) ;
#16353 = CARTESIAN_POINT ( 'NONE',  ( -2.182111253630085734, 3.267716535433071279, 3.785359618865289765E-16 ) ) ;
#16354 = ORIENTED_EDGE ( 'NONE', *, *, #32067, .F. ) ;
#16355 = ORIENTED_EDGE ( 'NONE', *, *, #23742, .T. ) ;
#16356 = VECTOR ( 'NONE', #6325, 39.37007874015748143 ) ;
#16357 = ADVANCED_FACE ( 'NONE', ( #4937 ), #29188, .T. ) ;
#16358 = EDGE_LOOP ( 'NONE', ( #44657, #6266, #37960, #30732 ) ) ;
#16359 = PLANE ( 'NONE',  #14556 ) ;
#16360 = CARTESIAN_POINT ( 'NONE',  ( 1.015142113812069313, 3.267716535433071279, -0.7874015748031473194 ) ) ;
#16361 = AXIS2_PLACEMENT_3D ( 'NONE', #40329, #32588, #4947 ) ;
#16362 = EDGE_CURVE ( 'NONE', #11338, #4264, #9065, .T. ) ;
#16363 = EDGE_CURVE ( 'NONE', #24535, #7807, #28336, .T. ) ;
#16364 = AXIS2_PLACEMENT_3D ( 'NONE', #14129, #1741, #26004 ) ;
#16365 = CARTESIAN_POINT ( 'NONE',  ( 0.2727639067037604947, 0.000000000000000000, -0.4724409448818886470 ) ) ;
#16366 = CARTESIAN_POINT ( 'NONE',  ( 1.287906020515829475, 3.267716535433071279, -4.468321617281353104E-16 ) ) ;
#16367 = CARTESIAN_POINT ( 'NONE',  ( -0.6214413264104939882, 0.000000000000000000, 1.102362204724404160 ) ) ;
#16368 = VERTEX_POINT ( 'NONE', #17329 ) ;
#16369 = ADVANCED_FACE ( 'NONE', ( #13963 ), #20109, .T. ) ;
#16370 = DIRECTION ( 'NONE',  ( -1.000000000000000000, 0.000000000000000000, 1.734723475976806848E-16 ) ) ;
#16371 = ADVANCED_FACE ( 'NONE', ( #36693 ), #49285, .F. ) ;
#16372 = VECTOR ( 'NONE', #34538, 39.37007874015747433 ) ;
#16373 = CARTESIAN_POINT ( 'NONE',  ( -1.636583440222564301, 3.346456692913386100, -1.417869535855831975 ) ) ;
#16374 = ORIENTED_EDGE ( 'NONE', *, *, #42206, .F. ) ;
#16375 = LINE ( 'NONE', #4751, #21608 ) ;
#16376 = DIRECTION ( 'NONE',  ( -1.000000000000000000, 0.000000000000000000, -0.000000000000000000 ) ) ;
#16377 = CARTESIAN_POINT ( 'NONE',  ( -1.636583440222563635, 3.346456692913386100, 0.3149606299212578953 ) ) ;
#16378 = VERTEX_POINT ( 'NONE', #40820 ) ;
#16379 = CARTESIAN_POINT ( 'NONE',  ( 0.000000000000000000, 3.267716535433071279, -0.5118110236220471121 ) ) ;
#16380 = CARTESIAN_POINT ( 'NONE',  ( -1.364345965745727973, 1.205361022782829114E-17, 1.150974876880269893 ) ) ;
#16381 = DIRECTION ( 'NONE',  ( 0.01601477604151182663, -0.9998717552508123996, 0.000000000000000000 ) ) ;
#16382 = ORIENTED_EDGE ( 'NONE', *, *, #37460, .T. ) ;
#16383 = CARTESIAN_POINT ( 'NONE',  ( 0.000000000000000000, 3.267716535433071279, -0.8267716535433052849 ) ) ;
#16384 = CARTESIAN_POINT ( 'NONE',  ( -1.909347346926324906, 3.346456692913386100, -0.4724409448818884805 ) ) ;
#16385 = EDGE_LOOP ( 'NONE', ( #2611, #48613, #50956, #5285 ) ) ;
#16386 = CARTESIAN_POINT ( 'NONE',  ( -1.716666360678977155, 3.267716535433071279, 1.220472440944875059 ) ) ;
#16387 = CARTESIAN_POINT ( 'NONE',  ( 0.2727639067037609943, 0.000000000000000000, 0.9055118110236167750 ) ) ;
#16388 = DIRECTION ( 'NONE',  ( 0.000000000000000000, 0.000000000000000000, -1.000000000000000000 ) ) ;
#16389 = CARTESIAN_POINT ( 'NONE',  ( 0.6551740444401462637, 0.000000000000000000, 1.885762267972743711 ) ) ;
#16390 = AXIS2_PLACEMENT_3D ( 'NONE', #24651, #40408, #5025 ) ;
#16391 = VERTEX_POINT ( 'NONE', #24816 ) ;
#16392 = EDGE_LOOP ( 'NONE', ( #14682, #41420, #47982, #11803 ) ) ;
#16393 = DIRECTION ( 'NONE',  ( -0.000000000000000000, 1.000000000000000000, -0.000000000000000000 ) ) ;
#16394 = CARTESIAN_POINT ( 'NONE',  ( -2.151809081513409438, 1.575012187087082127, 0.2418202932658340965 ) ) ;
#16395 = VERTEX_POINT ( 'NONE', #17078 ) ;
#16396 = CARTESIAN_POINT ( 'NONE',  ( -1.363819533518803473, 3.267716535433071279, -1.605145679676863057 ) ) ;
#16397 = PLANE ( 'NONE',  #5450 ) ;
#16398 = DIRECTION ( 'NONE',  ( 1.000000000000000000, 0.000000000000000000, 0.000000000000000000 ) ) ;
#16399 = CARTESIAN_POINT ( 'NONE',  ( -0.7317238754971217007, 0.1411726943947596014, -1.345337514773771614 ) ) ;
#16400 = VECTOR ( 'NONE', #34691, 39.37007874015748143 ) ;
#16401 = VECTOR ( 'NONE', #42042, 39.37007874015748143 ) ;
#16402 = EDGE_LOOP ( 'NONE', ( #17167, #15375, #35247, #11964, #6934, #315, #46269, #9492, #12453, #40912, #31142, #5707, #39452, #45201, #46520, #50799, #28617, #12072, #29309, #49661, #33003, #21847, #25346, #44842, #37880, #17581, #26833, #43698, #41104, #9854, #1876, #26768, #46205, #9908, #29092, #37258, #15811, #2239, #11685, #4845, #30724, #19092, #16475, #49666, #37664, #8726, #32647, #24278, #27200, #3858, #5869, #12045, #39295, #21809, #34397, #12063, #43042, #27572, #22569, #36803, #15801, #16026, #47801, #17901, #8561, #9847, #29476, #31420, #41530, #6633, #34757, #28810, #37625, #25019, #2744, #17238, #17960, #10078, #3107, #13934, #35284, #38043, #36552, #38270 ) ) ;
#16403 = ORIENTED_EDGE ( 'NONE', *, *, #28410, .F. ) ;
#16404 = EDGE_CURVE ( 'NONE', #10377, #35860, #34949, .T. ) ;
#16405 = CARTESIAN_POINT ( 'NONE',  ( -2.182111253630085290, 0.000000000000000000, 0.3149606299212578953 ) ) ;
#16406 = CARTESIAN_POINT ( 'NONE',  ( -2.161044708975090156, 0.000000000000000000, 0.1463148319730351032 ) ) ;
#16407 = CARTESIAN_POINT ( 'NONE',  ( -0.2727639067037607723, 3.346456692913386100, 2.362204724409437961 ) ) ;
#16408 = VECTOR ( 'NONE', #32048, 39.37007874015748143 ) ;
#16409 = DIRECTION ( 'NONE',  ( -0.01601477604151182663, 0.9998717552508123996, -0.000000000000000000 ) ) ;
#16410 = EDGE_CURVE ( 'NONE', #18300, #19616, #13204, .T. ) ;
#16411 = FACE_BOUND ( 'NONE', #2692, .T. ) ;
#16412 = ORIENTED_EDGE ( 'NONE', *, *, #8488, .T. ) ;
#16413 = EDGE_CURVE ( 'NONE', #48369, #28465, #16213, .T. ) ;
#16414 = CARTESIAN_POINT ( 'NONE',  ( 0.1968503937007874127, 3.267716535433071279, -6.829619984160656814E-17 ) ) ;
#16415 = EDGE_LOOP ( 'NONE', ( #38693, #860, #23640, #19378 ) ) ;
#16416 = VERTEX_POINT ( 'NONE', #5445 ) ;
#16417 = VECTOR ( 'NONE', #32646, 39.37007874015748143 ) ;
#16418 = FACE_OUTER_BOUND ( 'NONE', #14150, .T. ) ;
#16419 = ORIENTED_EDGE ( 'NONE', *, *, #15739, .T. ) ;
#16420 = ORIENTED_EDGE ( 'NONE', *, *, #37870, .F. ) ;
#16421 = CARTESIAN_POINT ( 'NONE',  ( -1.790900357307437352, 1.580792207208895128, -1.241130355818072406 ) ) ;
#16422 = ORIENTED_EDGE ( 'NONE', *, *, #47662, .F. ) ;
#16423 = ADVANCED_FACE ( 'NONE', ( #5953 ), #27518, .F. ) ;
#16424 = CARTESIAN_POINT ( 'NONE',  ( -0.9838852166859199944, 1.205361022782829114E-17, 1.929635236160303302 ) ) ;
#16425 = CARTESIAN_POINT ( 'NONE',  ( -0.6214413264104945434, 0.000000000000000000, -0.03937007874015895081 ) ) ;
#16426 = CARTESIAN_POINT ( 'NONE',  ( -1.439733046521776139, 0.000000000000000000, -4.780733988912460139E-16 ) ) ;
#16427 = EDGE_CURVE ( 'NONE', #8967, #17096, #40562, .T. ) ;
#16428 = CIRCLE ( 'NONE', #3223, 1.743387098533651480 ) ;
#16429 = CARTESIAN_POINT ( 'NONE',  ( 0.000000000000000000, 3.267716535433071279, -0.5118110236220467790 ) ) ;
#16430 = DIRECTION ( 'NONE',  ( 1.000000000000000000, 0.000000000000000000, 0.000000000000000000 ) ) ;
#16431 = LINE ( 'NONE', #16947, #17150 ) ;
#16432 = ORIENTED_EDGE ( 'NONE', *, *, #26136, .T. ) ;
#16433 = DIRECTION ( 'NONE',  ( -0.000000000000000000, -1.000000000000000000, -0.000000000000000000 ) ) ;
#16434 = ADVANCED_FACE ( 'NONE', ( #21201 ), #33599, .F. ) ;
#16435 = PLANE ( 'NONE',  #14476 ) ;
#16436 = CARTESIAN_POINT ( 'NONE',  ( 1.091055626815042645, 0.000000000000000000, 0.3149606299212578953 ) ) ;
#16437 = AXIS2_PLACEMENT_3D ( 'NONE', #11465, #35464, #38586 ) ;
#16438 = VERTEX_POINT ( 'NONE', #33089 ) ;
#16439 = LINE ( 'NONE', #23922, #45421 ) ;
#16440 = CARTESIAN_POINT ( 'NONE',  ( -1.733991708815627808, 9.921953787815782565E-05, 0.1852230845914871471 ) ) ;
#16441 = ORIENTED_EDGE ( 'NONE', *, *, #7195, .T. ) ;
#16442 = DIRECTION ( 'NONE',  ( -3.469446951953613696E-16, 0.000000000000000000, -1.000000000000000000 ) ) ;
#16443 = PLANE ( 'NONE',  #39868 ) ;
#16444 = AXIS2_PLACEMENT_3D ( 'NONE', #45815, #46074, #38857 ) ;
#16445 = DIRECTION ( 'NONE',  ( 0.01601477604151182663, -0.9998717552508123996, 0.000000000000000000 ) ) ;
#16446 = VERTEX_POINT ( 'NONE', #17832 ) ;
#16447 = LINE ( 'NONE', #32199, #175 ) ;
#16448 = VECTOR ( 'NONE', #16901, 39.37007874015748143 ) ;
#16449 = EDGE_LOOP ( 'NONE', ( #50615, #17356, #6350, #17578 ) ) ;
#16450 = CARTESIAN_POINT ( 'NONE',  ( -0.3136974817027967100, 1.615928078135840051, -2.936457595020224520 ) ) ;
#16451 = CARTESIAN_POINT ( 'NONE',  ( 0.000000000000000000, 0.000000000000000000, 0.000000000000000000 ) ) ;
#16452 = DIRECTION ( 'NONE',  ( -3.469446951953613696E-16, 0.000000000000000000, -1.000000000000000000 ) ) ;
#16453 = CARTESIAN_POINT ( 'NONE',  ( -0.6214413264104940993, 3.267716535433071279, 2.156057715732899547E-16 ) ) ;
#16454 = ORIENTED_EDGE ( 'NONE', *, *, #42419, .T. ) ;
#16455 = VERTEX_POINT ( 'NONE', #48771 ) ;
#16456 = CARTESIAN_POINT ( 'NONE',  ( -0.5455278134075214336, 3.346456692913386100, -8.878505979408855953E-16 ) ) ;
#16457 = VERTEX_POINT ( 'NONE', #44924 ) ;
#16458 = FACE_OUTER_BOUND ( 'NONE', #3041, .T. ) ;
#16459 = ORIENTED_EDGE ( 'NONE', *, *, #23041, .F. ) ;
#16460 = CARTESIAN_POINT ( 'NONE',  ( -0.6214413264104939882, 3.346456692913386100, 0.2755905511810998187 ) ) ;
#16461 = VECTOR ( 'NONE', #7251, 39.37007874015748143 ) ;
#16462 = VERTEX_POINT ( 'NONE', #1828 ) ;
#16463 = CARTESIAN_POINT ( 'NONE',  ( -1.983184043548481545, 1.684331982857502519, -1.828031556756394727 ) ) ;
#16464 = LINE ( 'NONE', #47913, #33910 ) ;
#16465 = EDGE_CURVE ( 'NONE', #30930, #24374, #13711, .T. ) ;
#16466 = VERTEX_POINT ( 'NONE', #34845 ) ;
#16467 = EDGE_CURVE ( 'NONE', #13984, #1578, #10599, .T. ) ;
#16468 = DIRECTION ( 'NONE',  ( 0.000000000000000000, 1.000000000000000000, 0.000000000000000000 ) ) ;
#16469 = ORIENTED_EDGE ( 'NONE', *, *, #36220, .F. ) ;
#16470 = EDGE_CURVE ( 'NONE', #34365, #46240, #26340, .T. ) ;
#16471 = ADVANCED_FACE ( 'NONE', ( #21969, #2344 ), #50040, .T. ) ;
#16472 = AXIS2_PLACEMENT_3D ( 'NONE', #11896, #30516, #30763 ) ;
#16473 = CARTESIAN_POINT ( 'NONE',  ( -2.803168555496243108, 1.675558592011573644, 0.9280531160220438780 ) ) ;
#16475 = ORIENTED_EDGE ( 'NONE', *, *, #44784, .F. ) ;
#16474 = EDGE_CURVE ( 'NONE', #20192, #1675, #6976, .T. ) ;
#16476 = VERTEX_POINT ( 'NONE', #42087 ) ;
#16477 = CARTESIAN_POINT ( 'NONE',  ( -1.556712866041156440, 1.596563264426776207, 2.509548638715847435 ) ) ;
#16478 = CARTESIAN_POINT ( 'NONE',  ( 1.944213194762889119, 0.05905979794000976862, 0.2136995197171435157 ) ) ;
#16479 = VERTEX_POINT ( 'NONE', #41838 ) ;
#16480 = AXIS2_PLACEMENT_3D ( 'NONE', #39298, #27927, #3935 ) ;
#16481 = DIRECTION ( 'NONE',  ( -1.000000000000000000, 0.000000000000000000, 1.734723475976806848E-16 ) ) ;
#16482 = EDGE_LOOP ( 'NONE', ( #2615, #2429, #6945, #27593 ) ) ;
#16483 = CARTESIAN_POINT ( 'NONE',  ( -1.909347346926324462, 3.267716535433071279, 0.1574803149606286423 ) ) ;
#16484 = FACE_OUTER_BOUND ( 'NONE', #33200, .T. ) ;
#16485 = EDGE_CURVE ( 'NONE', #38922, #3379, #6473, .T. ) ;
#16486 = DIRECTION ( 'NONE',  ( 0.000000000000000000, 0.000000000000000000, -1.000000000000000000 ) ) ;
#16487 = VERTEX_POINT ( 'NONE', #18091 ) ;
#16488 = ORIENTED_EDGE ( 'NONE', *, *, #13219, .T. ) ;
#16489 = PLANE ( 'NONE',  #45884 ) ;
#16490 = CARTESIAN_POINT ( 'NONE',  ( 0.000000000000000000, 3.267716535433071279, 0.4724409448818868706 ) ) ;
#16491 = DIRECTION ( 'NONE',  ( -0.000000000000000000, 1.000000000000000000, -0.000000000000000000 ) ) ;
#16492 = CARTESIAN_POINT ( 'NONE',  ( 0.000000000000000000, 1.574803149606302854, 0.000000000000000000 ) ) ;
#16493 = ADVANCED_FACE ( 'NONE', ( #46683 ), #14722, .F. ) ;
#16494 = DIRECTION ( 'NONE',  ( -0.000000000000000000, 0.000000000000000000, 1.000000000000000000 ) ) ;
#16495 = DIRECTION ( 'NONE',  ( -0.7227948638273878901, 0.000000000000000000, -0.6910626489868684219 ) ) ;
#16496 = B_SPLINE_CURVE_WITH_KNOTS ( 'NONE', 3,
 ( #5914, #17792, #33559, #43041 ),
 .UNSPECIFIED., .F., .F.,
 ( 4, 4 ),
 ( 5.511647321497469134E-05, 0.004930157801157326360 ),
 .UNSPECIFIED. ) ;
#16497 = LINE ( 'NONE', #23721, #6193 ) ;
#16498 = AXIS2_PLACEMENT_3D ( 'NONE', #42678, #6814, #50376 ) ;
#16499 = ORIENTED_EDGE ( 'NONE', *, *, #27385, .T. ) ;
#16500 = DIRECTION ( 'NONE',  ( 0.9998717552508121775, 0.01601477604151182663, 0.000000000000000000 ) ) ;
#16501 = EDGE_LOOP ( 'NONE', ( #33829, #31054, #23249, #28944 ) ) ;
#16502 = CARTESIAN_POINT ( 'NONE',  ( -0.1158910538491989134, 0.02606345816900213982, -1.836661962001401305 ) ) ;
#16503 = ORIENTED_EDGE ( 'NONE', *, *, #978, .F. ) ;
#16504 = B_SPLINE_CURVE_WITH_KNOTS ( 'NONE', 3,
 ( #33876, #6749, #13478, #45957 ),
 .UNSPECIFIED., .F., .F.,
 ( 4, 4 ),
 ( 6.390876033150945367E-07, 0.003275970498226882938 ),
 .UNSPECIFIED. ) ;
#16505 = EDGE_CURVE ( 'NONE', #17713, #33393, #37723, .T. ) ;
#16506 = DIRECTION ( 'NONE',  ( 1.734723475976806848E-16, 0.000000000000000000, 1.000000000000000000 ) ) ;
#16507 = AXIS2_PLACEMENT_3D ( 'NONE', #736, #4102, #16486 ) ;
#16508 = LINE ( 'NONE', #7733, #17977 ) ;
#16509 = VECTOR ( 'NONE', #43950, 39.37007874015748143 ) ;
#16510 = CARTESIAN_POINT ( 'NONE',  ( 1.253212129322610613, 3.267716535433071279, 1.692913385826762873 ) ) ;
#16511 = CARTESIAN_POINT ( 'NONE',  ( 1.363819533518803695, 0.000000000000000000, 1.732283464566921172 ) ) ;
#16512 = ORIENTED_EDGE ( 'NONE', *, *, #45287, .F. ) ;
#16513 = CARTESIAN_POINT ( 'NONE',  ( -1.022165783746114442, 1.703323867449966889, 2.770237110794461444 ) ) ;
#16514 = FACE_BOUND ( 'NONE', #35819, .T. ) ;
#16515 = ORIENTED_EDGE ( 'NONE', *, *, #15350, .F. ) ;
#16516 = CARTESIAN_POINT ( 'NONE',  ( -1.591447364397243103, 0.002429723416550041374, -0.7337366736851151927 ) ) ;
#16517 = CIRCLE ( 'NONE', #7448, 2.164630168518208109 ) ;
#16518 = ORIENTED_EDGE ( 'NONE', *, *, #14574, .F. ) ;
#16519 = DIRECTION ( 'NONE',  ( 1.734723475976806848E-16, 0.000000000000000000, 1.000000000000000000 ) ) ;
#16520 = CARTESIAN_POINT ( 'NONE',  ( -1.171042467547485311, 1.689145562575557369, 1.864045119995098698 ) ) ;
#16521 = CARTESIAN_POINT ( 'NONE',  ( 0.7423782071083085965, 3.267716535433071279, -0.1968503937007880511 ) ) ;
#16522 = VERTEX_POINT ( 'NONE', #49532 ) ;
#16524 = EDGE_CURVE ( 'NONE', #3576, #44829, #45677, .T. ) ;
#16523 = ORIENTED_EDGE ( 'NONE', *, *, #837, .F. ) ;
#16525 = DIRECTION ( 'NONE',  ( -1.000000000000000000, 0.000000000000000000, 0.000000000000000000 ) ) ;
#16526 = DIRECTION ( 'NONE',  ( 0.5773502691896241767, 0.5773502691896261751, 0.5773502691896268413 ) ) ;
#16527 = FACE_BOUND ( 'NONE', #49319, .T. ) ;
#16528 = ADVANCED_FACE ( 'NONE', ( #14975 ), #10343, .F. ) ;
#16529 = DIRECTION ( 'NONE',  ( 1.734723475976806848E-16, 0.000000000000000000, 1.000000000000000000 ) ) ;
#16530 = DIRECTION ( 'NONE',  ( -0.000000000000000000, 1.000000000000000000, -0.000000000000000000 ) ) ;
#16531 = EDGE_CURVE ( 'NONE', #24393, #22479, #38227, .T. ) ;
#16532 = EDGE_CURVE ( 'NONE', #46587, #22536, #34352, .T. ) ;
#16533 = EDGE_LOOP ( 'NONE', ( #5206, #42918, #27089 ) ) ;
#16534 = B_SPLINE_CURVE_WITH_KNOTS ( 'NONE', 3,
 ( #34996, #7125, #41984, #30871 ),
 .UNSPECIFIED., .F., .F.,
 ( 4, 4 ),
 ( 0.01409063418847883789, 0.03074670260773034597 ),
 .UNSPECIFIED. ) ;
#16535 = DIRECTION ( 'NONE',  ( 0.6427876096865403621, -0.7660444431189770143, 1.858431260983764056E-16 ) ) ;
#16536 = ORIENTED_EDGE ( 'NONE', *, *, #37123, .F. ) ;
#16537 = ORIENTED_EDGE ( 'NONE', *, *, #44483, .T. ) ;
#16538 = CONTEXT_DEPENDENT_SHAPE_REPRESENTATION ( #33867, #15743 ) ;
#16539 = ORIENTED_EDGE ( 'NONE', *, *, #5290, .T. ) ;
#16540 = LINE ( 'NONE', #36676, #27592 ) ;
#16541 = AXIS2_PLACEMENT_3D ( 'NONE', #12811, #12036, #16164 ) ;
#16542 = CARTESIAN_POINT ( 'NONE',  ( -1.985260859929297794, 3.267716535433071279, 6.887757239314512246E-16 ) ) ;
#16543 = VECTOR ( 'NONE', #23816, 39.37007874015748143 ) ;
#16544 = EDGE_CURVE ( 'NONE', #1746, #46902, #49787, .T. ) ;
#16545 = CARTESIAN_POINT ( 'NONE',  ( -1.363819533518803473, 3.346456692913386100, -1.299212598425192544 ) ) ;
#16546 = CARTESIAN_POINT ( 'NONE',  ( -1.883550378546958060, 5.905511811023623991, -1.069467267250447495 ) ) ;
#16547 = ORIENTED_EDGE ( 'NONE', *, *, #11561, .F. ) ;
#16548 = ORIENTED_EDGE ( 'NONE', *, *, #46296, .T. ) ;
#16549 = CARTESIAN_POINT ( 'NONE',  ( 1.473819267337850736, 1.665891067178861151, 1.761720034108342769 ) ) ;
#16550 = DIRECTION ( 'NONE',  ( 1.000000000000000000, -0.000000000000000000, 2.891205793294678326E-16 ) ) ;
#16551 = CARTESIAN_POINT ( 'NONE',  ( 0.08119777152254364916, 1.623385212329073957, 0.000000000000000000 ) ) ;
#16552 = EDGE_CURVE ( 'NONE', #38226, #6075, #2850, .T. ) ;
#16553 = VECTOR ( 'NONE', #42978, 39.37007874015748143 ) ;
#16554 = LINE ( 'NONE', #4673, #10316 ) ;
#16555 = DIRECTION ( 'NONE',  ( -3.469446951953613696E-16, 0.000000000000000000, -1.000000000000000000 ) ) ;
#16556 = FACE_OUTER_BOUND ( 'NONE', #27202, .T. ) ;
#16557 = EDGE_CURVE ( 'NONE', #46515, #36309, #35624, .T. ) ;
#16558 = DIRECTION ( 'NONE',  ( 0.000000000000000000, 0.000000000000000000, -1.000000000000000000 ) ) ;
#16559 = CARTESIAN_POINT ( 'NONE',  ( -2.160407304981126320, 6.692913385826772199, -0.1462862061266902158 ) ) ;
#16560 = ORIENTED_EDGE ( 'NONE', *, *, #6740, .F. ) ;
#16561 = CARTESIAN_POINT ( 'NONE',  ( 2.182111253630085290, 0.000000000000000000, -0.3149606299212596716 ) ) ;
#16562 = CARTESIAN_POINT ( 'NONE',  ( -0.3486774197067334935, 0.000000000000000000, 1.377952755905504256 ) ) ;
#16563 = VERTEX_POINT ( 'NONE', #34097 ) ;
#16564 = EDGE_CURVE ( 'NONE', #2069, #23689, #22971, .T. ) ;
#16565 = ORIENTED_EDGE ( 'NONE', *, *, #36010, .F. ) ;
#16566 = CARTESIAN_POINT ( 'NONE',  ( -0.2727639067037607723, 0.000000000000000000, -0.4724409448818883694 ) ) ;
#16567 = CARTESIAN_POINT ( 'NONE',  ( -1.909347346926324906, 0.000000000000000000, -0.7874015748031470974 ) ) ;
#16568 = DIRECTION ( 'NONE',  ( -0.000000000000000000, 0.000000000000000000, 1.000000000000000000 ) ) ;
#16569 = EDGE_LOOP ( 'NONE', ( #615, #40423, #4274, #633 ) ) ;
#16570 = EDGE_CURVE ( 'NONE', #48759, #20718, #30722, .T. ) ;
#16571 = ORIENTED_EDGE ( 'NONE', *, *, #2070, .T. ) ;
#16572 = PLANE ( 'NONE',  #32028 ) ;
#16573 = ORIENTED_EDGE ( 'NONE', *, *, #42397, .F. ) ;
#16574 = LINE ( 'NONE', #4696, #27862 ) ;
#16575 = VERTEX_POINT ( 'NONE', #19089 ) ;
#16576 = EDGE_CURVE ( 'NONE', #26914, #18530, #7983, .T. ) ;
#16577 = VECTOR ( 'NONE', #9831, 39.37007874015748143 ) ;
#16578 = CARTESIAN_POINT ( 'NONE',  ( -1.363819533518803029, 3.267716535433071279, 2.365849761790804994E-16 ) ) ;
#16579 = LINE ( 'NONE', #19410, #49421 ) ;
#16580 = DIRECTION ( 'NONE',  ( -3.469446951953613696E-16, 0.000000000000000000, -1.000000000000000000 ) ) ;
#16581 = VECTOR ( 'NONE', #5730, 39.37007874015748143 ) ;
#16582 = ORIENTED_EDGE ( 'NONE', *, *, #32208, .T. ) ;
#16583 = ORIENTED_EDGE ( 'NONE', *, *, #13585, .F. ) ;
#16584 = ORIENTED_EDGE ( 'NONE', *, *, #43858, .T. ) ;
#16585 = DIRECTION ( 'NONE',  ( -0.000000000000000000, 0.000000000000000000, 1.000000000000000000 ) ) ;
#16586 = ORIENTED_EDGE ( 'NONE', *, *, #17306, .F. ) ;
#16587 = ORIENTED_EDGE ( 'NONE', *, *, #8882, .T. ) ;
#16588 = LINE ( 'NONE', #4712, #46179 ) ;
#16589 = DIRECTION ( 'NONE',  ( 0.000000000000000000, 0.000000000000000000, -1.000000000000000000 ) ) ;
#16590 = VECTOR ( 'NONE', #43615, 39.37007874015748143 ) ;
#16591 = DIRECTION ( 'NONE',  ( -0.1785568947986370392, 0.000000000000000000, 0.9839295885986295565 ) ) ;
#16592 = EDGE_CURVE ( 'NONE', #30490, #6449, #4118, .T. ) ;
#16593 = VECTOR ( 'NONE', #48955, 39.37007874015748143 ) ;
#16594 = ORIENTED_EDGE ( 'NONE', *, *, #11552, .T. ) ;
#16595 = CARTESIAN_POINT ( 'NONE',  ( 0.1968503937007873017, 3.346456692913386100, -0.3149606299212591165 ) ) ;
#16596 = CARTESIAN_POINT ( 'NONE',  ( -0.8182917201112819283, 3.267716535433071279, 1.850393700787391849 ) ) ;
#16597 = CARTESIAN_POINT ( 'NONE',  ( 1.062992125984252079, 0.4235180831842795257, -1.014069264286642014 ) ) ;
#16598 = ADVANCED_FACE ( 'NONE', ( #39479 ), #19842, .F. ) ;
#16599 = ORIENTED_EDGE ( 'NONE', *, *, #12095, .F. ) ;
#16600 = CARTESIAN_POINT ( 'NONE',  ( 0.8603116971394481061, 0.000000000000000000, -1.824450401507204278 ) ) ;
#16601 = DIRECTION ( 'NONE',  ( 1.734723475976806848E-16, -0.000000000000000000, 1.000000000000000000 ) ) ;
#16602 = ORIENTED_EDGE ( 'NONE', *, *, #15924, .F. ) ;
#16603 = CARTESIAN_POINT ( 'NONE',  ( 1.039905234370930742, 2.755905511811024056, -0.5599999049406324536 ) ) ;
#16604 = ORIENTED_EDGE ( 'NONE', *, *, #22184, .F. ) ;
#16605 = VERTEX_POINT ( 'NONE', #35610 ) ;
#16606 = LINE ( 'NONE', #40605, #50895 ) ;
#16607 = DIRECTION ( 'NONE',  ( 0.000000000000000000, 0.000000000000000000, -1.000000000000000000 ) ) ;
#16608 = CARTESIAN_POINT ( 'NONE',  ( -1.955085917884560320, 1.688780925004493838, 2.212843326065125460 ) ) ;
#16609 = B_SPLINE_CURVE_WITH_KNOTS ( 'NONE', 3,
 ( #22360, #2992, #7369, #22862 ),
 .UNSPECIFIED., .F., .F.,
 ( 4, 4 ),
 ( 0.01157806808172074861, 0.03073653090630815501 ),
 .UNSPECIFIED. ) ;
#16610 = CARTESIAN_POINT ( 'NONE',  ( 0.4693945290273940363, 0.01171413463600641872, -1.885797023163377828 ) ) ;
#16611 = ORIENTED_EDGE ( 'NONE', *, *, #42269, .F. ) ;
#16612 = ORIENTED_EDGE ( 'NONE', *, *, #45996, .T. ) ;
#16613 = LINE ( 'NONE', #13759, #36636 ) ;
#16614 = PRODUCT_DEFINITION_SHAPE ( 'NONE', 'NONE',  #14612 ) ;
#16615 = EDGE_LOOP ( 'NONE', ( #50416, #42086, #181, #37813 ) ) ;
#16616 = CARTESIAN_POINT ( 'NONE',  ( 1.833433833923351353, 0.000000000000000000, 0.4330708661417290162 ) ) ;
#16617 = CARTESIAN_POINT ( 'NONE',  ( 0.9989521216866641407, 0.000000000000000000, 1.767914056614194651 ) ) ;
#16618 = VECTOR ( 'NONE', #41454, 39.37007874015748143 ) ;
#16619 =( GEOMETRIC_REPRESENTATION_CONTEXT ( 3 ) GLOBAL_UNCERTAINTY_ASSIGNED_CONTEXT ( ( #24162 ) ) GLOBAL_UNIT_ASSIGNED_CONTEXT ( ( #23563, #19689, #46530 ) ) REPRESENTATION_CONTEXT ( 'NONE', 'WORKASPACE' ) );
#16620 = EDGE_CURVE ( 'NONE', #1302, #30490, #47949, .T. ) ;
#16621 = CARTESIAN_POINT ( 'NONE',  ( 2.121469926805689354, 2.755905511811027164, -0.4337334748181388422 ) ) ;
#16622 = DIRECTION ( 'NONE',  ( -3.986037398843765983E-20, -1.000000000000000000, -1.160734090543304660E-16 ) ) ;
#16624 = LINE ( 'NONE', #32376, #30307 ) ;
#16623 = CIRCLE ( 'NONE', #35597, 2.165354330708661568 ) ;
#16625 = VERTEX_POINT ( 'NONE', #4622 ) ;
#16626 = CYLINDRICAL_SURFACE ( 'NONE', #48061, 2.165354330708661568 ) ;
#16627 = VECTOR ( 'NONE', #42555, 39.37007874015748143 ) ;
#16628 = CARTESIAN_POINT ( 'NONE',  ( 1.345337514773771614, 0.1411726943947604063, -0.7317238754971229220 ) ) ;
#16629 = EDGE_CURVE ( 'NONE', #21355, #47803, #23217, .T. ) ;
#16630 = EDGE_LOOP ( 'NONE', ( #40509, #11986, #43628, #3394 ) ) ;
#16631 = CARTESIAN_POINT ( 'NONE',  ( 2.009930929872536964, 6.692913385826772199, -0.8055662819783819817 ) ) ;
#16632 = ADVANCED_FACE ( 'NONE', ( #12365 ), #19338, .F. ) ;
#16633 = DIRECTION ( 'NONE',  ( 1.734723475976806848E-16, -0.000000000000000000, 1.000000000000000000 ) ) ;
#16634 = LINE ( 'NONE', #24114, #9816 ) ;
#16636 = EDGE_CURVE ( 'NONE', #5850, #3960, #43336, .T. ) ;
#16635 = ORIENTED_EDGE ( 'NONE', *, *, #12906, .F. ) ;
#16637 = LINE ( 'NONE', #48079, #26754 ) ;
#16638 = CARTESIAN_POINT ( 'NONE',  ( 1.363819533518803251, 0.000000000000000000, -0.1574803149606304187 ) ) ;
#16639 = B_SPLINE_CURVE_WITH_KNOTS ( 'NONE', 3,
 ( #23035, #22530, #18407, #6543 ),
 .UNSPECIFIED., .F., .F.,
 ( 4, 4 ),
 ( 0.1211873102087489551, 0.1625992483279400103 ),
 .UNSPECIFIED. ) ;
#16640 = CARTESIAN_POINT ( 'NONE',  ( 2.607952947267827781, 1.454965125674436921, 1.384780731079769289 ) ) ;
#16641 = VERTEX_POINT ( 'NONE', #16502 ) ;
#16642 = CARTESIAN_POINT ( 'NONE',  ( 1.560669927219590747, 0.000000000000000000, 0.4724409448818871482 ) ) ;
#16643 = CARTESIAN_POINT ( 'NONE',  ( -0.2727639067037608278, 3.267716535433071279, 0.2755905511810995412 ) ) ;
#16644 = EDGE_LOOP ( 'NONE', ( #24353, #37226, #34620, #35102, #40173 ) ) ;
#16645 = PLANE ( 'NONE',  #20428 ) ;
#16646 = DIRECTION ( 'NONE',  ( -1.000000000000000000, 0.000000000000000000, 0.000000000000000000 ) ) ;
#16647 = DIRECTION ( 'NONE',  ( 1.283101021437938170E-16, 1.000000000000000000, 1.154811821032258155E-17 ) ) ;
#16648 = DIRECTION ( 'NONE',  ( -0.000000000000000000, 1.000000000000000000, -0.000000000000000000 ) ) ;
#16649 = EDGE_CURVE ( 'NONE', #49792, #44687, #368, .T. ) ;
#16650 = ORIENTED_EDGE ( 'NONE', *, *, #46539, .F. ) ;
#16651 = ORIENTED_EDGE ( 'NONE', *, *, #29468, .T. ) ;
#16652 = LINE ( 'NONE', #48096, #17470 ) ;
#16653 = DIRECTION ( 'NONE',  ( -1.000000000000000000, -0.000000000000000000, -0.000000000000000000 ) ) ;
#16654 = VERTEX_POINT ( 'NONE', #23726 ) ;
#16655 = FACE_OUTER_BOUND ( 'NONE', #35772, .T. ) ;
#16656 = FACE_OUTER_BOUND ( 'NONE', #5341, .T. ) ;
#16657 = CARTESIAN_POINT ( 'NONE',  ( 0.2431224069212723493, 0.000000000000000000, 2.152304290637673034 ) ) ;
#16658 = VECTOR ( 'NONE', #9897, 39.37007874015748143 ) ;
#16659 = EDGE_CURVE ( 'NONE', #50326, #46463, #32253, .T. ) ;
#16660 = DIRECTION ( 'NONE',  ( 0.000000000000000000, 0.000000000000000000, -1.000000000000000000 ) ) ;
#16661 = ORIENTED_EDGE ( 'NONE', *, *, #12734, .F. ) ;
#16662 = VECTOR ( 'NONE', #17610, 39.37007874015748143 ) ;
#16663 = ORIENTED_EDGE ( 'NONE', *, *, #7847, .F. ) ;
#16664 = DIRECTION ( 'NONE',  ( -0.000000000000000000, -1.000000000000000000, -0.000000000000000000 ) ) ;
#16665 = LINE ( 'NONE', #44269, #236 ) ;
#16666 = CARTESIAN_POINT ( 'NONE',  ( -0.8329809839909438907, 1.607838722253305486, -2.833254665166566877 ) ) ;
#16667 = EDGE_CURVE ( 'NONE', #5831, #32813, #31233, .T. ) ;
#16668 = EDGE_CURVE ( 'NONE', #19099, #25200, #31740, .T. ) ;
#16669 = DIRECTION ( 'NONE',  ( -3.469446951953613696E-16, 0.000000000000000000, -1.000000000000000000 ) ) ;
#16670 = AXIS2_PLACEMENT_3D ( 'NONE', #38059, #22805, #2675 ) ;
#16671 = FACE_BOUND ( 'NONE', #6621, .T. ) ;
#16672 = ORIENTED_EDGE ( 'NONE', *, *, #2407, .T. ) ;
#16673 = LINE ( 'NONE', #16414, #5122 ) ;
#16674 = ORIENTED_EDGE ( 'NONE', *, *, #15085, .T. ) ;
#16675 = ORIENTED_EDGE ( 'NONE', *, *, #3579, .T. ) ;
#16676 = DIRECTION ( 'NONE',  ( 0.4338837391175526803, 0.000000000000000000, 0.9009688679024218105 ) ) ;
#16677 = VECTOR ( 'NONE', #23408, 39.37007874015748143 ) ;
#16678 = ORIENTED_EDGE ( 'NONE', *, *, #26324, .F. ) ;
#16679 = ORIENTED_EDGE ( 'NONE', *, *, #18637, .F. ) ;
#16680 = FACE_OUTER_BOUND ( 'NONE', #27073, .T. ) ;
#16681 = ORIENTED_EDGE ( 'NONE', *, *, #45364, .T. ) ;
#16682 = DIRECTION ( 'NONE',  ( -1.000000000000000000, 0.000000000000000000, 1.734723475976806848E-16 ) ) ;
#16683 = DIRECTION ( 'NONE',  ( 0.000000000000000000, 1.000000000000000000, 0.000000000000000000 ) ) ;
#16684 = CARTESIAN_POINT ( 'NONE',  ( -1.613340714851948965, 1.583636149837539975, -1.474425128113891814 ) ) ;
#16685 = FACE_OUTER_BOUND ( 'NONE', #35946, .T. ) ;
#16686 = CARTESIAN_POINT ( 'NONE',  ( 0.1968503937007873017, 0.000000000000000000, -0.3149606299212591165 ) ) ;
#16687 = DIRECTION ( 'NONE',  ( -1.000000000000000000, -0.000000000000000000, -0.000000000000000000 ) ) ;
#16688 = ORIENTED_EDGE ( 'NONE', *, *, #31051, .T. ) ;
#16689 = LINE ( 'NONE', #39663, #48017 ) ;
#16690 = DIRECTION ( 'NONE',  ( 0.000000000000000000, 1.000000000000000000, 0.000000000000000000 ) ) ;
#16691 = FACE_OUTER_BOUND ( 'NONE', #17293, .T. ) ;
#16692 = VERTEX_POINT ( 'NONE', #43591 ) ;
#16693 = VECTOR ( 'NONE', #21943, 39.37007874015748143 ) ;
#16694 = DIRECTION ( 'NONE',  ( -0.000000000000000000, 0.000000000000000000, 1.000000000000000000 ) ) ;
#16695 = EDGE_CURVE ( 'NONE', #44838, #14018, #12114, .T. ) ;
#16696 = LINE ( 'NONE', #41966, #27723 ) ;
#16697 = ORIENTED_EDGE ( 'NONE', *, *, #21784, .F. ) ;
#16698 = LINE ( 'NONE', #32453, #48499 ) ;
#16699 = EDGE_CURVE ( 'NONE', #38704, #6398, #39736, .T. ) ;
#16700 = DIRECTION ( 'NONE',  ( -1.000000000000000000, 0.000000000000000000, 0.000000000000000000 ) ) ;
#16701 = EDGE_CURVE ( 'NONE', #30309, #43045, #43077, .T. ) ;
#16702 = CARTESIAN_POINT ( 'NONE',  ( 0.000000000000000000, 0.000000000000000000, 0.000000000000000000 ) ) ;
#16703 = AXIS2_PLACEMENT_3D ( 'NONE', #28840, #20326, #1225 ) ;
#16704 = VERTEX_POINT ( 'NONE', #43845 ) ;
#16705 = VECTOR ( 'NONE', #34005, 39.37007874015748143 ) ;
#16706 = LINE ( 'NONE', #694, #17512 ) ;
#16707 = ORIENTED_EDGE ( 'NONE', *, *, #23268, .T. ) ;
#16708 = FACE_BOUND ( 'NONE', #41332, .T. ) ;
#16709 = CARTESIAN_POINT ( 'NONE',  ( 1.363819533518803029, 3.267716535433071279, -1.605145679676863724 ) ) ;
#16710 = EDGE_CURVE ( 'NONE', #31458, #1749, #47692, .T. ) ;
#16711 = AXIS2_PLACEMENT_3D ( 'NONE', #29781, #25906, #17319 ) ;
#16712 = CARTESIAN_POINT ( 'NONE',  ( 0.3734705886643994721, -0.6299212598425202314, -0.02018660888377523527 ) ) ;
#16713 = CARTESIAN_POINT ( 'NONE',  ( 0.7423782071083087075, 3.267716535433071279, -6.146657985744592735E-16 ) ) ;
#16714 = ORIENTED_EDGE ( 'NONE', *, *, #30239, .T. ) ;
#16715 = EDGE_LOOP ( 'NONE', ( #4791, #28026, #46931, #30637 ) ) ;
#16716 = DIRECTION ( 'NONE',  ( 1.000000000000000000, -0.000000000000000000, 0.000000000000000000 ) ) ;
#16717 = ORIENTED_EDGE ( 'NONE', *, *, #96, .F. ) ;
#16718 = ADVANCED_FACE ( 'NONE', ( #51037 ), #16244, .F. ) ;
#16719 = LINE ( 'NONE', #32211, #41757 ) ;
#16720 = ORIENTED_EDGE ( 'NONE', *, *, #13837, .T. ) ;
#16721 = CARTESIAN_POINT ( 'NONE',  ( 0.4696143004045478242, 3.267716535433071279, -1.629301903132387013E-16 ) ) ;
#16722 = EDGE_CURVE ( 'NONE', #39361, #41791, #31703, .T. ) ;
#16723 = ORIENTED_EDGE ( 'NONE', *, *, #28121, .T. ) ;
#16724 = CARTESIAN_POINT ( 'NONE',  ( 2.253340778107071785, 1.711184928431753294, -0.5647885202703215590 ) ) ;
#16725 = ADVANCED_FACE ( 'NONE', ( #47180 ), #32513, .F. ) ;
#16726 = LINE ( 'NONE', #25477, #2577 ) ;
#16727 = VERTEX_POINT ( 'NONE', #44108 ) ;
#16728 = EDGE_CURVE ( 'NONE', #39348, #30279, #17018, .T. ) ;
#16729 = CARTESIAN_POINT ( 'NONE',  ( -0.04921259842519708216, 1.616260271943668503, 2.716073891007743324 ) ) ;
#16730 = ORIENTED_EDGE ( 'NONE', *, *, #37827, .T. ) ;
#16731 = EDGE_CURVE ( 'NONE', #1644, #37208, #24503, .T. ) ;
#16732 = CARTESIAN_POINT ( 'NONE',  ( 0.2727639067037607168, 3.267716535433071279, -4.731699523581612206E-17 ) ) ;
#16733 = ORIENTED_EDGE ( 'NONE', *, *, #11105, .T. ) ;
#16734 = ORIENTED_EDGE ( 'NONE', *, *, #33166, .T. ) ;
#16735 = CARTESIAN_POINT ( 'NONE',  ( -1.909347346926324906, 3.346456692913386100, -0.6692913385826758654 ) ) ;
#16736 = VECTOR ( 'NONE', #13045, 39.37007874015748143 ) ;
#16737 = ORIENTED_EDGE ( 'NONE', *, *, #8838, .T. ) ;
#16738 = CARTESIAN_POINT ( 'NONE',  ( 0.07982360342473591996, 1.709180471932028711, 0.000000000000000000 ) ) ;
#16739 = EDGE_LOOP ( 'NONE', ( #3649, #22014, #21220, #31254 ) ) ;
#16740 = CARTESIAN_POINT ( 'NONE',  ( -2.121469926805683137, 5.905511811023623991, -0.4337334748181712052 ) ) ;
#16741 = VECTOR ( 'NONE', #41632, 39.37007874015748143 ) ;
#16742 = AXIS2_PLACEMENT_3D ( 'NONE', #1504, #5376, #48444 ) ;
#16743 = CARTESIAN_POINT ( 'NONE',  ( 0.7423782071083087075, 0.000000000000000000, -0.3149606299212593941 ) ) ;
#16744 = CARTESIAN_POINT ( 'NONE',  ( -0.07591351300297333182, 0.000000000000000000, -0.4724409448818883694 ) ) ;
#16745 = VERTEX_POINT ( 'NONE', #40506 ) ;
#16746 = CARTESIAN_POINT ( 'NONE',  ( -0.3486774197067339376, 3.346456692913386100, 2.204724409448808764 ) ) ;
#16747 = DIRECTION ( 'NONE',  ( -0.000000000000000000, 1.000000000000000000, -0.000000000000000000 ) ) ;
#16748 = AXIS2_PLACEMENT_3D ( 'NONE', #44544, #24691, #39921 ) ;
#16749 = CARTESIAN_POINT ( 'NONE',  ( -2.182111253630085734, 3.346456692913386100, -0.6299212598425177889 ) ) ;
#16750 = CARTESIAN_POINT ( 'NONE',  ( -1.721400284384397628, 0.0003482895740541699209, 0.2828415639128913361 ) ) ;
#16751 = CARTESIAN_POINT ( 'NONE',  ( 0.000000000000000000, 3.267716535433071279, -2.244094488188969283 ) ) ;
#16752 = CARTESIAN_POINT ( 'NONE',  ( -1.544727076607844474, 0.5249316497054296038, -1.078632795961144364 ) ) ;
#16753 = CARTESIAN_POINT ( 'NONE',  ( 0.000000000000000000, 6.692913385826772199, 0.000000000000000000 ) ) ;
#16754 = ORIENTED_EDGE ( 'NONE', *, *, #37444, .T. ) ;
#16755 = CARTESIAN_POINT ( 'NONE',  ( 0.5455278134075212115, 0.000000000000000000, -0.3149606299212593941 ) ) ;
#16756 = CARTESIAN_POINT ( 'NONE',  ( -1.266372989455463172, 1.699517224488781064, -2.667458714000412456 ) ) ;
#16757 = EDGE_CURVE ( 'NONE', #34628, #48087, #5894, .T. ) ;
#16758 = ORIENTED_EDGE ( 'NONE', *, *, #29349, .T. ) ;
#16759 = DIRECTION ( 'NONE',  ( 1.734723475976806848E-16, 0.000000000000000000, 1.000000000000000000 ) ) ;
#16760 = EDGE_CURVE ( 'NONE', #50682, #35324, #44608, .T. ) ;
#16761 = ORIENTED_EDGE ( 'NONE', *, *, #16722, .T. ) ;
#16762 = EDGE_CURVE ( 'NONE', #47284, #27651, #33538, .T. ) ;
#16763 = CARTESIAN_POINT ( 'NONE',  ( -0.6214413264104939882, 3.346456692913386100, 1.732283464566921172 ) ) ;
#16764 = DIRECTION ( 'NONE',  ( 0.000000000000000000, 0.000000000000000000, -1.000000000000000000 ) ) ;
#16765 = DIRECTION ( 'NONE',  ( 0.000000000000000000, 0.000000000000000000, -1.000000000000000000 ) ) ;
#16766 = LINE ( 'NONE', #44373, #21940 ) ;
#16767 = ORIENTED_EDGE ( 'NONE', *, *, #7225, .T. ) ;
#16768 = B_SPLINE_CURVE_WITH_KNOTS ( 'NONE', 3,
 ( #18539, #23928, #20038, #43534 ),
 .UNSPECIFIED., .F., .F.,
 ( 4, 4 ),
 ( 1.192911306398316375E-06, 0.004936895822257959809 ),
 .UNSPECIFIED. ) ;
#16769 = CARTESIAN_POINT ( 'NONE',  ( -0.07591351300297340121, 0.000000000000000000, -1.614173228346451605 ) ) ;
#16770 = VECTOR ( 'NONE', #21174, 39.37007874015748143 ) ;
#16771 = FACE_BOUND ( 'NONE', #13285, .T. ) ;
#16772 = VERTEX_POINT ( 'NONE', #21140 ) ;
#16773 = DIRECTION ( 'NONE',  ( -1.000000000000000000, -0.000000000000000000, -0.000000000000000000 ) ) ;
#16774 = VECTOR ( 'NONE', #21587, 39.37007874015748143 ) ;
#16775 = ORIENTED_EDGE ( 'NONE', *, *, #44892, .F. ) ;
#16776 = VECTOR ( 'NONE', #39258, 39.37007874015748143 ) ;
#16777 = LINE ( 'NONE', #41041, #9548 ) ;
#16778 = CARTESIAN_POINT ( 'NONE',  ( 2.473328170512036461, 1.659322169655358836, -1.612973743992607956 ) ) ;
#16779 = EDGE_CURVE ( 'NONE', #44880, #32877, #17518, .T. ) ;
#16780 = AXIS2_PLACEMENT_3D ( 'NONE', #42948, #50652, #39093 ) ;
#16781 = DIRECTION ( 'NONE',  ( -0.9998717552508121775, -0.01601477604151182316, 0.000000000000000000 ) ) ;
#16782 = EDGE_CURVE ( 'NONE', #13301, #20798, #28619, .T. ) ;
#16783 = VERTEX_POINT ( 'NONE', #12885 ) ;
#16784 = EDGE_LOOP ( 'NONE', ( #20113, #31160, #23305, #16217 ) ) ;
#16785 = ADVANCED_FACE ( 'NONE', ( #36378 ), #33279, .T. ) ;
#16786 = PLANE ( 'NONE',  #5377 ) ;
#16787 = PLANE ( 'NONE',  #14967 ) ;
#16788 = FACE_BOUND ( 'NONE', #7599, .T. ) ;
#16789 = DIRECTION ( 'NONE',  ( 0.01601477604151182663, -0.9998717552508123996, 0.000000000000000000 ) ) ;
#16790 = CARTESIAN_POINT ( 'NONE',  ( -0.5455278134075214336, 0.000000000000000000, -0.9448818897637762948 ) ) ;
#16791 = EDGE_LOOP ( 'NONE', ( #23300, #5776, #35720, #13622 ) ) ;
#16792 = DIRECTION ( 'NONE',  ( -3.469446951953613696E-16, 0.000000000000000000, -1.000000000000000000 ) ) ;
#16793 = EDGE_LOOP ( 'NONE', ( #47794, #32393, #48114, #40746 ) ) ;
#16794 = ORIENTED_EDGE ( 'NONE', *, *, #21784, .T. ) ;
#16795 = ORIENTED_EDGE ( 'NONE', *, *, #38343, .T. ) ;
#16796 = CARTESIAN_POINT ( 'NONE',  ( 0.000000000000000000, 3.267716535433071279, 0.5905511811023582691 ) ) ;
#16797 = CARTESIAN_POINT ( 'NONE',  ( 0.2184225803664230636, 0.02091578714757513086, -1.877866740686216618 ) ) ;
#16798 = DIRECTION ( 'NONE',  ( 1.000000000000000000, 0.000000000000000000, -3.469446951953613696E-16 ) ) ;
#16799 = CARTESIAN_POINT ( 'NONE',  ( 2.298430379965446857, 1.646290322915411997, 0.3610056012771685197 ) ) ;
#16800 = EDGE_LOOP ( 'NONE', ( #43859, #43943, #32468 ) ) ;
#16801 = ORIENTED_EDGE ( 'NONE', *, *, #32804, .F. ) ;
#16802 = VECTOR ( 'NONE', #22071, 39.37007874015748854 ) ;
#16803 = FACE_OUTER_BOUND ( 'NONE', #27434, .T. ) ;
#16804 = DIRECTION ( 'NONE',  ( 1.734723475976806848E-16, -0.000000000000000000, 1.000000000000000000 ) ) ;
#16805 = PLANE ( 'NONE',  #22484 ) ;
#16806 = CIRCLE ( 'NONE', #15983, 1.743387098533651480 ) ;
#16807 = DIRECTION ( 'NONE',  ( -1.000000000000000000, 0.000000000000000000, 0.000000000000000000 ) ) ;
#16808 = VECTOR ( 'NONE', #5280, 39.37007874015748143 ) ;
#16809 = FACE_OUTER_BOUND ( 'NONE', #13096, .T. ) ;
#16810 = VECTOR ( 'NONE', #31533, 39.37007874015748143 ) ;
#16811 = CARTESIAN_POINT ( 'NONE',  ( -1.062992125984251857, 0.4235180831842794702, 1.229331597148918448E-16 ) ) ;
#16812 = FACE_OUTER_BOUND ( 'NONE', #8830, .T. ) ;
#16813 = DIRECTION ( 'NONE',  ( 0.000000000000000000, 0.000000000000000000, 1.000000000000000000 ) ) ;
#16814 = AXIS2_PLACEMENT_3D ( 'NONE', #38968, #27594, #3602 ) ;
#16815 = ORIENTED_EDGE ( 'NONE', *, *, #41862, .T. ) ;
#16816 = LINE ( 'NONE', #20675, #22603 ) ;
#16817 = CARTESIAN_POINT ( 'NONE',  ( -1.909347346926324906, 3.346456692913386100, 1.417322834645662333 ) ) ;
#16818 = EDGE_CURVE ( 'NONE', #16904, #16878, #29390, .T. ) ;
#16819 = ORIENTED_EDGE ( 'NONE', *, *, #7952, .F. ) ;
#16820 = ADVANCED_FACE ( 'NONE', ( #9009, #32777 ), #9776, .T. ) ;
#16821 = PRODUCT_DEFINITION ( 'UNKNOWN', '', #45664, #6589 ) ;
#16822 = VERTEX_POINT ( 'NONE', #33028 ) ;
#16823 = FACE_OUTER_BOUND ( 'NONE', #30437, .T. ) ;
#16824 = DIRECTION ( 'NONE',  ( -1.000000000000000000, 0.000000000000000000, 1.734723475976806848E-16 ) ) ;
#16825 = LINE ( 'NONE', #32581, #13976 ) ;
#16826 = EDGE_CURVE ( 'NONE', #45425, #39932, #17271, .T. ) ;
#16827 = ORIENTED_EDGE ( 'NONE', *, *, #31487, .F. ) ;
#16828 = EDGE_CURVE ( 'NONE', #43386, #43398, #5131, .T. ) ;
#16829 = ORIENTED_EDGE ( 'NONE', *, *, #13202, .F. ) ;
#16830 = PLANE ( 'NONE',  #27068 ) ;
#16831 = ORIENTED_EDGE ( 'NONE', *, *, #49999, .T. ) ;
#16832 = VERTEX_POINT ( 'NONE', #41022 ) ;
#16833 = DIRECTION ( 'NONE',  ( 1.734723475976806848E-16, 0.000000000000000000, 1.000000000000000000 ) ) ;
#16834 = LINE ( 'NONE', #37224, #30521 ) ;
#16835 = CARTESIAN_POINT ( 'NONE',  ( -0.9602959360900468200, 0.01253876862113688373, 1.511314840084332145 ) ) ;
#16836 = EDGE_CURVE ( 'NONE', #16203, #10796, #36896, .T. ) ;
#16837 = ORIENTED_EDGE ( 'NONE', *, *, #6917, .F. ) ;
#16838 = AXIS2_PLACEMENT_3D ( 'NONE', #34883, #11637, #3384 ) ;
#16839 = ORIENTED_EDGE ( 'NONE', *, *, #43029, .T. ) ;
#16840 = EDGE_LOOP ( 'NONE', ( #29298, #49543, #18667, #37077 ) ) ;
#16841 = CARTESIAN_POINT ( 'NONE',  ( 2.695799277629594037, 1.761268146152256575, -1.205759334241453651 ) ) ;
#16842 = VECTOR ( 'NONE', #43517, 39.37007874015748143 ) ;
#16843 = ORIENTED_EDGE ( 'NONE', *, *, #20707, .F. ) ;
#16844 = ORIENTED_EDGE ( 'NONE', *, *, #34860, .T. ) ;
#16845 = EDGE_CURVE ( 'NONE', #39563, #9387, #30291, .T. ) ;
#16846 = AXIS2_PLACEMENT_3D ( 'NONE', #33394, #48318, #25119 ) ;
#16847 = CARTESIAN_POINT ( 'NONE',  ( -1.062992125984250968, 0.4724409448818890911, 1.181102362204724088 ) ) ;
#16848 = LINE ( 'NONE', #44194, #22775 ) ;
#16849 = CARTESIAN_POINT ( 'NONE',  ( 0.1155636338427008941, -0.5222242541845523167, 0.000000000000000000 ) ) ;
#16850 = AXIS2_PLACEMENT_3D ( 'NONE', #39885, #4516, #20255 ) ;
#16851 = VECTOR ( 'NONE', #15977, 39.37007874015748143 ) ;
#16852 = ORIENTED_EDGE ( 'NONE', *, *, #50110, .T. ) ;
#16853 = PLANE ( 'NONE',  #27098 ) ;
#16854 = DIRECTION ( 'NONE',  ( -0.000000000000000000, 1.000000000000000000, -0.000000000000000000 ) ) ;
#16855 = EDGE_CURVE ( 'NONE', #10381, #1302, #49997, .T. ) ;
#16856 = LINE ( 'NONE', #13741, #45110 ) ;
#16857 = ORIENTED_EDGE ( 'NONE', *, *, #605, .F. ) ;
#16858 = CARTESIAN_POINT ( 'NONE',  ( 2.158170387640339527, 5.905511811023623991, 0.2426819907294804068 ) ) ;
#16859 = DIRECTION ( 'NONE',  ( -3.469446951953613696E-16, 0.000000000000000000, -1.000000000000000000 ) ) ;
#16860 = VECTOR ( 'NONE', #8240, 39.37007874015748143 ) ;
#16861 = DIRECTION ( 'NONE',  ( 1.734723475976806848E-16, 0.000000000000000000, 1.000000000000000000 ) ) ;
#16862 = VERTEX_POINT ( 'NONE', #36633 ) ;
#16863 = ORIENTED_EDGE ( 'NONE', *, *, #15962, .T. ) ;
#16864 = CARTESIAN_POINT ( 'NONE',  ( 0.000000000000000000, 5.905511811023623991, 0.000000000000000000 ) ) ;
#16865 = DIRECTION ( 'NONE',  ( 1.000000000000000000, 0.000000000000000000, 0.000000000000000000 ) ) ;
#16866 = EDGE_CURVE ( 'NONE', #49288, #41994, #44863, .T. ) ;
#16867 = PLANE ( 'NONE',  #9917 ) ;
#16868 = DIRECTION ( 'NONE',  ( -3.469446951953613696E-16, 0.000000000000000000, -1.000000000000000000 ) ) ;
#16869 = FACE_OUTER_BOUND ( 'NONE', #13462, .T. ) ;
#16870 = ORIENTED_EDGE ( 'NONE', *, *, #19711, .T. ) ;
#16871 = ORIENTED_EDGE ( 'NONE', *, *, #27918, .T. ) ;
#16872 = CARTESIAN_POINT ( 'NONE',  ( -1.091055626815042201, 0.000000000000000000, 0.6299212598425164567 ) ) ;
#16873 = ORIENTED_EDGE ( 'NONE', *, *, #25807, .F. ) ;
#16874 = DIRECTION ( 'NONE',  ( 0.000000000000000000, -1.000000000000000000, 0.000000000000000000 ) ) ;
#16875 = DIRECTION ( 'NONE',  ( 0.000000000000000000, 0.000000000000000000, 1.000000000000000000 ) ) ;
#16876 = DIRECTION ( 'NONE',  ( -0.000000000000000000, -1.000000000000000000, -0.000000000000000000 ) ) ;
#16877 = DIRECTION ( 'NONE',  ( -3.469446951953613696E-16, 0.000000000000000000, -1.000000000000000000 ) ) ;
#16878 = VERTEX_POINT ( 'NONE', #47056 ) ;
#16879 = AXIS2_PLACEMENT_3D ( 'NONE', #12476, #23588, #16875 ) ;
#16880 = CARTESIAN_POINT ( 'NONE',  ( 0.000000000000000000, 3.267716535433071279, 1.377952755905504256 ) ) ;
#16881 = AXIS2_PLACEMENT_3D ( 'NONE', #6264, #14258, #45472 ) ;
#16882 = DIRECTION ( 'NONE',  ( -3.469446951953613696E-16, 0.000000000000000000, -1.000000000000000000 ) ) ;
#16883 = VECTOR ( 'NONE', #20628, 39.37007874015748143 ) ;
#16884 = EDGE_CURVE ( 'NONE', #33629, #29961, #2848, .T. ) ;
#16885 = AXIS2_PLACEMENT_3D ( 'NONE', #13898, #5891, #42026 ) ;
#16886 = EDGE_LOOP ( 'NONE', ( #12588, #47788, #14826, #22259 ) ) ;
#16887 = DIRECTION ( 'NONE',  ( 1.734723475976806848E-16, -0.000000000000000000, 1.000000000000000000 ) ) ;
#16888 = DIRECTION ( 'NONE',  ( -0.9998717552508122886, -0.01601477604151182316, 0.000000000000000000 ) ) ;
#16889 = CARTESIAN_POINT ( 'NONE',  ( -0.4349608091551073197, 1.574803149606302854, 2.121218629000295230 ) ) ;
#16890 = ORIENTED_EDGE ( 'NONE', *, *, #20272, .F. ) ;
#16891 = CARTESIAN_POINT ( 'NONE',  ( -1.363819533518803029, 3.267716535433071279, 0.7874015748031456541 ) ) ;
#16892 = EDGE_CURVE ( 'NONE', #31439, #17089, #26964, .T. ) ;
#16893 = DIRECTION ( 'NONE',  ( -1.000000000000000000, 0.000000000000000000, -0.000000000000000000 ) ) ;
#16894 = AXIS2_PLACEMENT_3D ( 'NONE', #43880, #36163, #4401 ) ;
#16895 = ORIENTED_EDGE ( 'NONE', *, *, #20368, .T. ) ;
#16896 = CARTESIAN_POINT ( 'NONE',  ( 1.300279662861326013, 0.04874602395362847423, 1.413491677621213860 ) ) ;
#16897 = CARTESIAN_POINT ( 'NONE',  ( 2.182111253630085290, 0.000000000000000000, 0.1181102362204698858 ) ) ;
#16898 = VERTEX_POINT ( 'NONE', #49470 ) ;
#16899 = CARTESIAN_POINT ( 'NONE',  ( 0.04921259842519667277, 5.905511811023623991, 2.952755905511811108 ) ) ;
#16900 = DIRECTION ( 'NONE',  ( 1.000000000000000000, 0.000000000000000000, 0.000000000000000000 ) ) ;
#16901 = DIRECTION ( 'NONE',  ( -3.469446951953613696E-16, 0.000000000000000000, -1.000000000000000000 ) ) ;
#16902 = PLANE ( 'NONE',  #33460 ) ;
#16903 = DIRECTION ( 'NONE',  ( 1.000000000000000000, -0.000000000000000000, 0.000000000000000000 ) ) ;
#16904 = VERTEX_POINT ( 'NONE', #19470 ) ;
#16905 = ORIENTED_EDGE ( 'NONE', *, *, #22087, .T. ) ;
#16906 = CARTESIAN_POINT ( 'NONE',  ( -0.8329809839909435576, 5.905511811023624880, -2.833254665166567321 ) ) ;
#16907 = CARTESIAN_POINT ( 'NONE',  ( -1.091055626815042645, 0.000000000000000000, 2.007874015748021268 ) ) ;
#16908 = EDGE_LOOP ( 'NONE', ( #40637, #35884 ) ) ;
#16909 = CARTESIAN_POINT ( 'NONE',  ( 1.556712866041120247, 1.480457248723645591, 2.509548638715870084 ) ) ;
#16910 = FACE_OUTER_BOUND ( 'NONE', #23700, .T. ) ;
#16911 = CARTESIAN_POINT ( 'NONE',  ( -0.5455278134075214336, 3.346456692913386100, 2.204724409448808764 ) ) ;
#16912 = LINE ( 'NONE', #4777, #12486 ) ;
#16913 = ORIENTED_EDGE ( 'NONE', *, *, #1761, .F. ) ;
#16914 = ORIENTED_EDGE ( 'NONE', *, *, #17339, .T. ) ;
#16915 = CARTESIAN_POINT ( 'NONE',  ( 2.932638728931774352, 1.205361022782829114E-17, 0.3475908556738223631 ) ) ;
#16916 = DIRECTION ( 'NONE',  ( 1.000000000000000000, -0.000000000000000000, 0.000000000000000000 ) ) ;
#16917 = ADVANCED_FACE ( 'NONE', ( #7361 ), #23600, .F. ) ;
#16918 = CARTESIAN_POINT ( 'NONE',  ( -0.04921259842519689481, 2.794703227806734062E-17, 1.924024829198930364 ) ) ;
#16919 = ORIENTED_EDGE ( 'NONE', *, *, #40220, .T. ) ;
#16920 = LINE ( 'NONE', #48620, #22402 ) ;
#16921 = FACE_BOUND ( 'NONE', #24720, .T. ) ;
#16922 = VECTOR ( 'NONE', #30269, 39.37007874015748143 ) ;
#16923 = EDGE_LOOP ( 'NONE', ( #30171, #48743, #2432, #41359 ) ) ;
#16924 = VECTOR ( 'NONE', #1201, 39.37007874015748143 ) ;
#16925 = LINE ( 'NONE', #40929, #169 ) ;
#16926 = AXIS2_PLACEMENT_3D ( 'NONE', #47173, #7720, #7229 ) ;
#16927 = ORIENTED_EDGE ( 'NONE', *, *, #16102, .F. ) ;
#16928 = ORIENTED_EDGE ( 'NONE', *, *, #26070, .F. ) ;
#16929 = DIRECTION ( 'NONE',  ( -1.509903313490212895E-14, 0.000000000000000000, 1.000000000000000000 ) ) ;
#16930 = EDGE_CURVE ( 'NONE', #35430, #34365, #50661, .T. ) ;
#16931 = AXIS2_PLACEMENT_3D ( 'NONE', #37609, #17722, #48912 ) ;
#16932 = EDGE_CURVE ( 'NONE', #35391, #5168, #39355, .T. ) ;
#16933 = ADVANCED_FACE ( 'NONE', ( #37661 ), #28372, .T. ) ;
#16934 = ORIENTED_EDGE ( 'NONE', *, *, #4587, .F. ) ;
#16935 = EDGE_LOOP ( 'NONE', ( #2885, #36332, #14696, #40585 ) ) ;
#16936 = DIRECTION ( 'NONE',  ( 1.142080616180681165E-16, -1.000000000000000000, -2.072570748943160811E-17 ) ) ;
#16937 = ORIENTED_EDGE ( 'NONE', *, *, #28417, .F. ) ;
#16938 = VECTOR ( 'NONE', #17914, 39.37007874015748143 ) ;
#16939 = EDGE_CURVE ( 'NONE', #37379, #7713, #3993, .T. ) ;
#16940 = CARTESIAN_POINT ( 'NONE',  ( -2.160844847978046879, 1.673297988508097855, 0.1614166014397402371 ) ) ;
#16941 = LINE ( 'NONE', #9184, #17870 ) ;
#16942 = CARTESIAN_POINT ( 'NONE',  ( 1.833791099076603537, 5.905511811023623991, -1.151507526013693994 ) ) ;
#16943 = ADVANCED_FACE ( 'NONE', ( #38853 ), #7773, .F. ) ;
#16944 =( BOUNDED_CURVE ( )  B_SPLINE_CURVE ( 3, ( #3344, #42323, #19085, #34841 ),
 .UNSPECIFIED., .F., .F. ) 
 B_SPLINE_CURVE_WITH_KNOTS ( ( 4, 4 ),
 ( 0.9053024471257524741, 0.9561597570633886267 ),
 .UNSPECIFIED. ) 
 CURVE ( )  GEOMETRIC_REPRESENTATION_ITEM ( )  RATIONAL_B_SPLINE_CURVE ( ( 1.000000000000000000, 0.9997844727828222311, 0.9997844727828222311, 1.000000000000000000 ) ) 
 REPRESENTATION_ITEM ( '' )  );
#16945 = FACE_OUTER_BOUND ( 'NONE', #11536, .T. ) ;
#16946 = LINE ( 'NONE', #9189, #18756 ) ;
#16947 = CARTESIAN_POINT ( 'NONE',  ( -1.363819533518803473, 3.346456692913386100, 1.850393700787392293 ) ) ;
#16948 = VERTEX_POINT ( 'NONE', #42956 ) ;
#16949 = CARTESIAN_POINT ( 'NONE',  ( 1.091055626815042645, 0.000000000000000000, -0.9448818897637765168 ) ) ;
#16950 = DIRECTION ( 'NONE',  ( -0.000000000000000000, 1.000000000000000000, -0.000000000000000000 ) ) ;
#16951 = EDGE_CURVE ( 'NONE', #25794, #46385, #13113, .T. ) ;
#16952 = VERTEX_POINT ( 'NONE', #18029 ) ;
#16953 = CARTESIAN_POINT ( 'NONE',  ( 0.2727639067037609943, 0.000000000000000000, 1.850393700787392293 ) ) ;
#16954 = CARTESIAN_POINT ( 'NONE',  ( -1.091055626815042201, 0.000000000000000000, 0.6299212598425164567 ) ) ;
#16955 = ORIENTED_EDGE ( 'NONE', *, *, #26597, .F. ) ;
#16956 = DIRECTION ( 'NONE',  ( 1.000000000000000000, 0.000000000000000000, 0.000000000000000000 ) ) ;
#16957 = CARTESIAN_POINT ( 'NONE',  ( 1.864846474276733890, 0.03794660422572829900, -0.7435542096351945851 ) ) ;
#16958 = EDGE_CURVE ( 'NONE', #13751, #14372, #31362, .T. ) ;
#16959 = DIRECTION ( 'NONE',  ( 0.000000000000000000, 0.000000000000000000, -1.000000000000000000 ) ) ;
#16960 = VECTOR ( 'NONE', #26766, 39.37007874015748143 ) ;
#16961 = VECTOR ( 'NONE', #13844, 39.37007874015748143 ) ;
#16962 = EDGE_LOOP ( 'NONE', ( #26984, #5696, #36821, #47285 ) ) ;
#16963 = DIRECTION ( 'NONE',  ( -0.000000000000000000, 1.000000000000000000, -0.000000000000000000 ) ) ;
#16964 = ORIENTED_EDGE ( 'NONE', *, *, #29827, .T. ) ;
#16965 = FACE_BOUND ( 'NONE', #3660, .T. ) ;
#16966 = CIRCLE ( 'NONE', #436, 1.743387098533651480 ) ;
#16967 = CARTESIAN_POINT ( 'NONE',  ( -0.5455278134075214336, 0.000000000000000000, 2.204724409448808764 ) ) ;
#16968 = CARTESIAN_POINT ( 'NONE',  ( -0.2727639067037607723, 3.346456692913386100, -0.7874015748031470974 ) ) ;
#16969 = CARTESIAN_POINT ( 'NONE',  ( -1.712496953225537188, 3.267716535433071279, 0.2755905511810996522 ) ) ;
#16970 = CIRCLE ( 'NONE', #6233, 2.165354330708661568 ) ;
#16971 = AXIS2_PLACEMENT_3D ( 'NONE', #19548, #16200, #35820 ) ;
#16972 = ORIENTED_EDGE ( 'NONE', *, *, #6261, .T. ) ;
#16973 = ORIENTED_EDGE ( 'NONE', *, *, #37872, .T. ) ;
#16974 = CARTESIAN_POINT ( 'NONE',  ( 1.909347346926324462, 0.000000000000000000, -1.102362204724406602 ) ) ;
#16975 = ORIENTED_EDGE ( 'NONE', *, *, #14123, .F. ) ;
#16976 = DIRECTION ( 'NONE',  ( -1.000000000000000000, -0.000000000000000000, -0.000000000000000000 ) ) ;
#16977 = VERTEX_POINT ( 'NONE', #7608 ) ;
#16978 = CARTESIAN_POINT ( 'NONE',  ( 2.734482843737263025, 0.000000000000000000, -1.115254632218672937 ) ) ;
#16979 = ORIENTED_EDGE ( 'NONE', *, *, #48524, .F. ) ;
#16980 = DIRECTION ( 'NONE',  ( -0.000000000000000000, 1.000000000000000000, -0.000000000000000000 ) ) ;
#16981 = CARTESIAN_POINT ( 'NONE',  ( -0.6382636202146998450, 1.632062195274633254, -2.127712142990381139 ) ) ;
#16982 = ORIENTED_EDGE ( 'NONE', *, *, #40231, .T. ) ;
#16983 = DIRECTION ( 'NONE',  ( -0.000000000000000000, 0.000000000000000000, 1.000000000000000000 ) ) ;
#16984 = EDGE_LOOP ( 'NONE', ( #17302, #21538, #27626, #45488, #10422 ) ) ;
#16985 = VERTEX_POINT ( 'NONE', #33791 ) ;
#16986 = EDGE_CURVE ( 'NONE', #45623, #21877, #25919, .T. ) ;
#16987 = EDGE_CURVE ( 'NONE', #46194, #8104, #10976, .T. ) ;
#16988 = ORIENTED_EDGE ( 'NONE', *, *, #16467, .F. ) ;
#16989 = VERTEX_POINT ( 'NONE', #11728 ) ;
#16990 = CARTESIAN_POINT ( 'NONE',  ( -2.182111253630085290, 3.346456692913386100, -0.3149606299212589500 ) ) ;
#16991 = ADVANCED_FACE ( 'NONE', ( #39103 ), #50914, .F. ) ;
#16992 = VECTOR ( 'NONE', #31539, 39.37007874015748143 ) ;
#16993 = CIRCLE ( 'NONE', #27650, 2.165354330708661568 ) ;
#16994 = ORIENTED_EDGE ( 'NONE', *, *, #27711, .T. ) ;
#16995 = CARTESIAN_POINT ( 'NONE',  ( 2.882374435144376079, 1.764165479168779527, -0.6410570582911828685 ) ) ;
#16996 = VECTOR ( 'NONE', #28001, 39.37007874015748143 ) ;
#16997 = ORIENTED_EDGE ( 'NONE', *, *, #46796, .T. ) ;
#16998 = DIRECTION ( 'NONE',  ( -0.000000000000000000, 1.000000000000000000, -0.000000000000000000 ) ) ;
#16999 = VECTOR ( 'NONE', #13998, 39.37007874015748143 ) ;
#17000 = LINE ( 'NONE', #29373, #3307 ) ;
#17001 = ORIENTED_EDGE ( 'NONE', *, *, #33219, .F. ) ;
#17002 = CIRCLE ( 'NONE', #46660, 2.165354330708661568 ) ;
#17003 = DIRECTION ( 'NONE',  ( 1.734723475976806848E-16, -0.000000000000000000, 1.000000000000000000 ) ) ;
#17004 = DIRECTION ( 'NONE',  ( 1.734723475976806848E-16, -0.000000000000000000, 1.000000000000000000 ) ) ;
#17005 = FACE_OUTER_BOUND ( 'NONE', #9614, .T. ) ;
#17006 = CARTESIAN_POINT ( 'NONE',  ( -1.722370577523733459, 1.205361022782829114E-17, 0.2829729990490794655 ) ) ;
#17007 = ADVANCED_FACE ( 'NONE', ( #22854 ), #38605, .F. ) ;
#17008 = CARTESIAN_POINT ( 'NONE',  ( 1.287906020515830141, 3.346456692913386100, 0.4330708661417287386 ) ) ;
#17009 = CARTESIAN_POINT ( 'NONE',  ( 2.475065961783442514, 0.9865970136139682323, 0.8559428686598158365 ) ) ;
#17010 = EDGE_CURVE ( 'NONE', #8152, #37129, #41519, .T. ) ;
#17011 = CARTESIAN_POINT ( 'NONE',  ( -1.004926760980926481, 0.000000000000000000, -0.6205843980233154422 ) ) ;
#17012 = ORIENTED_EDGE ( 'NONE', *, *, #34914, .T. ) ;
#17013 = DIRECTION ( 'NONE',  ( -0.9998717552508122886, -0.01601477604151180928, 0.000000000000000000 ) ) ;
#17014 = DIRECTION ( 'NONE',  ( -1.000000000000000000, 0.000000000000000000, 0.000000000000000000 ) ) ;
#17015 = EDGE_CURVE ( 'NONE', #39871, #48261, #31609, .T. ) ;
#17016 = B_SPLINE_CURVE_WITH_KNOTS ( 'NONE', 3,
 ( #30237, #5974, #45951, #29726 ),
 .UNSPECIFIED., .F., .F.,
 ( 4, 4 ),
 ( 2.655830146740026460E-07, 0.01938437877986225882 ),
 .UNSPECIFIED. ) ;
#17017 = VERTEX_POINT ( 'NONE', #28491 ) ;
#17018 = LINE ( 'NONE', #1765, #49785 ) ;
#17019 = EDGE_CURVE ( 'NONE', #29553, #36720, #39514, .T. ) ;
#17020 = ORIENTED_EDGE ( 'NONE', *, *, #24619, .T. ) ;
#17021 = LINE ( 'NONE', #45119, #21216 ) ;
#17022 = CARTESIAN_POINT ( 'NONE',  ( 0.4696143004045484348, 3.346456692913386100, 1.850393700787392293 ) ) ;
#17023 = DIRECTION ( 'NONE',  ( -0.000000000000000000, 0.000000000000000000, 1.000000000000000000 ) ) ;
#17024 = DIRECTION ( 'NONE',  ( 0.000000000000000000, -1.000000000000000000, 0.000000000000000000 ) ) ;
#17025 = DIRECTION ( 'NONE',  ( -3.469446951953613696E-16, 0.000000000000000000, -1.000000000000000000 ) ) ;
#17026 = VERTEX_POINT ( 'NONE', #8626 ) ;
#17027 = VECTOR ( 'NONE', #23027, 39.37007874015748143 ) ;
#17028 = LINE ( 'NONE', #13401, #29891 ) ;
#17029 = VECTOR ( 'NONE', #25488, 39.37007874015748143 ) ;
#17030 = DIRECTION ( 'NONE',  ( 0.000000000000000000, 0.000000000000000000, -1.000000000000000000 ) ) ;
#17031 = VECTOR ( 'NONE', #38392, 39.37007874015748143 ) ;
#17032 = ORIENTED_EDGE ( 'NONE', *, *, #49067, .F. ) ;
#17033 = CARTESIAN_POINT ( 'NONE',  ( -2.153807523435208093, 6.692913385826772199, 0.2420910006175677753 ) ) ;
#17034 = VECTOR ( 'NONE', #33177, 39.37007874015748143 ) ;
#17035 = ORIENTED_EDGE ( 'NONE', *, *, #27262, .F. ) ;
#17036 = PLANE ( 'NONE',  #10395 ) ;
#17037 = CARTESIAN_POINT ( 'NONE',  ( -1.326676825859837816, 1.205361022782829114E-17, -1.200346386814097999 ) ) ;
#17038 = AXIS2_PLACEMENT_3D ( 'NONE', #2959, #7087, #18954 ) ;
#17039 = FACE_OUTER_BOUND ( 'NONE', #18748, .T. ) ;
#17040 = VECTOR ( 'NONE', #47778, 39.37007874015748143 ) ;
#17041 = LINE ( 'NONE', #9029, #3261 ) ;
#17042 = ORIENTED_EDGE ( 'NONE', *, *, #9257, .T. ) ;
#17043 = ORIENTED_EDGE ( 'NONE', *, *, #38272, .T. ) ;
#17044 = DIRECTION ( 'NONE',  ( 0.000000000000000000, 0.6427876096865404731, 0.7660444431189771253 ) ) ;
#17045 = LINE ( 'NONE', #5919, #39691 ) ;
#17046 = CARTESIAN_POINT ( 'NONE',  ( -0.7053729475263578186, 3.346456692913386100, -2.047244094488181343 ) ) ;
#17047 = ORIENTED_EDGE ( 'NONE', *, *, #28973, .F. ) ;
#17048 = CARTESIAN_POINT ( 'NONE',  ( -1.636583440222564301, 3.267716535433071279, -0.9448818897637762948 ) ) ;
#17049 = LINE ( 'NONE', #44394, #35737 ) ;
#17050 = ORIENTED_EDGE ( 'NONE', *, *, #26066, .F. ) ;
#17051 = DIRECTION ( 'NONE',  ( 3.986037398843765983E-20, 1.000000000000000000, 1.160734090543304660E-16 ) ) ;
#17052 = ADVANCED_FACE ( 'NONE', ( #8878 ), #24634, .F. ) ;
#17053 = APPLICATION_CONTEXT ( 'automotive_design' ) ;
#17054 = ADVANCED_FACE ( 'NONE', ( #47824 ), #106, .F. ) ;
#17055 = CARTESIAN_POINT ( 'NONE',  ( -2.165354330708661568, 3.267716535433071279, -6.146657985744592735E-16 ) ) ;
#17056 = ORIENTED_EDGE ( 'NONE', *, *, #7473, .F. ) ;
#17057 = VERTEX_POINT ( 'NONE', #15850 ) ;
#17058 = EDGE_CURVE ( 'NONE', #15499, #38331, #1126, .T. ) ;
#17059 = ORIENTED_EDGE ( 'NONE', *, *, #9787, .T. ) ;
#17060 = LINE ( 'NONE', #8788, #40810 ) ;
#17061 = LINE ( 'NONE', #12926, #50500 ) ;
#17063 = CARTESIAN_POINT ( 'NONE',  ( 0.2727639067037604392, 0.000000000000000000, -0.6692913385826760875 ) ) ;
#17062 = VECTOR ( 'NONE', #14398, 39.37007874015748143 ) ;
#17064 = CARTESIAN_POINT ( 'NONE',  ( 0.4788131938641111973, 1.628272305554966159, 2.914091152102192162 ) ) ;
#17065 = ORIENTED_EDGE ( 'NONE', *, *, #42795, .F. ) ;
#17066 = ORIENTED_EDGE ( 'NONE', *, *, #22432, .F. ) ;
#17068 = VECTOR ( 'NONE', #16230, 39.37007874015748143 ) ;
#17067 = CARTESIAN_POINT ( 'NONE',  ( 1.833433833923351353, 0.000000000000000000, 0.7480314960629872445 ) ) ;
#17069 = CARTESIAN_POINT ( 'NONE',  ( 4.268512490100411402E-16, 0.000000000000000000, 1.889763779527550369 ) ) ;
#17070 = CARTESIAN_POINT ( 'NONE',  ( 1.530693736245518854, 1.574803149606302854, -1.531579597454043373 ) ) ;
#17071 = FACE_OUTER_BOUND ( 'NONE', #27136, .T. ) ;
#17072 = ADVANCED_FACE ( 'NONE', ( #12495 ), #35999, .F. ) ;
#17073 = CARTESIAN_POINT ( 'NONE',  ( 3.937007874015748143, 2.913385826771657250, 1.023622047244094446 ) ) ;
#17074 = AXIS2_PLACEMENT_3D ( 'NONE', #8090, #23324, #601 ) ;
#17075 = DIRECTION ( 'NONE',  ( -3.469446951953613696E-16, 0.000000000000000000, -1.000000000000000000 ) ) ;
#17076 = CIRCLE ( 'NONE', #2958, 0.3740157480314960647 ) ;
#17077 = EDGE_LOOP ( 'NONE', ( #49548, #5534, #21988, #3515 ) ) ;
#17078 = CARTESIAN_POINT ( 'NONE',  ( -0.4788131938641533858, 5.905511811023623991, 2.914091152102185944 ) ) ;
#17079 = FACE_OUTER_BOUND ( 'NONE', #18248, .T. ) ;
#17080 = EDGE_CURVE ( 'NONE', #975, #41895, #44453, .T. ) ;
#17081 = ORIENTED_EDGE ( 'NONE', *, *, #29852, .F. ) ;
#17082 = ORIENTED_EDGE ( 'NONE', *, *, #5961, .T. ) ;
#17083 = DIRECTION ( 'NONE',  ( -0.01601477604151182663, 0.9998717552508123996, -0.000000000000000000 ) ) ;
#17084 = LINE ( 'NONE', #13210, #20393 ) ;
#17085 = ORIENTED_EDGE ( 'NONE', *, *, #34584, .F. ) ;
#17086 = ORIENTED_EDGE ( 'NONE', *, *, #36115, .T. ) ;
#17087 = DIRECTION ( 'NONE',  ( 0.000000000000000000, -1.000000000000000000, 0.000000000000000000 ) ) ;
#17088 = ORIENTED_EDGE ( 'NONE', *, *, #43513, .T. ) ;
#17089 = VERTEX_POINT ( 'NONE', #12760 ) ;
#17090 = DIRECTION ( 'NONE',  ( 0.000000000000000000, 0.000000000000000000, 1.000000000000000000 ) ) ;
#17091 = CARTESIAN_POINT ( 'NONE',  ( 0.000000000000000000, 0.000000000000000000, 0.000000000000000000 ) ) ;
#17092 = VECTOR ( 'NONE', #44611, 39.37007874015748143 ) ;
#17093 = CIRCLE ( 'NONE', #573, 1.850107469027523432 ) ;
#17094 = EDGE_LOOP ( 'NONE', ( #35842, #14962, #40726, #14635 ) ) ;
#17095 = ORIENTED_EDGE ( 'NONE', *, *, #24879, .T. ) ;
#17096 = VERTEX_POINT ( 'NONE', #5008 ) ;
#17097 = AXIS2_PLACEMENT_3D ( 'NONE', #3214, #35221, #6598 ) ;
#17098 = CARTESIAN_POINT ( 'NONE',  ( -0.8182917201112814842, 0.000000000000000000, 1.417322834645662777 ) ) ;
#17099 = EDGE_LOOP ( 'NONE', ( #3381, #32596, #47249, #7209 ) ) ;
#17100 = VERTEX_POINT ( 'NONE', #11987 ) ;
#17101 = DIRECTION ( 'NONE',  ( -0.000000000000000000, 1.000000000000000000, -0.000000000000000000 ) ) ;
#17102 = DIRECTION ( 'NONE',  ( 0.000000000000000000, 0.000000000000000000, -1.000000000000000000 ) ) ;
#17103 = CARTESIAN_POINT ( 'NONE',  ( 2.622993961246840922, 1.756668590291742493, 0.8005172129084018318 ) ) ;
#17104 = ORIENTED_EDGE ( 'NONE', *, *, #18286, .F. ) ;
#17105 = CARTESIAN_POINT ( 'NONE',  ( 1.253212129322610613, 3.346456692913386100, 1.692913385826762873 ) ) ;
#17106 = CARTESIAN_POINT ( 'NONE',  ( 0.000000000000000000, 3.346456692913386100, 0.000000000000000000 ) ) ;
#17107 = LINE ( 'NONE', #37243, #40206 ) ;
#17108 = EDGE_LOOP ( 'NONE', ( #27254, #28187, #9087, #47038 ) ) ;
#17109 = DIRECTION ( 'NONE',  ( 3.986037398843765983E-20, 1.000000000000000000, 1.160734090543304660E-16 ) ) ;
#17110 = CARTESIAN_POINT ( 'NONE',  ( -0.04921259842519708216, 1.608688524157807498, 2.242709805336809303 ) ) ;
#17111 = EDGE_CURVE ( 'NONE', #19240, #11648, #24806, .T. ) ;
#17112 = EDGE_CURVE ( 'NONE', #40318, #18552, #39610, .T. ) ;
#17113 = LINE ( 'NONE', #16344, #27396 ) ;
#17114 = ORIENTED_EDGE ( 'NONE', *, *, #26495, .T. ) ;
#17115 = VERTEX_POINT ( 'NONE', #24375 ) ;
#17116 = LINE ( 'NONE', #43947, #23753 ) ;
#17117 = ADVANCED_FACE ( 'NONE', ( #31876 ), #12243, .T. ) ;
#17118 = DIRECTION ( 'NONE',  ( 0.000000000000000000, 0.000000000000000000, 1.000000000000000000 ) ) ;
#17119 = CARTESIAN_POINT ( 'NONE',  ( -0.07591351300297277671, 3.267716535433071279, 0.7874015748031456541 ) ) ;
#17120 = CARTESIAN_POINT ( 'NONE',  ( -3.001271764839907430, 2.755905511811027164, 0.08552506819282471029 ) ) ;
#17121 = ORIENTED_EDGE ( 'NONE', *, *, #33628, .F. ) ;
#17122 = VERTEX_POINT ( 'NONE', #43718 ) ;
#17123 = CARTESIAN_POINT ( 'NONE',  ( 0.000000000000000000, 3.267716535433071279, 0.4330708661417287386 ) ) ;
#17124 = ORIENTED_EDGE ( 'NONE', *, *, #38933, .T. ) ;
#17125 = CARTESIAN_POINT ( 'NONE',  ( -1.712496953225537633, 0.000000000000000000, -0.4724409448818884805 ) ) ;
#17126 = CARTESIAN_POINT ( 'NONE',  ( -2.475498251075796130, 1.050049506817961831, -0.6154945137624749929 ) ) ;
#17127 = EDGE_CURVE ( 'NONE', #24669, #47091, #16637, .T. ) ;
#17128 = AXIS2_PLACEMENT_3D ( 'NONE', #17910, #34173, #41404 ) ;
#17129 = AXIS2_PLACEMENT_3D ( 'NONE', #47696, #12369, #4122 ) ;
#17130 = LINE ( 'NONE', #33140, #20897 ) ;
#17131 = LINE ( 'NONE', #45479, #50743 ) ;
#17132 = DIRECTION ( 'NONE',  ( 0.9998717552508121775, 0.01601477604151182663, 0.000000000000000000 ) ) ;
#17133 = ORIENTED_EDGE ( 'NONE', *, *, #3540, .F. ) ;
#17134 = DIRECTION ( 'NONE',  ( 0.9510565162951500895, 0.000000000000000000, 0.3090169943749582204 ) ) ;
#17135 = ADVANCED_FACE ( 'NONE', ( #24116 ), #39957, .T. ) ;
#17136 = VECTOR ( 'NONE', #5418, 39.37007874015748143 ) ;
#17137 = CARTESIAN_POINT ( 'NONE',  ( 0.7423782071083085965, 3.267716535433071279, 0.1181102362204701633 ) ) ;
#17138 = ORIENTED_EDGE ( 'NONE', *, *, #41933, .T. ) ;
#17139 = DIRECTION ( 'NONE',  ( 1.000000000000000000, 0.000000000000000000, 0.000000000000000000 ) ) ;
#17140 = FACE_OUTER_BOUND ( 'NONE', #36616, .T. ) ;
#17141 = CARTESIAN_POINT ( 'NONE',  ( -1.439733046521776583, 3.346456692913386100, -0.3149606299212592275 ) ) ;
#17142 = ORIENTED_EDGE ( 'NONE', *, *, #33913, .T. ) ;
#17143 = CARTESIAN_POINT ( 'NONE',  ( -0.3381173457103602287, 1.574803149606302854, 2.138793126519845877 ) ) ;
#17144 = VECTOR ( 'NONE', #35082, 39.37007874015748143 ) ;
#17145 = DIRECTION ( 'NONE',  ( -0.000000000000000000, 1.000000000000000000, -0.000000000000000000 ) ) ;
#17146 = ORIENTED_EDGE ( 'NONE', *, *, #32092, .T. ) ;
#17147 = CARTESIAN_POINT ( 'NONE',  ( -1.052895522975213050, 1.537105172708097767, 2.758704046758604811 ) ) ;
#17148 = CARTESIAN_POINT ( 'NONE',  ( 2.191624600584984872, 1.710196431015120977, 0.7638471876793682114 ) ) ;
#17149 = EDGE_LOOP ( 'NONE', ( #28333, #9496, #7490, #12685 ) ) ;
#17150 = VECTOR ( 'NONE', #932, 39.37007874015748143 ) ;
#17151 = DIRECTION ( 'NONE',  ( 1.734723475976806848E-16, 0.000000000000000000, 1.000000000000000000 ) ) ;
#17152 = EDGE_CURVE ( 'NONE', #17158, #46657, #18886, .T. ) ;
#17153 = DIRECTION ( 'NONE',  ( -0.000000000000000000, 1.000000000000000000, -0.000000000000000000 ) ) ;
#17154 = CARTESIAN_POINT ( 'NONE',  ( 0.000000000000000000, 2.755905511811023612, 0.000000000000000000 ) ) ;
#17155 = LINE ( 'NONE', #12772, #25993 ) ;
#17156 = DIRECTION ( 'NONE',  ( 0.000000000000000000, 0.000000000000000000, 1.000000000000000000 ) ) ;
#17157 = ORIENTED_EDGE ( 'NONE', *, *, #26709, .F. ) ;
#17158 = VERTEX_POINT ( 'NONE', #50321 ) ;
#17159 = LINE ( 'NONE', #13032, #22409 ) ;
#17160 = CARTESIAN_POINT ( 'NONE',  ( 0.1968503937007877458, 3.267716535433071279, -6.829619984160669139E-17 ) ) ;
#17161 = ORIENTED_EDGE ( 'NONE', *, *, #5348, .T. ) ;
#17162 = CARTESIAN_POINT ( 'NONE',  ( 2.947574761915768171, 1.765190094501404072, -0.1816379373804911379 ) ) ;
#17163 = CARTESIAN_POINT ( 'NONE',  ( 1.091055626815042645, 0.000000000000000000, 0.7480314960629872445 ) ) ;
#17164 = DIRECTION ( 'NONE',  ( 1.000000000000000000, 0.000000000000000000, 0.000000000000000000 ) ) ;
#17165 = CARTESIAN_POINT ( 'NONE',  ( -1.225600105435525000, 0.000000000000000000, -1.239880218767125175 ) ) ;
#17166 = ORIENTED_EDGE ( 'NONE', *, *, #14765, .F. ) ;
#17167 = ORIENTED_EDGE ( 'NONE', *, *, #30158, .T. ) ;
#17168 = DIRECTION ( 'NONE',  ( -0.000000000000000000, 1.000000000000000000, -0.000000000000000000 ) ) ;
#17169 = DIRECTION ( 'NONE',  ( -1.000000000000000000, 0.000000000000000000, -0.000000000000000000 ) ) ;
#17170 = CIRCLE ( 'NONE', #28722, 2.165354330708661568 ) ;
#17171 = VECTOR ( 'NONE', #43594, 39.37007874015748143 ) ;
#17172 = DIRECTION ( 'NONE',  ( 1.734723475976806848E-16, -0.000000000000000000, 1.000000000000000000 ) ) ;
#17173 = ORIENTED_EDGE ( 'NONE', *, *, #22064, .T. ) ;
#17174 = CARTESIAN_POINT ( 'NONE',  ( 0.2727639067037604947, 3.346456692913386100, -0.1574803149606298636 ) ) ;
#17175 = FACE_BOUND ( 'NONE', #11851, .T. ) ;
#17176 = VERTEX_POINT ( 'NONE', #11391 ) ;
#17177 = DIRECTION ( 'NONE',  ( -3.469446951953613696E-16, 0.000000000000000000, -1.000000000000000000 ) ) ;
#17178 = ORIENTED_EDGE ( 'NONE', *, *, #28615, .T. ) ;
#17180 = ORIENTED_EDGE ( 'NONE', *, *, #1514, .T. ) ;
#17179 = VECTOR ( 'NONE', #46536, 39.37007874015748143 ) ;
#17181 = FACE_OUTER_BOUND ( 'NONE', #43683, .T. ) ;
#17182 = ADVANCED_FACE ( 'NONE', ( #3642 ), #19374, .T. ) ;
#17183 = AXIS2_PLACEMENT_3D ( 'NONE', #24055, #15790, #300 ) ;
#17184 = EDGE_CURVE ( 'NONE', #33705, #45841, #35023, .T. ) ;
#17185 = ORIENTED_EDGE ( 'NONE', *, *, #37160, .F. ) ;
#17186 = FACE_OUTER_BOUND ( 'NONE', #13368, .T. ) ;
#17187 = ADVANCED_FACE ( 'NONE', ( #23254 ), #10290, .T. ) ;
#17188 = VECTOR ( 'NONE', #22640, 39.37007874015748143 ) ;
#17189 = VERTEX_POINT ( 'NONE', #35393 ) ;
#17191 = CARTESIAN_POINT ( 'NONE',  ( -1.790754330931495275, 1.646411344893201845, -1.241033964651257149 ) ) ;
#17190 = CIRCLE ( 'NONE', #18806, 2.244934639244525076 ) ;
#17192 = LINE ( 'NONE', #29825, #29405 ) ;
#17193 = DIRECTION ( 'NONE',  ( -0.000000000000000000, 1.000000000000000000, -0.000000000000000000 ) ) ;
#17194 = ADVANCED_FACE ( 'NONE', ( #35140 ), #31010, .T. ) ;
#17195 = LINE ( 'NONE', #32960, #23946 ) ;
#17196 = CARTESIAN_POINT ( 'NONE',  ( -1.363819533518803029, 0.000000000000000000, 0.5905511811023582691 ) ) ;
#17197 = DIRECTION ( 'NONE',  ( 1.734723475976806848E-16, -0.000000000000000000, 1.000000000000000000 ) ) ;
#17198 = VERTEX_POINT ( 'NONE', #50820 ) ;
#17199 = PLANE ( 'NONE',  #29115 ) ;
#17200 = DIRECTION ( 'NONE',  ( 1.734723475976806848E-16, -0.000000000000000000, 1.000000000000000000 ) ) ;
#17201 = VERTEX_POINT ( 'NONE', #46223 ) ;
#17202 = CARTESIAN_POINT ( 'NONE',  ( -1.909347346926324462, 3.346456692913386100, -0.03937007874015881204 ) ) ;
#17203 = DIRECTION ( 'NONE',  ( -3.469446951953613696E-16, 0.000000000000000000, -1.000000000000000000 ) ) ;
#17204 = ORIENTED_EDGE ( 'NONE', *, *, #40791, .T. ) ;
#17205 = FACE_OUTER_BOUND ( 'NONE', #43324, .T. ) ;
#17206 = VECTOR ( 'NONE', #29081, 39.37007874015748143 ) ;
#17207 = EDGE_CURVE ( 'NONE', #47496, #45614, #3138, .T. ) ;
#17208 = CARTESIAN_POINT ( 'NONE',  ( 2.319222573356612749, 1.745048544795088308, -0.1534186080535354380 ) ) ;
#17209 = CARTESIAN_POINT ( 'NONE',  ( -1.439733046521776583, 3.267716535433071279, -0.6299212598425177889 ) ) ;
#17210 = VERTEX_POINT ( 'NONE', #11890 ) ;
#17211 = VECTOR ( 'NONE', #48306, 39.37007874015748143 ) ;
#17212 = PLANE ( 'NONE',  #46081 ) ;
#17213 = ORIENTED_EDGE ( 'NONE', *, *, #32145, .T. ) ;
#17214 = FACE_BOUND ( 'NONE', #33809, .T. ) ;
#17215 = EDGE_CURVE ( 'NONE', #29095, #42180, #23505, .T. ) ;
#17216 = DIRECTION ( 'NONE',  ( -0.000000000000000000, 0.000000000000000000, 1.000000000000000000 ) ) ;
#17217 = VECTOR ( 'NONE', #36028, 39.37007874015748143 ) ;
#17218 = VECTOR ( 'NONE', #1402, 39.37007874015748854 ) ;
#17219 = PLANE ( 'NONE',  #19361 ) ;
#17220 = CARTESIAN_POINT ( 'NONE',  ( -1.439733046521776139, 3.267716535433071279, 1.259842519685033357 ) ) ;
#17221 = B_SPLINE_CURVE_WITH_KNOTS ( 'NONE', 3,
 ( #50794, #35370, #31491, #239 ),
 .UNSPECIFIED., .F., .F.,
 ( 4, 4 ),
 ( 0.001744585901858061424, 0.04556827975943426173 ),
 .UNSPECIFIED. ) ;
#17222 = VECTOR ( 'NONE', #45162, 39.37007874015748143 ) ;
#17223 = EDGE_LOOP ( 'NONE', ( #47337, #47055, #18987, #33982 ) ) ;
#17224 = VERTEX_POINT ( 'NONE', #11639 ) ;
#17225 = DIRECTION ( 'NONE',  ( -3.469446951953613696E-16, 0.000000000000000000, -1.000000000000000000 ) ) ;
#17226 = ORIENTED_EDGE ( 'NONE', *, *, #49108, .F. ) ;
#17227 = EDGE_CURVE ( 'NONE', #3253, #3427, #46719, .T. ) ;
#17228 = AXIS2_PLACEMENT_3D ( 'NONE', #14400, #33535, #37402 ) ;
#17229 = DIRECTION ( 'NONE',  ( -0.000000000000000000, 1.000000000000000000, -0.000000000000000000 ) ) ;
#17230 = ORIENTED_EDGE ( 'NONE', *, *, #34511, .T. ) ;
#17231 = ADVANCED_FACE ( 'NONE', ( #19128 ), #27125, .T. ) ;
#17232 = LINE ( 'NONE', #48669, #11600 ) ;
#17233 = VERTEX_POINT ( 'NONE', #31270 ) ;
#17234 = LINE ( 'NONE', #12586, #19984 ) ;
#17235 = CARTESIAN_POINT ( 'NONE',  ( -2.454875160333845674, 3.346456692913386100, -0.1574803149606298636 ) ) ;
#17236 = ORIENTED_EDGE ( 'NONE', *, *, #9074, .T. ) ;
#17237 = DIRECTION ( 'NONE',  ( 0.000000000000000000, -1.000000000000000000, 0.000000000000000000 ) ) ;
#17238 = ORIENTED_EDGE ( 'NONE', *, *, #20358, .T. ) ;
#17239 = VERTEX_POINT ( 'NONE', #11139 ) ;
#17240 = EDGE_CURVE ( 'NONE', #50120, #22538, #13, .T. ) ;
#17241 = VECTOR ( 'NONE', #36719, 39.37007874015748143 ) ;
#17242 = ORIENTED_EDGE ( 'NONE', *, *, #44663, .F. ) ;
#17243 = VERTEX_POINT ( 'NONE', #43373 ) ;
#17244 = EDGE_CURVE ( 'NONE', #38459, #24866, #42369, .T. ) ;
#17245 = LINE ( 'NONE', #33004, #34351 ) ;
#17246 = EDGE_CURVE ( 'NONE', #29348, #11414, #28405, .T. ) ;
#17247 = DIRECTION ( 'NONE',  ( -4.561975526775755056E-17, -1.000000000000000000, 1.067327232801816862E-16 ) ) ;
#17248 = ORIENTED_EDGE ( 'NONE', *, *, #20561, .F. ) ;
#17249 = DIRECTION ( 'NONE',  ( 1.734723475976806848E-16, -0.000000000000000000, 1.000000000000000000 ) ) ;
#17250 = VERTEX_POINT ( 'NONE', #31521 ) ;
#17251 = LINE ( 'NONE', #29879, #18647 ) ;
#17252 = AXIS2_PLACEMENT_3D ( 'NONE', #26115, #25604, #2374 ) ;
#17253 = VECTOR ( 'NONE', #47800, 39.37007874015748143 ) ;
#17254 = DIRECTION ( 'NONE',  ( 0.000000000000000000, 0.000000000000000000, -1.000000000000000000 ) ) ;
#17255 = AXIS2_PLACEMENT_3D ( 'NONE', #10155, #6291, #48340 ) ;
#17256 = ORIENTED_EDGE ( 'NONE', *, *, #44616, .F. ) ;
#17257 = LINE ( 'NONE', #18260, #37674 ) ;
#17258 = CARTESIAN_POINT ( 'NONE',  ( 0.000000000000000000, 6.692913385826772199, -2.086614173228346303 ) ) ;
#17259 = ORIENTED_EDGE ( 'NONE', *, *, #17019, .F. ) ;
#17260 = CARTESIAN_POINT ( 'NONE',  ( -2.454875160333845674, 3.346456692913386100, -0.1574803149606298636 ) ) ;
#17261 = DIRECTION ( 'NONE',  ( 0.000000000000000000, 0.000000000000000000, -1.000000000000000000 ) ) ;
#17262 = VECTOR ( 'NONE', #362, 39.37007874015748143 ) ;
#17263 = CARTESIAN_POINT ( 'NONE',  ( 1.091055626815042645, 0.000000000000000000, -0.6299212598425181220 ) ) ;
#17264 = LINE ( 'NONE', #41511, #6666 ) ;
#17265 = DIRECTION ( 'NONE',  ( 0.000000000000000000, 0.000000000000000000, -1.000000000000000000 ) ) ;
#17266 = VERTEX_POINT ( 'NONE', #47214 ) ;
#17267 = LINE ( 'NONE', #25259, #26249 ) ;
#17268 = EDGE_CURVE ( 'NONE', #23466, #20757, #26867, .T. ) ;
#17269 = DIRECTION ( 'NONE',  ( 0.000000000000000000, 0.000000000000000000, -1.000000000000000000 ) ) ;
#17270 = ORIENTED_EDGE ( 'NONE', *, *, #13049, .T. ) ;
#17271 = LINE ( 'NONE', #9519, #47316 ) ;
#17272 = VERTEX_POINT ( 'NONE', #7271 ) ;
#17273 = CARTESIAN_POINT ( 'NONE',  ( 1.287906020515829919, 0.000000000000000000, -1.456692913385822630 ) ) ;
#17274 = EDGE_CURVE ( 'NONE', #39828, #42444, #15258, .T. ) ;
#17275 = CARTESIAN_POINT ( 'NONE',  ( -1.636583440222563635, 0.000000000000000000, 0.3149606299212578953 ) ) ;
#17276 = CARTESIAN_POINT ( 'NONE',  ( -0.8942052331142552601, 3.267716535433071279, 1.692913385826762873 ) ) ;
#17277 = EDGE_CURVE ( 'NONE', #1528, #24292, #40545, .T. ) ;
#17278 = CARTESIAN_POINT ( 'NONE',  ( 0.5455278134075212115, 3.346456692913386100, 0.9448818897637746295 ) ) ;
#17279 = CARTESIAN_POINT ( 'NONE',  ( -2.165354330708661568, 1.574803149606301966, -1.520079223026944511E-17 ) ) ;
#17280 = VECTOR ( 'NONE', #19352, 39.37007874015748143 ) ;
#17281 = ORIENTED_EDGE ( 'NONE', *, *, #48081, .T. ) ;
#17282 = EDGE_CURVE ( 'NONE', #25584, #20592, #4661, .T. ) ;
#17283 = CARTESIAN_POINT ( 'NONE',  ( 0.9989521216866641407, 0.000000000000000000, 1.767914056614194651 ) ) ;
#17284 = DIRECTION ( 'NONE',  ( -0.000000000000000000, 1.000000000000000000, -0.000000000000000000 ) ) ;
#17285 = ORIENTED_EDGE ( 'NONE', *, *, #45541, .F. ) ;
#17286 = CARTESIAN_POINT ( 'NONE',  ( -1.593548266680976155, 0.001619815658173129856, -0.7346346424156023902 ) ) ;
#17287 = EDGE_LOOP ( 'NONE', ( #49560, #9461, #37404 ) ) ;
#17288 = CIRCLE ( 'NONE', #2474, 2.106299212598425008 ) ;
#17289 = CARTESIAN_POINT ( 'NONE',  ( -2.491402175429631605, 1.205361022782829114E-17, -1.585592796919542025 ) ) ;
#17290 = CARTESIAN_POINT ( 'NONE',  ( 1.363819533518803695, 0.000000000000000000, 1.732283464566921172 ) ) ;
#17291 = CARTESIAN_POINT ( 'NONE',  ( 2.147141360900377105, 6.692913385826772199, 0.3405121111982932769 ) ) ;
#17292 = DIRECTION ( 'NONE',  ( 1.000000000000000000, 0.000000000000000000, 0.000000000000000000 ) ) ;
#17293 = EDGE_LOOP ( 'NONE', ( #42365, #26648, #5573, #424 ) ) ;
#17294 = VERTEX_POINT ( 'NONE', #20139 ) ;
#17295 = CARTESIAN_POINT ( 'NONE',  ( 1.146850602739119651, 0.5249316497054294928, -1.494778961828568065 ) ) ;
#17296 = CARTESIAN_POINT ( 'NONE',  ( -0.2727639067037604392, 3.267716535433071279, 4.731699523581607276E-17 ) ) ;
#17297 = FACE_BOUND ( 'NONE', #27346, .T. ) ;
#17298 = AXIS2_PLACEMENT_3D ( 'NONE', #28243, #19734, #22923 ) ;
#17299 = EDGE_CURVE ( 'NONE', #34229, #29725, #28140, .T. ) ;
#17300 = FACE_OUTER_BOUND ( 'NONE', #50741, .T. ) ;
#17301 = LINE ( 'NONE', #24786, #39013 ) ;
#17302 = ORIENTED_EDGE ( 'NONE', *, *, #837, .T. ) ;
#17303 = EDGE_CURVE ( 'NONE', #10313, #25755, #44106, .T. ) ;
#17304 = EDGE_CURVE ( 'NONE', #11282, #39747, #1040, .T. ) ;
#17305 = DIRECTION ( 'NONE',  ( -3.469446951953613696E-16, 0.000000000000000000, -1.000000000000000000 ) ) ;
#17306 = EDGE_CURVE ( 'NONE', #47803, #16032, #12401, .T. ) ;
#17307 = LINE ( 'NONE', #13429, #39397 ) ;
#17308 = ORIENTED_EDGE ( 'NONE', *, *, #10169, .F. ) ;
#17309 = ORIENTED_EDGE ( 'NONE', *, *, #50032, .F. ) ;
#17310 = ORIENTED_EDGE ( 'NONE', *, *, #36215, .F. ) ;
#17311 = FACE_OUTER_BOUND ( 'NONE', #13232, .T. ) ;
#17312 = CARTESIAN_POINT ( 'NONE',  ( 0.7381027496705272473, 1.730766751998747521, -2.859439394060913298 ) ) ;
#17313 = VECTOR ( 'NONE', #4784, 39.37007874015748143 ) ;
#17314 = B_SPLINE_CURVE_WITH_KNOTS ( 'NONE', 3,
 ( #47761, #39547, #4179, #47506 ),
 .UNSPECIFIED., .F., .F.,
 ( 4, 4 ),
 ( 0.001814792330965703596, 0.004762084017055013413 ),
 .UNSPECIFIED. ) ;
#17315 = LINE ( 'NONE', #1042, #18466 ) ;
#17316 = FACE_OUTER_BOUND ( 'NONE', #29016, .T. ) ;
#17317 = EDGE_LOOP ( 'NONE', ( #17104, #12759, #27962, #34920, #3827, #19007 ) ) ;
#17318 = ORIENTED_EDGE ( 'NONE', *, *, #3418, .T. ) ;
#17319 = DIRECTION ( 'NONE',  ( 1.734723475976806848E-16, 0.000000000000000000, 1.000000000000000000 ) ) ;
#17320 = SURFACE_STYLE_FILL_AREA ( #32303 ) ;
#17321 = DIRECTION ( 'NONE',  ( 0.000000000000000000, 1.000000000000000000, 0.000000000000000000 ) ) ;
#17322 = PLANE ( 'NONE',  #3717 ) ;
#17323 = DIRECTION ( 'NONE',  ( 1.734723475976806848E-16, 0.000000000000000000, 1.000000000000000000 ) ) ;
#17324 = VECTOR ( 'NONE', #19320, 39.37007874015748143 ) ;
#17325 = VECTOR ( 'NONE', #33952, 39.37007874015748143 ) ;
#17326 = DIRECTION ( 'NONE',  ( -0.01601477604151182663, 0.9998717552508123996, -0.000000000000000000 ) ) ;
#17327 = FACE_OUTER_BOUND ( 'NONE', #13874, .T. ) ;
#17328 = VERTEX_POINT ( 'NONE', #16279 ) ;
#17329 = CARTESIAN_POINT ( 'NONE',  ( -1.166969139818015533, 3.267716535433071279, 0.7874015748031456541 ) ) ;
#17330 = LINE ( 'NONE', #33090, #41749 ) ;
#17331 = VECTOR ( 'NONE', #32593, 39.37007874015748143 ) ;
#17332 = B_SPLINE_CURVE_WITH_KNOTS ( 'NONE', 3,
 ( #2079, #14200, #5946, #41829 ),
 .UNSPECIFIED., .F., .F.,
 ( 4, 4 ),
 ( 0.0004124273248910236846, 0.004895227329085388539 ),
 .UNSPECIFIED. ) ;
#17333 = ORIENTED_EDGE ( 'NONE', *, *, #6892, .T. ) ;
#17334 = EDGE_LOOP ( 'NONE', ( #41031, #9965, #10794, #27529 ) ) ;
#17335 = LINE ( 'NONE', #48011, #29862 ) ;
#17336 = DIRECTION ( 'NONE',  ( -3.469446951953613696E-16, 0.000000000000000000, -1.000000000000000000 ) ) ;
#17337 = EDGE_CURVE ( 'NONE', #30710, #24910, #28993, .T. ) ;
#17338 = VERTEX_POINT ( 'NONE', #20920 ) ;
#17339 = EDGE_CURVE ( 'NONE', #40993, #26527, #13615, .T. ) ;
#17340 = ORIENTED_EDGE ( 'NONE', *, *, #25389, .F. ) ;
#17341 = CARTESIAN_POINT ( 'NONE',  ( 1.872964171113514320, 0.5249316475426858419, 0.2040481836961198225 ) ) ;
#17342 = VERTEX_POINT ( 'NONE', #9045 ) ;
#17343 = DIRECTION ( 'NONE',  ( 1.000000000000000000, 0.000000000000000000, 0.000000000000000000 ) ) ;
#17344 = CARTESIAN_POINT ( 'NONE',  ( -0.2727639067037607723, 0.000000000000000000, -0.1574803149606301411 ) ) ;
#17345 = ORIENTED_EDGE ( 'NONE', *, *, #8749, .T. ) ;
#17346 = ORIENTED_EDGE ( 'NONE', *, *, #42275, .F. ) ;
#17347 = EDGE_LOOP ( 'NONE', ( #16419, #2076, #33497, #38526 ) ) ;
#17348 = DIRECTION ( 'NONE',  ( -0.000000000000000000, 1.000000000000000000, -0.000000000000000000 ) ) ;
#17349 = ORIENTED_EDGE ( 'NONE', *, *, #37730, .T. ) ;
#17350 = VERTEX_POINT ( 'NONE', #31779 ) ;
#17351 = FACE_OUTER_BOUND ( 'NONE', #11865, .T. ) ;
#17352 = CARTESIAN_POINT ( 'NONE',  ( 1.902660579019252562, 1.639951345248664039, -1.314902632263422966 ) ) ;
#17353 = DIRECTION ( 'NONE',  ( 0.9195277725514544587, 0.000000000000000000, -0.3930250316539147803 ) ) ;
#17354 = EDGE_CURVE ( 'NONE', #42335, #25112, #43216, .T. ) ;
#17355 = VECTOR ( 'NONE', #9447, 39.37007874015748143 ) ;
#17356 = ORIENTED_EDGE ( 'NONE', *, *, #16892, .F. ) ;
#17357 = EDGE_CURVE ( 'NONE', #20926, #20810, #787, .T. ) ;
#17358 = AXIS2_PLACEMENT_3D ( 'NONE', #6586, #45531, #50145 ) ;
#17359 = FACE_OUTER_BOUND ( 'NONE', #9290, .T. ) ;
#17360 = DIRECTION ( 'NONE',  ( 1.734723475976806848E-16, -0.000000000000000000, 1.000000000000000000 ) ) ;
#17361 = DIRECTION ( 'NONE',  ( -3.469446951953613696E-16, 0.000000000000000000, -1.000000000000000000 ) ) ;
#17362 = VERTEX_POINT ( 'NONE', #24284 ) ;
#17363 = EDGE_CURVE ( 'NONE', #45537, #12259, #9302, .T. ) ;
#17364 = FACE_OUTER_BOUND ( 'NONE', #20713, .T. ) ;
#17365 = DIRECTION ( 'NONE',  ( -3.469446951953613696E-16, 0.000000000000000000, -1.000000000000000000 ) ) ;
#17366 = EDGE_CURVE ( 'NONE', #3716, #49734, #43629, .T. ) ;
#17367 = CARTESIAN_POINT ( 'NONE',  ( 0.000000000000000000, 3.267716535433071279, -0.1968503937007879123 ) ) ;
#17368 = ORIENTED_EDGE ( 'NONE', *, *, #22933, .F. ) ;
#17369 = ORIENTED_EDGE ( 'NONE', *, *, #34875, .F. ) ;
#17370 = LINE ( 'NONE', #44967, #28031 ) ;
#17371 = DIRECTION ( 'NONE',  ( 0.000000000000000000, -1.000000000000000000, 0.000000000000000000 ) ) ;
#17372 = CARTESIAN_POINT ( 'NONE',  ( -2.437180031585919782, 1.681273446161504426, -1.667735833703134718 ) ) ;
#17373 = VERTEX_POINT ( 'NONE', #20402 ) ;
#17374 = ORIENTED_EDGE ( 'NONE', *, *, #44666, .T. ) ;
#17375 = CARTESIAN_POINT ( 'NONE',  ( -1.486187880958816931, 3.346456692913386100, 1.574803149606291530 ) ) ;
#17376 = EDGE_LOOP ( 'NONE', ( #27707, #25595, #42396, #40447 ) ) ;
#17377 = CARTESIAN_POINT ( 'NONE',  ( -2.339241080213612545, 0.000000000000000000, 1.802537235681884065 ) ) ;
#17378 = DIRECTION ( 'NONE',  ( -1.000000000000000000, -0.000000000000000000, -0.000000000000000000 ) ) ;
#17379 = DIRECTION ( 'NONE',  ( 1.734723475976806848E-16, 0.000000000000000000, 1.000000000000000000 ) ) ;
#17380 = CARTESIAN_POINT ( 'NONE',  ( -2.160501893660597084, 3.267716535433071279, -1.141732283464563791 ) ) ;
#17381 = FACE_OUTER_BOUND ( 'NONE', #31128, .T. ) ;
#17382 = ORIENTED_EDGE ( 'NONE', *, *, #3043, .F. ) ;
#17383 = DIRECTION ( 'NONE',  ( -0.01601477604151182663, 0.9998717552508123996, -0.000000000000000000 ) ) ;
#17384 = LINE ( 'NONE', #33409, #40565 ) ;
#17385 = VECTOR ( 'NONE', #26830, 39.37007874015748143 ) ;
#17386 = EDGE_LOOP ( 'NONE', ( #40906, #1433, #15767, #43734 ) ) ;
#17387 = CARTESIAN_POINT ( 'NONE',  ( -1.198202975868768005, 3.346456692913386100, 1.732283464566920950 ) ) ;
#17388 = VECTOR ( 'NONE', #49981, 39.37007874015748143 ) ;
#17389 = CARTESIAN_POINT ( 'NONE',  ( 0.04921259842519689481, 1.205361022782829114E-17, 2.952755905511811108 ) ) ;
#17390 = DIRECTION ( 'NONE',  ( -1.000000000000000000, 0.000000000000000000, -0.000000000000000000 ) ) ;
#17391 = ORIENTED_EDGE ( 'NONE', *, *, #51011, .F. ) ;
#17392 = DIRECTION ( 'NONE',  ( -3.469446951953613696E-16, 0.000000000000000000, -1.000000000000000000 ) ) ;
#17393 = CARTESIAN_POINT ( 'NONE',  ( -1.695772546416001392, 1.551146592414875958, -2.417756147381374010 ) ) ;
#17394 = EDGE_CURVE ( 'NONE', #35414, #23176, #11134, .T. ) ;
#17395 = EDGE_CURVE ( 'NONE', #34717, #22865, #16540, .T. ) ;
#17396 = ORIENTED_EDGE ( 'NONE', *, *, #8007, .F. ) ;
#17397 = PLANE ( 'NONE',  #12311 ) ;
#17398 = AXIS2_PLACEMENT_3D ( 'NONE', #46089, #42230, #1984 ) ;
#17399 = DIRECTION ( 'NONE',  ( 0.000000000000000000, 0.000000000000000000, -1.000000000000000000 ) ) ;
#17400 = VERTEX_POINT ( 'NONE', #1297 ) ;
#17401 = DIRECTION ( 'NONE',  ( 1.734723475976806848E-16, -0.000000000000000000, 1.000000000000000000 ) ) ;
#17402 = EDGE_CURVE ( 'NONE', #41605, #10030, #17060, .T. ) ;
#17403 = CARTESIAN_POINT ( 'NONE',  ( 0.000000000000000000, 3.267716535433071279, 0.000000000000000000 ) ) ;
#17404 = LINE ( 'NONE', #33167, #12314 ) ;
#17405 = CARTESIAN_POINT ( 'NONE',  ( -1.171042467547485311, 1.689145562575557369, 1.864045119995098698 ) ) ;
#17406 = CARTESIAN_POINT ( 'NONE',  ( -0.5455278134075214336, 3.346456692913386100, -2.034427629037601104 ) ) ;
#17407 = ORIENTED_EDGE ( 'NONE', *, *, #7130, .T. ) ;
#17408 = VERTEX_POINT ( 'NONE', #40292 ) ;
#17409 = CARTESIAN_POINT ( 'NONE',  ( 1.550261229843175492, 1.634307024739966696, 1.699618603577774945 ) ) ;
#17410 = CARTESIAN_POINT ( 'NONE',  ( 1.091055626815042645, 3.267716535433071279, -1.892679809432644882E-16 ) ) ;
#17411 = ORIENTED_EDGE ( 'NONE', *, *, #1563, .T. ) ;
#17412 = CARTESIAN_POINT ( 'NONE',  ( -1.091055626815042645, 0.000000000000000000, 1.889763779527550147 ) ) ;
#17413 = LINE ( 'NONE', #49619, #40099 ) ;
#17414 = DIRECTION ( 'NONE',  ( -0.9998717552508122886, -0.01601477604151181275, 0.000000000000000000 ) ) ;
#17415 = LINE ( 'NONE', #14750, #36379 ) ;
#17416 = VERTEX_POINT ( 'NONE', #32817 ) ;
#17417 = ORIENTED_EDGE ( 'NONE', *, *, #50678, .F. ) ;
#17418 = EDGE_CURVE ( 'NONE', #46251, #37360, #48501, .T. ) ;
#17419 = DIRECTION ( 'NONE',  ( 1.000000000000000000, 0.000000000000000000, -3.469446951953613696E-16 ) ) ;
#17420 = CARTESIAN_POINT ( 'NONE',  ( 2.576863348864710801, 0.000000000000000000, 1.442554885838449819 ) ) ;
#17421 = CARTESIAN_POINT ( 'NONE',  ( 4.268512490100411402E-16, 0.000000000000000000, 1.574803149606291974 ) ) ;
#17422 = ORIENTED_EDGE ( 'NONE', *, *, #12150, .T. ) ;
#17423 = CARTESIAN_POINT ( 'NONE',  ( 1.091055626815043311, 3.346456692913386100, 1.889763779527550369 ) ) ;
#17424 = FACE_BOUND ( 'NONE', #7589, .T. ) ;
#17425 = ORIENTED_EDGE ( 'NONE', *, *, #12667, .F. ) ;
#17426 = EDGE_CURVE ( 'NONE', #25538, #4899, #8275, .T. ) ;
#17427 = CARTESIAN_POINT ( 'NONE',  ( -2.168245791271168343, 1.560742704294596495, -2.004968704497279486 ) ) ;
#17428 = VERTEX_POINT ( 'NONE', #24020 ) ;
#17429 = ORIENTED_EDGE ( 'NONE', *, *, #27252, .F. ) ;
#17430 = CIRCLE ( 'NONE', #19863, 2.106299212598425008 ) ;
#17431 = DIRECTION ( 'NONE',  ( 0.000000000000000000, 1.000000000000000000, 0.000000000000000000 ) ) ;
#17432 = CIRCLE ( 'NONE', #5884, 0.8858267716535433989 ) ;
#17433 = AXIS2_PLACEMENT_3D ( 'NONE', #9991, #6375, #13869 ) ;
#17434 = VERTEX_POINT ( 'NONE', #39170 ) ;
#17435 = CARTESIAN_POINT ( 'NONE',  ( 1.015142113812069979, 3.267716535433071279, 1.912654141836395372 ) ) ;
#17436 = CARTESIAN_POINT ( 'NONE',  ( 1.287906020515830141, 0.000000000000000000, -0.3149606299212596716 ) ) ;
#17437 = ORIENTED_EDGE ( 'NONE', *, *, #18207, .T. ) ;
#17438 = AXIS2_PLACEMENT_3D ( 'NONE', #26857, #7256, #38749 ) ;
#17439 = DIRECTION ( 'NONE',  ( 1.000000000000000000, 0.000000000000000000, 0.000000000000000000 ) ) ;
#17440 = EDGE_CURVE ( 'NONE', #12193, #22497, #47387, .T. ) ;
#17441 = CARTESIAN_POINT ( 'NONE',  ( 1.909347346926324684, 0.000000000000000000, 0.5905511811023582691 ) ) ;
#17442 = PLANE ( 'NONE',  #26707 ) ;
#17443 = VECTOR ( 'NONE', #8432, 39.37007874015748143 ) ;
#17444 = CARTESIAN_POINT ( 'NONE',  ( 1.355960331127249452, 0.04963785175798203497, -1.364517356352728861 ) ) ;
#17445 = CARTESIAN_POINT ( 'NONE',  ( 2.755905511811024056, 4.960629921259846142, -1.023622047244094224 ) ) ;
#17446 = DIRECTION ( 'NONE',  ( -0.000000000000000000, 1.000000000000000000, -0.000000000000000000 ) ) ;
#17447 = VERTEX_POINT ( 'NONE', #15673 ) ;
#17448 = CARTESIAN_POINT ( 'NONE',  ( 0.000000000000000000, 0.000000000000000000, 0.000000000000000000 ) ) ;
#17449 = CARTESIAN_POINT ( 'NONE',  ( 1.025452293874513421, 0.4610579152940180725, 1.025452293874513199 ) ) ;
#17450 = EDGE_LOOP ( 'NONE', ( #41188, #47071, #39445, #18416 ) ) ;
#17451 = LINE ( 'NONE', #13588, #1772 ) ;
#17452 = DIRECTION ( 'NONE',  ( 0.000000000000000000, 0.000000000000000000, 1.000000000000000000 ) ) ;
#17453 = VERTEX_POINT ( 'NONE', #35051 ) ;
#17454 = CARTESIAN_POINT ( 'NONE',  ( -0.8182917201112819283, 0.000000000000000000, 1.850393700787391849 ) ) ;
#17455 = CARTESIAN_POINT ( 'NONE',  ( -0.6214413264104945434, 0.000000000000000000, -0.6692913385826760875 ) ) ;
#17456 = DIRECTION ( 'NONE',  ( -1.000000000000000000, 0.000000000000000000, 0.000000000000000000 ) ) ;
#17457 = EDGE_CURVE ( 'NONE', #3179, #7335, #3294, .T. ) ;
#17458 = ORIENTED_EDGE ( 'NONE', *, *, #49140, .F. ) ;
#17459 = PLANE ( 'NONE',  #32112 ) ;
#17460 = EDGE_LOOP ( 'NONE', ( #12684, #46220, #12594, #50697 ) ) ;
#17461 = FACE_BOUND ( 'NONE', #25950, .T. ) ;
#17462 = EDGE_CURVE ( 'NONE', #38330, #4093, #31428, .T. ) ;
#17463 = CARTESIAN_POINT ( 'NONE',  ( 1.163887619842433718, 0.04656145577143805392, -1.518228404148327160 ) ) ;
#17464 = AXIS2_PLACEMENT_3D ( 'NONE', #19964, #27461, #39346 ) ;
#17465 = VECTOR ( 'NONE', #27753, 39.37007874015748143 ) ;
#17466 = DIRECTION ( 'NONE',  ( 0.000000000000000000, 0.000000000000000000, -1.000000000000000000 ) ) ;
#17468 = EDGE_CURVE ( 'NONE', #21800, #24086, #440, .T. ) ;
#17467 = CARTESIAN_POINT ( 'NONE',  ( -1.091055626815042645, 3.346456692913386100, 1.889763779527550147 ) ) ;
#17469 = EDGE_CURVE ( 'NONE', #50140, #35927, #39684, .T. ) ;
#17470 = VECTOR ( 'NONE', #32404, 39.37007874015748143 ) ;
#17471 = ORIENTED_EDGE ( 'NONE', *, *, #38672, .F. ) ;
#17472 = ORIENTED_EDGE ( 'NONE', *, *, #48467, .F. ) ;
#17473 = LINE ( 'NONE', #13604, #42758 ) ;
#17474 = EDGE_LOOP ( 'NONE', ( #20238, #48538, #11711, #5563 ) ) ;
#17475 = VECTOR ( 'NONE', #22186, 39.37007874015748143 ) ;
#17476 = CARTESIAN_POINT ( 'NONE',  ( 0.3664524127070866721, -0.6299212598425202314, 0.07483588040983164824 ) ) ;
#17477 = ORIENTED_EDGE ( 'NONE', *, *, #556, .F. ) ;
#17478 = CARTESIAN_POINT ( 'NONE',  ( -1.712496953225537633, 3.346456692913386100, -1.102362204724405492 ) ) ;
#17479 = VECTOR ( 'NONE', #22346, 39.37007874015748143 ) ;
#17480 = EDGE_CURVE ( 'NONE', #9409, #35448, #47128, .T. ) ;
#17481 = ORIENTED_EDGE ( 'NONE', *, *, #29987, .T. ) ;
#17482 = CARTESIAN_POINT ( 'NONE',  ( -0.2727639067037602172, 3.346456692913386100, 1.732283464566921172 ) ) ;
#17483 = CARTESIAN_POINT ( 'NONE',  ( 0.8182917201112819283, 3.346456692913386100, 0.1574803149606286423 ) ) ;
#17484 = ORIENTED_EDGE ( 'NONE', *, *, #19814, .F. ) ;
#17485 = ADVANCED_FACE ( 'NONE', ( #31178 ), #11798, .F. ) ;
#17486 = CARTESIAN_POINT ( 'NONE',  ( -2.417802884545332542, 3.267716535433071279, -0.3543307086614173040 ) ) ;
#17487 = ORIENTED_EDGE ( 'NONE', *, *, #5455, .T. ) ;
#17488 = VERTEX_POINT ( 'NONE', #23673 ) ;
#17489 = EDGE_CURVE ( 'NONE', #25903, #14916, #38676, .T. ) ;
#17490 = ORIENTED_EDGE ( 'NONE', *, *, #32110, .F. ) ;
#17491 = ORIENTED_EDGE ( 'NONE', *, *, #13715, .T. ) ;
#17492 = DIRECTION ( 'NONE',  ( -0.01601477604151182663, 0.9998717552508123996, -0.000000000000000000 ) ) ;
#17493 = VERTEX_POINT ( 'NONE', #23165 ) ;
#17494 = DIRECTION ( 'NONE',  ( -0.000000000000000000, 1.000000000000000000, -0.000000000000000000 ) ) ;
#17495 = EDGE_CURVE ( 'NONE', #27834, #3496, #2077, .T. ) ;
#17496 = ORIENTED_EDGE ( 'NONE', *, *, #42141, .F. ) ;
#17497 = CARTESIAN_POINT ( 'NONE',  ( 0.9442395380435398833, 1.624600478255878055, -2.074157072296122450 ) ) ;
#17498 = CIRCLE ( 'NONE', #25719, 2.165354330708661568 ) ;
#17499 = DIRECTION ( 'NONE',  ( -3.469446951953613696E-16, 0.000000000000000000, -1.000000000000000000 ) ) ;
#17500 = ORIENTED_EDGE ( 'NONE', *, *, #5447, .T. ) ;
#17501 = VECTOR ( 'NONE', #37170, 39.37007874015748143 ) ;
#17502 = DIRECTION ( 'NONE',  ( -1.000000000000000000, -0.000000000000000000, -0.000000000000000000 ) ) ;
#17503 = CARTESIAN_POINT ( 'NONE',  ( 0.1155636338427008941, -0.5222242541845523167, 0.000000000000000000 ) ) ;
#17504 = EDGE_LOOP ( 'NONE', ( #19936, #22605, #48001, #48939 ) ) ;
#17505 = CARTESIAN_POINT ( 'NONE',  ( 1.363819533518803695, 3.346456692913386100, 1.535433070866133898 ) ) ;
#17506 = CARTESIAN_POINT ( 'NONE',  ( 1.377485945418314151, 1.001684976433488528, 2.209573301320594485 ) ) ;
#17507 = EDGE_CURVE ( 'NONE', #13815, #29456, #38921, .T. ) ;
#17508 = CIRCLE ( 'NONE', #38125, 2.106299212598425008 ) ;
#17509 = LINE ( 'NONE', #28865, #4564 ) ;
#17510 = EDGE_CURVE ( 'NONE', #48815, #26618, #7929, .T. ) ;
#17511 = DIRECTION ( 'NONE',  ( 0.000000000000000000, 0.000000000000000000, -1.000000000000000000 ) ) ;
#17512 = VECTOR ( 'NONE', #44308, 39.37007874015748143 ) ;
#17513 = DIRECTION ( 'NONE',  ( 0.7818314824680311359, 0.000000000000000000, -0.6234898018587319291 ) ) ;
#17514 = ORIENTED_EDGE ( 'NONE', *, *, #35535, .F. ) ;
#17515 = LINE ( 'NONE', #33275, #13875 ) ;
#17516 = DIRECTION ( 'NONE',  ( 1.154631945610162802E-14, 0.000000000000000000, 1.000000000000000000 ) ) ;
#17517 = ORIENTED_EDGE ( 'NONE', *, *, #36072, .F. ) ;
#17518 = LINE ( 'NONE', #40254, #34984 ) ;
#17519 = ORIENTED_EDGE ( 'NONE', *, *, #35514, .T. ) ;
#17520 = LINE ( 'NONE', #48713, #40472 ) ;
#17521 = ADVANCED_FACE ( 'NONE', ( #27541 ), #19284, .F. ) ;
#17522 = DIRECTION ( 'NONE',  ( -1.000000000000000000, 0.000000000000000000, 1.734723475976806848E-16 ) ) ;
#17523 = DIRECTION ( 'NONE',  ( -1.000000000000000000, 0.000000000000000000, 0.000000000000000000 ) ) ;
#17524 = DIRECTION ( 'NONE',  ( -0.8584487936018655452, -1.160734090543304660E-16, -0.5128992774059071280 ) ) ;
#17525 = CARTESIAN_POINT ( 'NONE',  ( 1.091055626815042867, 3.267716535433071279, -1.892679809432645129E-16 ) ) ;
#17526 = EDGE_LOOP ( 'NONE', ( #19136, #46454, #40187, #13816 ) ) ;
#17527 = ADVANCED_FACE ( 'NONE', ( #35306 ), #16194, .F. ) ;
#17528 = DIRECTION ( 'NONE',  ( -0.000000000000000000, 1.000000000000000000, -0.000000000000000000 ) ) ;
#17529 = CARTESIAN_POINT ( 'NONE',  ( 0.7111759851608010496, 1.722959852249558388, -2.391904164000848709 ) ) ;
#17530 = CARTESIAN_POINT ( 'NONE',  ( 0.000000000000000000, 2.755905511811024056, 0.000000000000000000 ) ) ;
#17531 = VERTEX_POINT ( 'NONE', #23935 ) ;
#17532 = LINE ( 'NONE', #12899, #41943 ) ;
#17533 = VERTEX_POINT ( 'NONE', #4313 ) ;
#17534 = CARTESIAN_POINT ( 'NONE',  ( 0.000000000000000000, 3.346456692913386100, 0.000000000000000000 ) ) ;
#17535 = CARTESIAN_POINT ( 'NONE',  ( -0.8182917201112819283, 0.000000000000000000, -0.4724409448818886470 ) ) ;
#17536 = CIRCLE ( 'NONE', #32359, 2.165354330708661568 ) ;
#17537 = CARTESIAN_POINT ( 'NONE',  ( 0.3382312733057617482, 0.000000000000000000, -2.139420919314966252 ) ) ;
#17538 = VECTOR ( 'NONE', #4847, 39.37007874015748143 ) ;
#17539 = CARTESIAN_POINT ( 'NONE',  ( -0.5455278134075214336, 0.000000000000000000, -1.889763779527552146 ) ) ;
#17540 = ORIENTED_EDGE ( 'NONE', *, *, #50002, .T. ) ;
#17541 = EDGE_LOOP ( 'NONE', ( #14884, #40062, #40803, #32483 ) ) ;
#17542 = DIRECTION ( 'NONE',  ( 0.000000000000000000, -0.7660444431189770143, 0.6427876096865403621 ) ) ;
#17544 = CARTESIAN_POINT ( 'NONE',  ( -0.07591351300297340121, 0.000000000000000000, -1.929133858267710000 ) ) ;
#17543 = VECTOR ( 'NONE', #49233, 39.37007874015748854 ) ;
#17545 = FACE_BOUND ( 'NONE', #16482, .T. ) ;
#17546 = ORIENTED_EDGE ( 'NONE', *, *, #5179, .F. ) ;
#17547 = VECTOR ( 'NONE', #19137, 39.37007874015748143 ) ;
#17548 = VECTOR ( 'NONE', #5436, 39.37007874015748143 ) ;
#17549 = CARTESIAN_POINT ( 'NONE',  ( -0.5455278134075214336, 3.346456692913386100, 0.3149606299212577287 ) ) ;
#17550 = DIRECTION ( 'NONE',  ( 1.734723475976806848E-16, 0.000000000000000000, 1.000000000000000000 ) ) ;
#17551 = EDGE_CURVE ( 'NONE', #46022, #25081, #23413, .T. ) ;
#17552 = ORIENTED_EDGE ( 'NONE', *, *, #7895, .F. ) ;
#17553 = ORIENTED_EDGE ( 'NONE', *, *, #21936, .T. ) ;
#17554 = LINE ( 'NONE', #37950, #24125 ) ;
#17555 = FACE_OUTER_BOUND ( 'NONE', #10948, .T. ) ;
#17556 = ORIENTED_EDGE ( 'NONE', *, *, #34204, .T. ) ;
#17557 = ORIENTED_EDGE ( 'NONE', *, *, #3839, .T. ) ;
#17558 = EDGE_CURVE ( 'NONE', #44866, #11414, #27157, .T. ) ;
#17559 = VERTEX_POINT ( 'NONE', #50985 ) ;
#17560 = LINE ( 'NONE', #25303, #18608 ) ;
#17561 = CARTESIAN_POINT ( 'NONE',  ( 0.4330136603435741360, 0.5160455853568218787, -0.4330136603435745246 ) ) ;
#17562 = EDGE_CURVE ( 'NONE', #34870, #19370, #26785, .T. ) ;
#17563 = EDGE_CURVE ( 'NONE', #42223, #32548, #15170, .T. ) ;
#17564 = DIRECTION ( 'NONE',  ( -0.01601477604151182663, 0.9998717552508123996, -0.000000000000000000 ) ) ;
#17565 = PLANE ( 'NONE',  #18165 ) ;
#17566 = ORIENTED_EDGE ( 'NONE', *, *, #12867, .T. ) ;
#17567 = B_SPLINE_CURVE_WITH_KNOTS ( 'NONE', 3,
 ( #19667, #35943, #4700, #571 ),
 .UNSPECIFIED., .F., .F.,
 ( 4, 4 ),
 ( 2.102925087030960871E-07, 0.01994480150632338758 ),
 .UNSPECIFIED. ) ;
#17568 = ORIENTED_EDGE ( 'NONE', *, *, #27968, .T. ) ;
#17569 = DIRECTION ( 'NONE',  ( 1.000000000000000000, -0.000000000000000000, 0.000000000000000000 ) ) ;
#17570 = CARTESIAN_POINT ( 'NONE',  ( -1.166969139818015533, 0.000000000000000000, 0.4724409448818871482 ) ) ;
#17571 = CARTESIAN_POINT ( 'NONE',  ( -0.2727639067037607723, 0.000000000000000000, -1.732283464566922726 ) ) ;
#17572 = EDGE_CURVE ( 'NONE', #45000, #45220, #9212, .T. ) ;
#17573 = DIRECTION ( 'NONE',  ( -3.469446951953613696E-16, 0.000000000000000000, -1.000000000000000000 ) ) ;
#17574 = CARTESIAN_POINT ( 'NONE',  ( 1.015142113812069091, 3.226129038349118794, -2.244094488188969283 ) ) ;
#17575 = LINE ( 'NONE', #33340, #43278 ) ;
#17576 = CARTESIAN_POINT ( 'NONE',  ( -1.472219874544909768, 5.905511811023623991, 2.560030851058948453 ) ) ;
#17577 = VECTOR ( 'NONE', #12787, 39.37007874015748143 ) ;
#17578 = ORIENTED_EDGE ( 'NONE', *, *, #47002, .T. ) ;
#17579 = DIRECTION ( 'NONE',  ( -1.000000000000000000, -0.000000000000000000, -0.000000000000000000 ) ) ;
#17580 = CARTESIAN_POINT ( 'NONE',  ( 1.636583440222563857, 3.346456692913386100, -1.161035397307311917E-15 ) ) ;
#17581 = ORIENTED_EDGE ( 'NONE', *, *, #25489, .T. ) ;
#17582 = AXIS2_PLACEMENT_3D ( 'NONE', #27888, #24022, #32555 ) ;
#17584 = EDGE_CURVE ( 'NONE', #606, #30894, #24455, .T. ) ;
#17583 = VERTEX_POINT ( 'NONE', #1209 ) ;
#17585 = VECTOR ( 'NONE', #15717, 39.37007874015748143 ) ;
#17586 = DIRECTION ( 'NONE',  ( -1.000000000000000000, 0.000000000000000000, -0.000000000000000000 ) ) ;
#17587 = DIRECTION ( 'NONE',  ( -4.336808689942018969E-17, -5.168407336632174847E-17, -1.000000000000000000 ) ) ;
#17588 = ORIENTED_EDGE ( 'NONE', *, *, #21965, .F. ) ;
#17589 = EDGE_CURVE ( 'NONE', #21352, #34259, #33233, .T. ) ;
#17590 = EDGE_CURVE ( 'NONE', #47487, #19912, #48157, .T. ) ;
#17591 = VERTEX_POINT ( 'NONE', #16713 ) ;
#17592 = CARTESIAN_POINT ( 'NONE',  ( 1.181102362204724532, 0.5905511811023621549, 1.062992125984251413 ) ) ;
#17593 = ORIENTED_EDGE ( 'NONE', *, *, #2591, .F. ) ;
#17594 = DIRECTION ( 'NONE',  ( 1.734723475976806848E-16, -0.000000000000000000, 1.000000000000000000 ) ) ;
#17595 = CARTESIAN_POINT ( 'NONE',  ( -1.636583440222563857, 3.267716535433071279, 2.839019714148966584E-16 ) ) ;
#17596 = ADVANCED_FACE ( 'NONE', ( #25215 ), #28568, .T. ) ;
#17597 = VERTEX_POINT ( 'NONE', #43795 ) ;
#17598 = ORIENTED_EDGE ( 'NONE', *, *, #22695, .F. ) ;
#17599 = LINE ( 'NONE', #8832, #17241 ) ;
#17600 = ORIENTED_EDGE ( 'NONE', *, *, #2821, .T. ) ;
#17601 = ORIENTED_EDGE ( 'NONE', *, *, #32856, .T. ) ;
#17602 = CARTESIAN_POINT ( 'NONE',  ( 0.000000000000000000, 3.267716535433071279, -1.771653543307081025 ) ) ;
#17603 = CARTESIAN_POINT ( 'NONE',  ( 1.901865911302007106, 1.672747016891200200, -1.314378076695968511 ) ) ;
#17604 = CARTESIAN_POINT ( 'NONE',  ( 0.000000000000000000, 3.267716535433071279, 1.220472440944875281 ) ) ;
#17605 = VERTEX_POINT ( 'NONE', #24960 ) ;
#17606 = CARTESIAN_POINT ( 'NONE',  ( 0.7423782071083092626, 3.346456692913386100, 2.204724409448808764 ) ) ;
#17607 = CARTESIAN_POINT ( 'NONE',  ( -1.985260859929297572, 3.267716535433071279, -6.146657985744592735E-16 ) ) ;
#17608 = CARTESIAN_POINT ( 'NONE',  ( 0.8182917201112824834, 3.346456692913386100, 1.417322834645662777 ) ) ;
#17609 = EDGE_LOOP ( 'NONE', ( #3897, #41744, #32689, #25541 ) ) ;
#17610 = DIRECTION ( 'NONE',  ( 1.000000000000000000, -0.000000000000000000, 0.000000000000000000 ) ) ;
#17611 = AXIS2_PLACEMENT_3D ( 'NONE', #14755, #30502, #10873 ) ;
#17612 = CARTESIAN_POINT ( 'NONE',  ( 1.091055626815043311, 0.000000000000000000, 1.889763779527550369 ) ) ;
#17613 = PLANE ( 'NONE',  #8474 ) ;
#17614 = ORIENTED_EDGE ( 'NONE', *, *, #28629, .F. ) ;
#17615 = VECTOR ( 'NONE', #41970, 39.37007874015748143 ) ;
#17616 = VERTEX_POINT ( 'NONE', #17220 ) ;
#17617 =( NAMED_UNIT ( * ) SI_UNIT ( $, .STERADIAN. ) SOLID_ANGLE_UNIT ( ) );
#17618 = VECTOR ( 'NONE', #4603, 39.37007874015748143 ) ;
#17619 = VECTOR ( 'NONE', #9763, 39.37007874015748143 ) ;
#17620 = CARTESIAN_POINT ( 'NONE',  ( 1.091055626815042645, 3.346456692913386100, -0.3149606299212596716 ) ) ;
#17621 = EDGE_CURVE ( 'NONE', #50730, #19682, #40973, .T. ) ;
#17622 = EDGE_CURVE ( 'NONE', #21285, #25659, #40463, .T. ) ;
#17623 = LINE ( 'NONE', #36484, #47531 ) ;
#17624 = CARTESIAN_POINT ( 'NONE',  ( 1.091055626815042423, 3.346456692913386100, -1.574803149606294417 ) ) ;
#17625 = ORIENTED_EDGE ( 'NONE', *, *, #47329, .F. ) ;
#17627 = EDGE_CURVE ( 'NONE', #10406, #27808, #8700, .T. ) ;
#17626 = VERTEX_POINT ( 'NONE', #44053 ) ;
#17628 = AXIS2_PLACEMENT_3D ( 'NONE', #44232, #19962, #23851 ) ;
#17629 = DIRECTION ( 'NONE',  ( -0.000000000000000000, -1.000000000000000000, -0.000000000000000000 ) ) ;
#17630 = ORIENTED_EDGE ( 'NONE', *, *, #7047, .F. ) ;
#17631 = CARTESIAN_POINT ( 'NONE',  ( -1.363819533518803473, 3.346456692913386100, -0.1574803149606300023 ) ) ;
#17632 = DIRECTION ( 'NONE',  ( -0.9195277725514489076, 0.000000000000000000, -0.3930250316539278255 ) ) ;
#17633 = DIRECTION ( 'NONE',  ( -0.000000000000000000, 1.000000000000000000, -0.000000000000000000 ) ) ;
#17634 = CARTESIAN_POINT ( 'NONE',  ( 1.761123562704336232, 3.346456692913386100, -1.259842519685035800 ) ) ;
#17635 = DIRECTION ( 'NONE',  ( 0.000000000000000000, 0.000000000000000000, -1.000000000000000000 ) ) ;
#17636 = VERTEX_POINT ( 'NONE', #8448 ) ;
#17637 = LINE ( 'NONE', #41642, #42341 ) ;
#17638 = LINE ( 'NONE', #2404, #21079 ) ;
#17639 = EDGE_CURVE ( 'NONE', #13314, #40666, #1460, .T. ) ;
#17640 = CARTESIAN_POINT ( 'NONE',  ( 0.2156685157584260770, 1.722625337188476546, -2.945280361644574185 ) ) ;
#17641 = VERTEX_POINT ( 'NONE', #24713 ) ;
#17642 = FACE_OUTER_BOUND ( 'NONE', #1914, .T. ) ;
#17643 = EDGE_CURVE ( 'NONE', #9082, #8114, #49821, .T. ) ;
#17644 = CARTESIAN_POINT ( 'NONE',  ( -1.166969139818016199, 3.346456692913386100, -1.614173228346451605 ) ) ;
#17645 = LINE ( 'NONE', #3666, #12284 ) ;
#17646 = ORIENTED_EDGE ( 'NONE', *, *, #9407, .F. ) ;
#17647 = PLANE ( 'NONE',  #5227 ) ;
#17648 = ADVANCED_FACE ( 'NONE', ( #20577 ), #8957, .F. ) ;
#17649 = CARTESIAN_POINT ( 'NONE',  ( 1.761123562704338452, 3.346456692913386100, 1.259842519685033135 ) ) ;
#17650 = CIRCLE ( 'NONE', #7724, 2.165354330708661568 ) ;
#17651 = VECTOR ( 'NONE', #10075, 39.37007874015748143 ) ;
#17652 = EDGE_CURVE ( 'NONE', #5216, #6745, #20223, .T. ) ;
#17653 = VERTEX_POINT ( 'NONE', #4575 ) ;
#17654 = AXIS2_PLACEMENT_3D ( 'NONE', #48839, #41398, #44997 ) ;
#17655 = CARTESIAN_POINT ( 'NONE',  ( -2.160407304981126320, 1.574879494900809584, -0.1462862061266896330 ) ) ;
#17656 = CARTESIAN_POINT ( 'NONE',  ( 1.152568299495707826, 1.574803149606302854, 1.833124570921553120 ) ) ;
#17657 = ORIENTED_EDGE ( 'NONE', *, *, #37818, .F. ) ;
#17658 = LINE ( 'NONE', #47832, #10531 ) ;
#17659 = CIRCLE ( 'NONE', #21787, 2.165354330708661568 ) ;
#17660 = AXIS2_PLACEMENT_3D ( 'NONE', #20672, #29187, #36434 ) ;
#17661 = PLANE ( 'NONE',  #44904 ) ;
#17662 = FACE_OUTER_BOUND ( 'NONE', #42171, .T. ) ;
#17663 = CARTESIAN_POINT ( 'NONE',  ( -2.122484638469143814, 1.673906474958827939, -0.4339650761337435214 ) ) ;
#17664 = PLANE ( 'NONE',  #10611 ) ;
#17665 = ORIENTED_EDGE ( 'NONE', *, *, #7847, .T. ) ;
#17666 = VERTEX_POINT ( 'NONE', #1716 ) ;
#17667 = CARTESIAN_POINT ( 'NONE',  ( 0.07982360342473591996, 1.709180471932028711, 0.000000000000000000 ) ) ;
#17668 = AXIS2_PLACEMENT_3D ( 'NONE', #39280, #15537, #43137 ) ;
#17669 = DIRECTION ( 'NONE',  ( 1.000000000000000000, 0.000000000000000000, -3.469446951953613696E-16 ) ) ;
#17670 = ORIENTED_EDGE ( 'NONE', *, *, #21027, .T. ) ;
#17671 = DIRECTION ( 'NONE',  ( 1.000000000000000000, 0.000000000000000000, 0.000000000000000000 ) ) ;
#17672 = LINE ( 'NONE', #6307, #25983 ) ;
#17673 = DIRECTION ( 'NONE',  ( -0.000000000000000000, 1.000000000000000000, -0.000000000000000000 ) ) ;
#17674 = VERTEX_POINT ( 'NONE', #36587 ) ;
#17675 = ORIENTED_EDGE ( 'NONE', *, *, #29603, .F. ) ;
#17676 = CARTESIAN_POINT ( 'NONE',  ( -1.363819533518803473, 3.346456692913386100, -0.7874015748031470974 ) ) ;
#17677 = CARTESIAN_POINT ( 'NONE',  ( -1.166969139818016199, 0.000000000000000000, -0.6692913385826760875 ) ) ;
#17678 = DIRECTION ( 'NONE',  ( -0.000000000000000000, 1.000000000000000000, -0.000000000000000000 ) ) ;
#17679 = ORIENTED_EDGE ( 'NONE', *, *, #1723, .F. ) ;
#17680 = CARTESIAN_POINT ( 'NONE',  ( -1.091055626815042201, 3.346456692913386100, 1.377952755905504256 ) ) ;
#17681 = DIRECTION ( 'NONE',  ( -1.000000000000000000, 0.000000000000000000, 1.734723475976806848E-16 ) ) ;
#17682 = ORIENTED_EDGE ( 'NONE', *, *, #46072, .F. ) ;
#17683 = CARTESIAN_POINT ( 'NONE',  ( 1.363819533518803251, 0.000000000000000000, -0.7874015748031473194 ) ) ;
#17684 = VERTEX_POINT ( 'NONE', #16969 ) ;
#17685 = ORIENTED_EDGE ( 'NONE', *, *, #5404, .T. ) ;
#17686 = LINE ( 'NONE', #33453, #3156 ) ;
#17687 = CARTESIAN_POINT ( 'NONE',  ( 1.560669927219590303, 3.267716535433071279, -1.501022570047217508 ) ) ;
#17688 = EDGE_LOOP ( 'NONE', ( #43012, #45194, #31496, #11669 ) ) ;
#17689 = CARTESIAN_POINT ( 'NONE',  ( 1.393175312147112432, 0.000000000000000000, 1.048074961516293202 ) ) ;
#17690 = DIRECTION ( 'NONE',  ( -1.000000000000000000, 0.000000000000000000, -0.000000000000000000 ) ) ;
#17691 = ORIENTED_EDGE ( 'NONE', *, *, #16341, .F. ) ;
#17692 = VECTOR ( 'NONE', #12216, 39.37007874015748143 ) ;
#17693 = EDGE_CURVE ( 'NONE', #18779, #49170, #28827, .T. ) ;
#17694 = VECTOR ( 'NONE', #608, 39.37007874015748143 ) ;
#17695 = EDGE_CURVE ( 'NONE', #40865, #24856, #44816, .T. ) ;
#17696 = VECTOR ( 'NONE', #23411, 39.37007874015748143 ) ;
#17697 = CARTESIAN_POINT ( 'NONE',  ( -1.536664496436148184E-16, 0.000000000000000000, 0.4330708661417287386 ) ) ;
#17698 = EDGE_CURVE ( 'NONE', #41767, #19583, #701, .T. ) ;
#17699 = CARTESIAN_POINT ( 'NONE',  ( -1.909347346926324462, 3.346456692913386100, -0.1574803149606297248 ) ) ;
#17700 = VECTOR ( 'NONE', #4628, 39.37007874015748143 ) ;
#17701 = CIRCLE ( 'NONE', #35016, 2.165354330708661568 ) ;
#17702 = LINE ( 'NONE', #25696, #49475 ) ;
#17703 = PLANE ( 'NONE',  #3893 ) ;
#17704 = DIRECTION ( 'NONE',  ( -3.469446951953613696E-16, 0.000000000000000000, -1.000000000000000000 ) ) ;
#17705 = AXIS2_PLACEMENT_3D ( 'NONE', #39863, #42624, #8018 ) ;
#17706 = EDGE_LOOP ( 'NONE', ( #40966, #979, #30375, #44671 ) ) ;
#17707 = CARTESIAN_POINT ( 'NONE',  ( 2.721585451156246727, 1.452232124017870607, -1.145429582200450769 ) ) ;
#17708 = CARTESIAN_POINT ( 'NONE',  ( 0.000000000000000000, 5.905511811023623991, 0.000000000000000000 ) ) ;
#17709 = EDGE_LOOP ( 'NONE', ( #35840, #47136, #36664, #20364 ) ) ;
#17710 = LINE ( 'NONE', #16953, #21573 ) ;
#17711 = EDGE_CURVE ( 'NONE', #50549, #11356, #47897, .T. ) ;
#17712 = CARTESIAN_POINT ( 'NONE',  ( -0.3486774197067339376, 3.346456692913386100, -1.574803149606293529 ) ) ;
#17713 = VERTEX_POINT ( 'NONE', #49926 ) ;
#17714 = LINE ( 'NONE', #10474, #25470 ) ;
#17715 = CARTESIAN_POINT ( 'NONE',  ( 0.5455278134075208785, 3.346456692913386100, -1.574803149606293529 ) ) ;
#17716 = ADVANCED_FACE ( 'NONE', ( #49427 ), #26229, .T. ) ;
#17717 = ORIENTED_EDGE ( 'NONE', *, *, #6892, .F. ) ;
#17718 = DIRECTION ( 'NONE',  ( 1.000000000000000000, 0.000000000000000000, 0.000000000000000000 ) ) ;
#17719 = ORIENTED_EDGE ( 'NONE', *, *, #47823, .T. ) ;
#17720 = FACE_BOUND ( 'NONE', #9581, .T. ) ;
#17721 = FACE_OUTER_BOUND ( 'NONE', #18157, .T. ) ;
#17722 = DIRECTION ( 'NONE',  ( -0.01601477604151182663, 0.9998717552508123996, -0.000000000000000000 ) ) ;
#17723 = CARTESIAN_POINT ( 'NONE',  ( 1.287906020515830585, 3.346456692913386100, 1.740706023381843659 ) ) ;
#17724 = APPLICATION_CONTEXT ( 'automotive_design' ) ;
#17725 = ORIENTED_EDGE ( 'NONE', *, *, #49867, .T. ) ;
#17726 = EDGE_LOOP ( 'NONE', ( #31883, #31739, #22790, #1194 ) ) ;
#17727 = AXIS2_PLACEMENT_3D ( 'NONE', #44414, #40557, #20933 ) ;
#17728 = CARTESIAN_POINT ( 'NONE',  ( 1.183645401082124904, 0.000000000000000000, 1.279993023352361980 ) ) ;
#17729 = ORIENTED_EDGE ( 'NONE', *, *, #6485, .F. ) ;
#17730 = CIRCLE ( 'NONE', #22699, 2.165354330708661568 ) ;
#17731 = DIRECTION ( 'NONE',  ( 0.000000000000000000, 0.000000000000000000, 1.000000000000000000 ) ) ;
#17732 = ORIENTED_EDGE ( 'NONE', *, *, #49031, .T. ) ;
#17733 = VECTOR ( 'NONE', #16646, 39.37007874015748143 ) ;
#17734 = LINE ( 'NONE', #18994, #41326 ) ;
#17735 = ORIENTED_EDGE ( 'NONE', *, *, #47037, .F. ) ;
#17736 = LINE ( 'NONE', #9483, #10944 ) ;
#17737 = CARTESIAN_POINT ( 'NONE',  ( 1.636583440222563635, 3.346456692913386100, -1.259842519685035800 ) ) ;
#17738 = VECTOR ( 'NONE', #50729, 39.37007874015748143 ) ;
#17739 = ORIENTED_EDGE ( 'NONE', *, *, #5455, .F. ) ;
#17740 = LINE ( 'NONE', #45582, #16705 ) ;
#17741 = VERTEX_POINT ( 'NONE', #18486 ) ;
#17742 = VERTEX_POINT ( 'NONE', #21597 ) ;
#17743 = ORIENTED_EDGE ( 'NONE', *, *, #23933, .T. ) ;
#17744 = ORIENTED_EDGE ( 'NONE', *, *, #36865, .F. ) ;
#17745 = CARTESIAN_POINT ( 'NONE',  ( -1.091055626815042201, 3.346456692913386100, 0.3149606299212580063 ) ) ;
#17746 = EDGE_CURVE ( 'NONE', #31458, #37657, #10230, .T. ) ;
#17747 = ADVANCED_FACE ( 'NONE', ( #26472 ), #9726, .F. ) ;
#17748 = ORIENTED_EDGE ( 'NONE', *, *, #37396, .F. ) ;
#17749 = FACE_OUTER_BOUND ( 'NONE', #764, .T. ) ;
#17750 = PLANE ( 'NONE',  #13713 ) ;
#17751 = EDGE_CURVE ( 'NONE', #12958, #27093, #2735, .T. ) ;
#17752 = EDGE_CURVE ( 'NONE', #18200, #36096, #41980, .T. ) ;
#17753 = CARTESIAN_POINT ( 'NONE',  ( -1.091055626815042201, 3.267716535433071279, 1.259842519685033357 ) ) ;
#17754 = ORIENTED_EDGE ( 'NONE', *, *, #4071, .F. ) ;
#17755 = FACE_OUTER_BOUND ( 'NONE', #41403, .T. ) ;
#17756 = DIRECTION ( 'NONE',  ( -0.6427876096865403621, 0.7660444431189770143, 0.000000000000000000 ) ) ;
#17757 = VECTOR ( 'NONE', #4361, 39.37007874015748143 ) ;
#17758 = ORIENTED_EDGE ( 'NONE', *, *, #24167, .T. ) ;
#17759 = LINE ( 'NONE', #17505, #43097 ) ;
#17760 = DIRECTION ( 'NONE',  ( 1.000000000000000000, -0.000000000000000000, 0.000000000000000000 ) ) ;
#17761 = DIRECTION ( 'NONE',  ( 1.000000000000000000, 0.000000000000000000, 0.000000000000000000 ) ) ;
#17762 = VECTOR ( 'NONE', #15300, 39.37007874015748143 ) ;
#17763 = LINE ( 'NONE', #33782, #37193 ) ;
#17764 = B_SPLINE_CURVE_WITH_KNOTS ( 'NONE', 3,
 ( #35193, #31321, #50872, #15813 ),
 .UNSPECIFIED., .F., .F.,
 ( 4, 4 ),
 ( 0.1211775127643062444, 0.1625894504277921315 ),
 .UNSPECIFIED. ) ;
#17765 = CARTESIAN_POINT ( 'NONE',  ( 0.7368177193319344065, 0.01309245855044433200, 1.823186522806556686 ) ) ;
#17766 = EDGE_CURVE ( 'NONE', #32953, #17017, #18230, .T. ) ;
#17767 = LINE ( 'NONE', #25763, #16206 ) ;
#17768 = ORIENTED_EDGE ( 'NONE', *, *, #6394, .T. ) ;
#17769 = CARTESIAN_POINT ( 'NONE',  ( 0.4696143004045478797, 3.267716535433071279, -1.614173228346451605 ) ) ;
#17770 = LINE ( 'NONE', #41271, #44870 ) ;
#17771 = AXIS2_PLACEMENT_3D ( 'NONE', #890, #4509, #27993 ) ;
#17772 = ORIENTED_EDGE ( 'NONE', *, *, #10557, .T. ) ;
#17773 = DIRECTION ( 'NONE',  ( -0.000000000000000000, 1.000000000000000000, -0.000000000000000000 ) ) ;
#17774 = EDGE_CURVE ( 'NONE', #49369, #11755, #48913, .T. ) ;
#17775 = EDGE_LOOP ( 'NONE', ( #9274, #3668, #5963, #43502 ) ) ;
#17776 = DIRECTION ( 'NONE',  ( -0.000000000000000000, 1.000000000000000000, -0.000000000000000000 ) ) ;
#17777 = CARTESIAN_POINT ( 'NONE',  ( -2.044241703397525978, 1.205361022782829114E-17, -0.7159595814952911530 ) ) ;
#17778 = CARTESIAN_POINT ( 'NONE',  ( -0.6094175224461334528, 1.205361022782829114E-17, 1.763844451117148271 ) ) ;
#17779 = DIRECTION ( 'NONE',  ( -0.000000000000000000, 1.000000000000000000, -0.000000000000000000 ) ) ;
#17780 = DIRECTION ( 'NONE',  ( -0.000000000000000000, 0.000000000000000000, 1.000000000000000000 ) ) ;
#17781 = VERTEX_POINT ( 'NONE', #22361 ) ;
#17782 = EDGE_CURVE ( 'NONE', #28960, #18289, #6364, .T. ) ;
#17783 = CARTESIAN_POINT ( 'NONE',  ( 0.000000000000000000, 3.267716535433071279, -2.244094488188968395 ) ) ;
#17784 = ORIENTED_EDGE ( 'NONE', *, *, #47553, .T. ) ;
#17785 = CARTESIAN_POINT ( 'NONE',  ( 1.325491792074623643, 1.485765544018708750, -2.638988599164732385 ) ) ;
#17786 = ORIENTED_EDGE ( 'NONE', *, *, #17698, .T. ) ;
#17787 = CARTESIAN_POINT ( 'NONE',  ( 1.429658358381396877, 0.01654809226879937895, -1.434979885194824112 ) ) ;
#17788 = DIRECTION ( 'NONE',  ( 1.000000000000000000, 0.000000000000000000, 0.000000000000000000 ) ) ;
#17789 = EDGE_CURVE ( 'NONE', #13301, #31303, #14357, .T. ) ;
#17790 = EDGE_LOOP ( 'NONE', ( #6220, #42538, #9872, #13053 ) ) ;
#17791 = PLANE ( 'NONE',  #33044 ) ;
#17792 = CARTESIAN_POINT ( 'NONE',  ( 1.975114622544695386, 0.03906914021382532770, -0.4003288316781843936 ) ) ;
#17793 = CARTESIAN_POINT ( 'NONE',  ( 2.088343298084792021, 5.905511811023623991, 0.6267986818430609786 ) ) ;
#17794 = B_SPLINE_CURVE_WITH_KNOTS ( 'NONE', 3,
 ( #49460, #3031, #45863, #49214 ),
 .UNSPECIFIED., .F., .F.,
 ( 4, 4 ),
 ( 0.01212773829365105735, 0.03073793659894883193 ),
 .UNSPECIFIED. ) ;
#17795 = ORIENTED_EDGE ( 'NONE', *, *, #44380, .T. ) ;
#17796 = ORIENTED_EDGE ( 'NONE', *, *, #17643, .T. ) ;
#17797 = CIRCLE ( 'NONE', #35109, 1.850107469027523432 ) ;
#17798 = LINE ( 'NONE', #40531, #43804 ) ;
#17799 = FACE_BOUND ( 'NONE', #37113, .T. ) ;
#17800 = ORIENTED_EDGE ( 'NONE', *, *, #3252, .T. ) ;
#17801 = AXIS2_PLACEMENT_3D ( 'NONE', #32409, #48355, #24395 ) ;
#17802 = LINE ( 'NONE', #5924, #29516 ) ;
#17803 = CARTESIAN_POINT ( 'NONE',  ( 0.000000000000000000, 3.267716535433071279, -1.456692913385823296 ) ) ;
#17804 = VECTOR ( 'NONE', #2629, 39.37007874015748143 ) ;
#17805 = ORIENTED_EDGE ( 'NONE', *, *, #3003, .T. ) ;
#17806 = ORIENTED_EDGE ( 'NONE', *, *, #49711, .F. ) ;
#17807 = CARTESIAN_POINT ( 'NONE',  ( -0.6377510516001282381, 1.027715665865251315, -2.495823182398442697 ) ) ;
#17808 = VECTOR ( 'NONE', #7188, 39.37007874015748143 ) ;
#17809 = DIRECTION ( 'NONE',  ( 0.000000000000000000, 0.000000000000000000, 1.000000000000000000 ) ) ;
#17810 = VERTEX_POINT ( 'NONE', #14102 ) ;
#17811 = EDGE_LOOP ( 'NONE', ( #11204, #41531, #5421, #40415 ) ) ;
#17812 = VERTEX_POINT ( 'NONE', #6099 ) ;
#17813 = CARTESIAN_POINT ( 'NONE',  ( -2.101391096692225791, 1.575819129783617489, -0.5301069970517552354 ) ) ;
#17814 = EDGE_CURVE ( 'NONE', #49632, #23850, #6617, .T. ) ;
#17815 = DIRECTION ( 'NONE',  ( -0.000000000000000000, 0.000000000000000000, 1.000000000000000000 ) ) ;
#17816 = EDGE_CURVE ( 'NONE', #14372, #23850, #10487, .T. ) ;
#17817 = DIRECTION ( 'NONE',  ( -1.000000000000000000, -0.000000000000000000, -0.000000000000000000 ) ) ;
#17818 = EDGE_CURVE ( 'NONE', #18090, #6701, #45822, .T. ) ;
#17819 = LINE ( 'NONE', #3845, #41246 ) ;
#17820 = ORIENTED_EDGE ( 'NONE', *, *, #14346, .F. ) ;
#17821 = ORIENTED_EDGE ( 'NONE', *, *, #19155, .F. ) ;
#17822 = CARTESIAN_POINT ( 'NONE',  ( 0.6551740444401462637, 0.000000000000000000, 1.885762267972743711 ) ) ;
#17823 = FACE_OUTER_BOUND ( 'NONE', #8528, .T. ) ;
#17824 = CARTESIAN_POINT ( 'NONE',  ( 0.000000000000000000, 3.267716535433071279, -1.456692913385822630 ) ) ;
#17825 = LINE ( 'NONE', #2081, #42445 ) ;
#17826 = CARTESIAN_POINT ( 'NONE',  ( 0.000000000000000000, 3.267716535433071279, 0.000000000000000000 ) ) ;
#17827 = CARTESIAN_POINT ( 'NONE',  ( 2.372989701366758020, 3.242957824277338030, 0.6299212598425161236 ) ) ;
#17828 = CIRCLE ( 'NONE', #46647, 2.874015748031496731 ) ;
#17829 = CARTESIAN_POINT ( 'NONE',  ( -0.8182917201112819283, 3.346456692913386100, -1.102362204724405492 ) ) ;
#17830 = ORIENTED_EDGE ( 'NONE', *, *, #15675, .F. ) ;
#17831 = AXIS2_PLACEMENT_3D ( 'NONE', #21711, #21202, #49286 ) ;
#17832 = CARTESIAN_POINT ( 'NONE',  ( -0.5284761224300577043, 5.905511811023623991, -2.099874368989737228 ) ) ;
#17833 = DIRECTION ( 'NONE',  ( 1.000000000000000000, 0.000000000000000000, 0.000000000000000000 ) ) ;
#17834 = VECTOR ( 'NONE', #26505, 39.37007874015748143 ) ;
#17835 = ORIENTED_EDGE ( 'NONE', *, *, #10826, .F. ) ;
#17836 = VECTOR ( 'NONE', #35189, 39.37007874015748143 ) ;
#17837 = VERTEX_POINT ( 'NONE', #41728 ) ;
#17838 = CARTESIAN_POINT ( 'NONE',  ( 0.9671406142315196464, 3.267716535433070391, -2.244094488188969283 ) ) ;
#17839 = VECTOR ( 'NONE', #8924, 39.37007874015748143 ) ;
#17840 = VERTEX_POINT ( 'NONE', #18739 ) ;
#17841 = EDGE_CURVE ( 'NONE', #6632, #37350, #13600, .T. ) ;
#17842 = CIRCLE ( 'NONE', #35160, 1.850107469027523432 ) ;
#17843 = B_SPLINE_CURVE_WITH_KNOTS ( 'NONE', 3,
 ( #654, #48109, #46397, #31907 ),
 .UNSPECIFIED., .F., .F.,
 ( 4, 4 ),
 ( 2.074264429158795827E-07, 0.002500727467959800148 ),
 .UNSPECIFIED. ) ;
#17844 = ORIENTED_EDGE ( 'NONE', *, *, #42017, .F. ) ;
#17845 = PLANE ( 'NONE',  #3977 ) ;
#17846 = EDGE_CURVE ( 'NONE', #30518, #20081, #45568, .T. ) ;
#17847 = ORIENTED_EDGE ( 'NONE', *, *, #6356, .F. ) ;
#17848 = CARTESIAN_POINT ( 'NONE',  ( -2.889674983507169337, 1.674218314264582785, -0.6090712660038034576 ) ) ;
#17849 = CARTESIAN_POINT ( 'NONE',  ( 0.000000000000000000, 3.267716535433071279, -1.456692913385822186 ) ) ;
#17850 = ADVANCED_FACE ( 'NONE', ( #41225 ), #13852, .F. ) ;
#17851 = ORIENTED_EDGE ( 'NONE', *, *, #23638, .F. ) ;
#17852 = ORIENTED_EDGE ( 'NONE', *, *, #29005, .F. ) ;
#17853 = LINE ( 'NONE', #18871, #13151 ) ;
#17854 = VERTEX_POINT ( 'NONE', #41472 ) ;
#17855 = ORIENTED_EDGE ( 'NONE', *, *, #22148, .F. ) ;
#17856 = ADVANCED_FACE ( 'NONE', ( #17974 ), #22109, .F. ) ;
#17857 = CARTESIAN_POINT ( 'NONE',  ( -2.443311489867025621, 3.267716535433071279, -0.03937007874015881204 ) ) ;
#17858 = CARTESIAN_POINT ( 'NONE',  ( -1.091055626815042201, 0.000000000000000000, 0.6299212598425164567 ) ) ;
#17859 = CARTESIAN_POINT ( 'NONE',  ( -0.8182917201112819283, 3.267716535433071279, -2.244094488188968395 ) ) ;
#17860 = EDGE_CURVE ( 'NONE', #22211, #42163, #11740, .T. ) ;
#17861 = ORIENTED_EDGE ( 'NONE', *, *, #47739, .F. ) ;
#17862 = LINE ( 'NONE', #37241, #23833 ) ;
#17863 = DIRECTION ( 'NONE',  ( 0.000000000000000000, 0.000000000000000000, 1.000000000000000000 ) ) ;
#17864 = DIRECTION ( 'NONE',  ( -0.000000000000000000, 1.000000000000000000, -0.000000000000000000 ) ) ;
#17865 = CIRCLE ( 'NONE', #3856, 0.3937007874015748254 ) ;
#17866 = ORIENTED_EDGE ( 'NONE', *, *, #18195, .F. ) ;
#17867 = DIRECTION ( 'NONE',  ( 0.000000000000000000, 0.000000000000000000, -1.000000000000000000 ) ) ;
#17868 = DIRECTION ( 'NONE',  ( -0.000000000000000000, 1.000000000000000000, -0.000000000000000000 ) ) ;
#17869 = AXIS2_PLACEMENT_3D ( 'NONE', #38958, #19324, #43066 ) ;
#17870 = VECTOR ( 'NONE', #49398, 39.37007874015748143 ) ;
#17871 = CARTESIAN_POINT ( 'NONE',  ( 0.000000000000000000, 3.267716535433071279, 1.535433070866133898 ) ) ;
#17872 = ORIENTED_EDGE ( 'NONE', *, *, #23109, .T. ) ;
#17873 = ORIENTED_EDGE ( 'NONE', *, *, #26502, .F. ) ;
#17874 = SHAPE_REPRESENTATION_RELATIONSHIP ( 'NONE' , 'NONE' ,  #8330, #43986 ) ;
#17875 = EDGE_CURVE ( 'NONE', #4281, #44874, #27481, .T. ) ;
#17876 = CARTESIAN_POINT ( 'NONE',  ( -0.8182917201112819283, 3.346456692913386100, -0.7874015748031467643 ) ) ;
#17877 = CIRCLE ( 'NONE', #547, 0.3740157480314960647 ) ;
#17878 = CARTESIAN_POINT ( 'NONE',  ( -1.091055626815042645, 0.000000000000000000, -0.5118110236220467790 ) ) ;
#17879 = EDGE_CURVE ( 'NONE', #29609, #30462, #47065, .T. ) ;
#17880 = EDGE_CURVE ( 'NONE', #16054, #14478, #15861, .T. ) ;
#17881 = CARTESIAN_POINT ( 'NONE',  ( -1.109524193798323788, 0.000000000000000000, 1.344750771968458380 ) ) ;
#17882 = VERTEX_POINT ( 'NONE', #4002 ) ;
#17883 = ORIENTED_EDGE ( 'NONE', *, *, #25382, .F. ) ;
#17884 = AXIS2_PLACEMENT_3D ( 'NONE', #18179, #50128, #29546 ) ;
#17885 = EDGE_CURVE ( 'NONE', #23291, #42847, #3494, .T. ) ;
#17886 = CARTESIAN_POINT ( 'NONE',  ( 0.002207914879453961969, 6.692913385826772199, 0.04916304461325451958 ) ) ;
#17887 = ORIENTED_EDGE ( 'NONE', *, *, #34299, .F. ) ;
#17888 = DIRECTION ( 'NONE',  ( 1.000000000000000000, 0.000000000000000000, -3.469446951953613696E-16 ) ) ;
#17889 = CARTESIAN_POINT ( 'NONE',  ( -2.623503965249869729, 1.678368413758691391, 1.355882097269835107 ) ) ;
#17890 = DIRECTION ( 'NONE',  ( 0.9510565162951500895, 0.000000000000000000, 0.3090169943749582204 ) ) ;
#17891 = LINE ( 'NONE', #40877, #18641 ) ;
#17892 = CARTESIAN_POINT ( 'NONE',  ( 0.08139965876239094178, 1.610780518492231694, 0.000000000000000000 ) ) ;
#17893 = ORIENTED_EDGE ( 'NONE', *, *, #30052, .T. ) ;
#17894 = CARTESIAN_POINT ( 'NONE',  ( -2.121605289024800722, 3.267716535433071279, 0.4330708661417290162 ) ) ;
#17895 = FACE_OUTER_BOUND ( 'NONE', #48579, .T. ) ;
#17896 = CARTESIAN_POINT ( 'NONE',  ( 0.4696143004045479352, 0.000000000000000000, -0.7874015748031473194 ) ) ;
#17897 = ORIENTED_EDGE ( 'NONE', *, *, #12572, .F. ) ;
#17898 = CARTESIAN_POINT ( 'NONE',  ( -0.7053729475263578186, 3.346456692913386100, -2.047244094488181343 ) ) ;
#17899 = FACE_OUTER_BOUND ( 'NONE', #41816, .T. ) ;
#17900 = PLANE ( 'NONE',  #27922 ) ;
#17901 = ORIENTED_EDGE ( 'NONE', *, *, #12189, .T. ) ;
#17902 = AXIS2_PLACEMENT_3D ( 'NONE', #2719, #9964, #17452 ) ;
#17903 = EDGE_CURVE ( 'NONE', #47182, #12647, #50669, .T. ) ;
#17904 = CARTESIAN_POINT ( 'NONE',  ( 0.000000000000000000, 3.267716535433071279, -0.9448818897637765168 ) ) ;
#17905 = VECTOR ( 'NONE', #27776, 39.37007874015748143 ) ;
#17906 = VERTEX_POINT ( 'NONE', #11998 ) ;
#17907 = DIRECTION ( 'NONE',  ( -0.9510565162951500895, 0.000000000000000000, -0.3090169943749582204 ) ) ;
#17908 = CARTESIAN_POINT ( 'NONE',  ( -0.01641453323182725382, 1.514958906868826061, 2.952755905511811108 ) ) ;
#17909 = ORIENTED_EDGE ( 'NONE', *, *, #33596, .T. ) ;
#17910 = CARTESIAN_POINT ( 'NONE',  ( 1.037524086854322514, 0.000000000000000000, 2.764473043227584803 ) ) ;
#17911 = EDGE_CURVE ( 'NONE', #34814, #19095, #35496, .T. ) ;
#17912 = CARTESIAN_POINT ( 'NONE',  ( 0.6160390700230953254, 1.623012950100491958, -2.417151584004514131 ) ) ;
#17913 = CYLINDRICAL_SURFACE ( 'NONE', #37905, 2.165354330708661568 ) ;
#17914 = DIRECTION ( 'NONE',  ( -0.000000000000000000, 1.000000000000000000, -0.000000000000000000 ) ) ;
#17915 = ADVANCED_FACE ( 'NONE', ( #46573 ), #11244, .F. ) ;
#17916 = ADVANCED_FACE ( 'NONE', ( #10987 ), #50923, .F. ) ;
#17917 = DIRECTION ( 'NONE',  ( -0.000000000000000000, 1.000000000000000000, -0.000000000000000000 ) ) ;
#17918 = ORIENTED_EDGE ( 'NONE', *, *, #24324, .T. ) ;
#17919 = ORIENTED_EDGE ( 'NONE', *, *, #33964, .T. ) ;
#17920 = CARTESIAN_POINT ( 'NONE',  ( 0.1968503937007878568, 0.000000000000000000, 1.259842519685033357 ) ) ;
#17921 = CARTESIAN_POINT ( 'NONE',  ( 1.331808205664952505, 0.000000000000000000, 1.125026879082043685 ) ) ;
#17922 = ORIENTED_EDGE ( 'NONE', *, *, #6588, .F. ) ;
#17923 = CARTESIAN_POINT ( 'NONE',  ( 0.5455278134075212115, 3.346456692913386100, 0.3149606299212576177 ) ) ;
#17924 = CARTESIAN_POINT ( 'NONE',  ( -1.083598637574820334, 1.603934357758587614, 2.747180975113330259 ) ) ;
#17925 = LINE ( 'NONE', #18689, #33560 ) ;
#17926 = AXIS2_PLACEMENT_3D ( 'NONE', #22394, #46111, #45600 ) ;
#17927 = ORIENTED_EDGE ( 'NONE', *, *, #9244, .T. ) ;
#17928 = VERTEX_POINT ( 'NONE', #26973 ) ;
#17929 = CARTESIAN_POINT ( 'NONE',  ( 0.000000000000000000, 3.267716535433071279, -0.03937007874015881204 ) ) ;
#17930 = CARTESIAN_POINT ( 'NONE',  ( -1.195183497228115035E-16, 3.346456692913386100, -0.9448818897637765168 ) ) ;
#17931 = LINE ( 'NONE', #36795, #43667 ) ;
#17932 = EDGE_CURVE ( 'NONE', #42532, #31299, #39112, .T. ) ;
#17933 = EDGE_LOOP ( 'NONE', ( #49101, #49208, #25356, #23548 ) ) ;
#17934 = LINE ( 'NONE', #10695, #37264 ) ;
#17935 = FACE_BOUND ( 'NONE', #24476, .T. ) ;
#17936 = ORIENTED_EDGE ( 'NONE', *, *, #24220, .F. ) ;
#17937 = DIRECTION ( 'NONE',  ( -0.000000000000000000, 1.000000000000000000, -0.000000000000000000 ) ) ;
#17938 = EDGE_LOOP ( 'NONE', ( #47291, #14978, #31411, #41623 ) ) ;
#17939 = VERTEX_POINT ( 'NONE', #23611 ) ;
#17940 = EDGE_CURVE ( 'NONE', #33992, #44975, #19481, .T. ) ;
#17941 = DIRECTION ( 'NONE',  ( -1.000000000000000000, 0.000000000000000000, -0.000000000000000000 ) ) ;
#17942 = CARTESIAN_POINT ( 'NONE',  ( 0.000000000000000000, 5.905511811023623991, 0.000000000000000000 ) ) ;
#17943 = VECTOR ( 'NONE', #3699, 39.37007874015748143 ) ;
#17944 = VECTOR ( 'NONE', #6222, 39.37007874015748143 ) ;
#17945 = VERTEX_POINT ( 'NONE', #31624 ) ;
#17946 = CARTESIAN_POINT ( 'NONE',  ( 2.122900538663711867, 1.752334412280341258, -2.052396120422125048 ) ) ;
#17947 = EDGE_CURVE ( 'NONE', #48074, #14448, #27228, .T. ) ;
#17948 = CARTESIAN_POINT ( 'NONE',  ( -0.2727639067037608278, 3.346456692913386100, -0.3543307086614175816 ) ) ;
#17949 = ORIENTED_EDGE ( 'NONE', *, *, #38927, .T. ) ;
#17950 = EDGE_CURVE ( 'NONE', #37274, #23861, #38613, .T. ) ;
#17951 = DIRECTION ( 'NONE',  ( 0.000000000000000000, 0.000000000000000000, -1.000000000000000000 ) ) ;
#17952 = DIRECTION ( 'NONE',  ( -3.469446951953613696E-16, 0.000000000000000000, -1.000000000000000000 ) ) ;
#17953 = CARTESIAN_POINT ( 'NONE',  ( -2.182111253630085734, 3.240462944951739033, -1.127888942729357469 ) ) ;
#17954 = CARTESIAN_POINT ( 'NONE',  ( -1.670787592146344203, 0.000000000000000000, 0.5255918861343552573 ) ) ;
#17955 = CARTESIAN_POINT ( 'NONE',  ( -1.905671854841497481, 1.555429617898292705, 2.256015092822653667 ) ) ;
#17956 = VERTEX_POINT ( 'NONE', #18985 ) ;
#17957 = FACE_OUTER_BOUND ( 'NONE', #19951, .T. ) ;
#17958 = AXIS2_PLACEMENT_3D ( 'NONE', #22089, #5572, #33968 ) ;
#17959 = CARTESIAN_POINT ( 'NONE',  ( 1.091055626815043311, 3.267716535433071279, 1.870389530743258755 ) ) ;
#17960 = ORIENTED_EDGE ( 'NONE', *, *, #24940, .T. ) ;
#17961 = CARTESIAN_POINT ( 'NONE',  ( 0.000000000000000000, 6.692913385826772199, 0.000000000000000000 ) ) ;
#17962 = DIRECTION ( 'NONE',  ( -0.000000000000000000, 1.000000000000000000, -0.000000000000000000 ) ) ;
#17963 = ORIENTED_EDGE ( 'NONE', *, *, #22650, .T. ) ;
#17964 = DIRECTION ( 'NONE',  ( -1.000000000000000000, 0.000000000000000000, 0.000000000000000000 ) ) ;
#17965 = DIRECTION ( 'NONE',  ( 1.734723475976806848E-16, -0.000000000000000000, 1.000000000000000000 ) ) ;
#17966 = CARTESIAN_POINT ( 'NONE',  ( 0.000000000000000000, 3.267716535433071279, -0.3149606299212592275 ) ) ;
#17967 = EDGE_LOOP ( 'NONE', ( #34372, #46874, #33197, #11350 ) ) ;
#17968 = CARTESIAN_POINT ( 'NONE',  ( -0.04921259842519708910, 1.718497255264965551, 2.952755905511811108 ) ) ;
#17969 = B_SPLINE_CURVE_WITH_KNOTS ( 'NONE', 3,
 ( #16286, #38768, #35909, #3397 ),
 .UNSPECIFIED., .F., .F.,
 ( 4, 4 ),
 ( 2.008317325138464645E-07, 0.002500501682857974185 ),
 .UNSPECIFIED. ) ;
#17970 = ORIENTED_EDGE ( 'NONE', *, *, #42863, .T. ) ;
#17971 = LINE ( 'NONE', #33739, #30324 ) ;
#17972 = CARTESIAN_POINT ( 'NONE',  ( 0.2727639067037604947, 3.267716535433071279, -1.102362204724405714 ) ) ;
#17973 = CARTESIAN_POINT ( 'NONE',  ( -0.5455278134075216556, 3.254044873612428557, -2.388497533030866204 ) ) ;
#17974 = FACE_OUTER_BOUND ( 'NONE', #24675, .T. ) ;
#17975 = EDGE_CURVE ( 'NONE', #32481, #39570, #31372, .T. ) ;
#17976 = VECTOR ( 'NONE', #37031, 39.37007874015748143 ) ;
#17977 = VECTOR ( 'NONE', #31744, 39.37007874015748143 ) ;
#17978 = EDGE_CURVE ( 'NONE', #7934, #24890, #32016, .T. ) ;
#17979 = ORIENTED_EDGE ( 'NONE', *, *, #8082, .F. ) ;
#17980 = ORIENTED_EDGE ( 'NONE', *, *, #18396, .T. ) ;
#17981 = EDGE_CURVE ( 'NONE', #23434, #3623, #43223, .T. ) ;
#17982 = DIRECTION ( 'NONE',  ( 0.000000000000000000, 1.000000000000000000, 0.000000000000000000 ) ) ;
#17983 = VECTOR ( 'NONE', #11073, 39.37007874015748143 ) ;
#17984 = CARTESIAN_POINT ( 'NONE',  ( -0.07591351300297340121, 3.346456692913386100, -0.6692913385826758654 ) ) ;
#17985 = ORIENTED_EDGE ( 'NONE', *, *, #50061, .F. ) ;
#17986 = DIRECTION ( 'NONE',  ( 0.000000000000000000, 1.000000000000000000, 0.000000000000000000 ) ) ;
#17987 = VECTOR ( 'NONE', #20112, 39.37007874015748143 ) ;
#17988 = VERTEX_POINT ( 'NONE', #34739 ) ;
#17989 = CARTESIAN_POINT ( 'NONE',  ( 0.000000000000000000, 3.346456692913386100, 0.000000000000000000 ) ) ;
#17990 = CIRCLE ( 'NONE', #1477, 0.3740157480314960647 ) ;
#17991 = CARTESIAN_POINT ( 'NONE',  ( 2.455254121199802686, 1.757512009626756244, -1.640354758320677453 ) ) ;
#17992 = ORIENTED_EDGE ( 'NONE', *, *, #29661, .T. ) ;
#17993 = CARTESIAN_POINT ( 'NONE',  ( 0.000000000000000000, 3.267716535433071279, -1.929133858267711110 ) ) ;
#17994 = EDGE_LOOP ( 'NONE', ( #28270, #7947, #12337 ) ) ;
#17995 = ORIENTED_EDGE ( 'NONE', *, *, #46072, .T. ) ;
#17996 = EDGE_CURVE ( 'NONE', #35748, #28425, #35831, .T. ) ;
#17997 = VECTOR ( 'NONE', #46981, 39.37007874015748143 ) ;
#17998 = EDGE_CURVE ( 'NONE', #58, #24845, #8384, .T. ) ;
#17999 = ORIENTED_EDGE ( 'NONE', *, *, #50553, .T. ) ;
#18000 = ORIENTED_EDGE ( 'NONE', *, *, #7697, .F. ) ;
#18001 = PLANE ( 'NONE',  #49952 ) ;
#18002 = ADVANCED_FACE ( 'NONE', ( #25152 ), #44750, .F. ) ;
#18003 = ORIENTED_EDGE ( 'NONE', *, *, #13143, .T. ) ;
#18004 = CARTESIAN_POINT ( 'NONE',  ( -2.151809081513409438, 6.692913385826772199, 0.2418202932658334581 ) ) ;
#18005 = EDGE_CURVE ( 'NONE', #16878, #8594, #20246, .T. ) ;
#18006 = DIRECTION ( 'NONE',  ( -0.000000000000000000, 1.000000000000000000, -0.000000000000000000 ) ) ;
#18007 = VECTOR ( 'NONE', #8565, 39.37007874015748143 ) ;
#18008 = DIRECTION ( 'NONE',  ( 1.734723475976806848E-16, 0.000000000000000000, 1.000000000000000000 ) ) ;
#18009 = B_SPLINE_CURVE_WITH_KNOTS ( 'NONE', 3,
 ( #15382, #11753, #7632, #4261 ),
 .UNSPECIFIED., .F., .F.,
 ( 4, 4 ),
 ( 2.472340750494697777E-07, 0.002500446055397966515 ),
 .UNSPECIFIED. ) ;
#18010 = B_SPLINE_CURVE_WITH_KNOTS ( 'NONE', 3,
 ( #16380, #5258, #24635, #43719 ),
 .UNSPECIFIED., .F., .F.,
 ( 4, 4 ),
 ( 6.023332361526389438E-07, 0.0004818377974856800200 ),
 .UNSPECIFIED. ) ;
#18011 = DIRECTION ( 'NONE',  ( -3.469446951953613696E-16, 0.000000000000000000, -1.000000000000000000 ) ) ;
#18012 = LINE ( 'NONE', #33776, #36165 ) ;
#18013 = EDGE_LOOP ( 'NONE', ( #35320, #50864, #3704, #5927 ) ) ;
#18014 = DIRECTION ( 'NONE',  ( 1.000000000000000000, 0.000000000000000000, 0.000000000000000000 ) ) ;
#18015 = CARTESIAN_POINT ( 'NONE',  ( -1.909347346926324906, 3.346456692913386100, -0.7874015748031470974 ) ) ;
#18016 = AXIS2_PLACEMENT_3D ( 'NONE', #3202, #18951, #26941 ) ;
#18017 = CARTESIAN_POINT ( 'NONE',  ( 3.927031490892378253E-16, 0.000000000000000000, 1.692913385826762873 ) ) ;
#18018 = DIRECTION ( 'NONE',  ( 0.000000000000000000, 0.000000000000000000, -1.000000000000000000 ) ) ;
#18019 = VECTOR ( 'NONE', #5034, 39.37007874015748143 ) ;
#18020 = CIRCLE ( 'NONE', #12269, 2.106299212598425008 ) ;
#18021 = ORIENTED_EDGE ( 'NONE', *, *, #30878, .T. ) ;
#18022 = CARTESIAN_POINT ( 'NONE',  ( -1.712496953225537633, 3.346456692913386100, 1.325184350462985883 ) ) ;
#18023 = CARTESIAN_POINT ( 'NONE',  ( -0.8182917201112819283, 3.346456692913386100, -0.4724409448818886470 ) ) ;
#18024 = EDGE_LOOP ( 'NONE', ( #29486, #14787, #11260, #9128 ) ) ;
#18025 = CARTESIAN_POINT ( 'NONE',  ( -0.8182917201112819283, 0.000000000000000000, 2.047244094488179567 ) ) ;
#18026 = CARTESIAN_POINT ( 'NONE',  ( 0.000000000000000000, 3.267716535433071279, -1.889763779527552812 ) ) ;
#18027 = VECTOR ( 'NONE', #22892, 39.37007874015748143 ) ;
#18028 = ORIENTED_EDGE ( 'NONE', *, *, #48936, .T. ) ;
#18029 = CARTESIAN_POINT ( 'NONE',  ( 1.909347346926324684, 3.346456692913386100, -0.4724409448818889246 ) ) ;
#18030 = VECTOR ( 'NONE', #21844, 39.37007874015748143 ) ;
#18031 = EDGE_LOOP ( 'NONE', ( #18939, #47139, #17437, #32135 ) ) ;
#18032 = CARTESIAN_POINT ( 'NONE',  ( -1.363819533518803473, 3.267716535433071279, -1.417322834645664109 ) ) ;
#18033 = CARTESIAN_POINT ( 'NONE',  ( -2.101347671104863313, 1.674245022174266406, -0.5300970854448181502 ) ) ;
#18034 = DIRECTION ( 'NONE',  ( -1.000000000000000000, 0.000000000000000000, -0.000000000000000000 ) ) ;
#18035 = AXIS2_PLACEMENT_3D ( 'NONE', #50769, #3336, #30964 ) ;
#18036 = CARTESIAN_POINT ( 'NONE',  ( -1.216138243788243756, 1.692421698714137834, 2.131422395811148895 ) ) ;
#18037 = CARTESIAN_POINT ( 'NONE',  ( 1.962403044652552442, 1.049866565067837820, -0.4983838811554699988 ) ) ;
#18038 = ORIENTED_EDGE ( 'NONE', *, *, #9881, .T. ) ;
#18039 = LINE ( 'NONE', #49483, #2612 ) ;
#18040 = EDGE_CURVE ( 'NONE', #35466, #50600, #29014, .T. ) ;
#18041 = ORIENTED_EDGE ( 'NONE', *, *, #10175, .F. ) ;
#18042 = VERTEX_POINT ( 'NONE', #19983 ) ;
#18043 = EDGE_CURVE ( 'NONE', #37363, #9867, #45749, .T. ) ;
#18044 = CARTESIAN_POINT ( 'NONE',  ( 1.083598637574781920, 1.736150426126270130, 2.747180975113346246 ) ) ;
#18045 = ORIENTED_EDGE ( 'NONE', *, *, #13200, .F. ) ;
#18046 = CARTESIAN_POINT ( 'NONE',  ( 1.091055626815042645, 0.000000000000000000, 1.259842519685033357 ) ) ;
#18047 = DIRECTION ( 'NONE',  ( -1.000000000000000000, 0.000000000000000000, 1.734723475976806848E-16 ) ) ;
#18048 = EDGE_CURVE ( 'NONE', #26872, #46130, #18553, .T. ) ;
#18049 = VERTEX_POINT ( 'NONE', #28502 ) ;
#18050 = EDGE_CURVE ( 'NONE', #24025, #8409, #17155, .T. ) ;
#18051 = DIRECTION ( 'NONE',  ( -0.000000000000000000, 0.000000000000000000, 1.000000000000000000 ) ) ;
#18052 = VECTOR ( 'NONE', #44565, 39.37007874015748143 ) ;
#18053 = DIRECTION ( 'NONE',  ( 1.734723475976806848E-16, -0.000000000000000000, 1.000000000000000000 ) ) ;
#18054 = ADVANCED_FACE ( 'NONE', ( #638 ), #5272, .F. ) ;
#18055 = CARTESIAN_POINT ( 'NONE',  ( 0.1450934409768589450, 1.205361022782829114E-17, 2.161127057262026252 ) ) ;
#18056 = ORIENTED_EDGE ( 'NONE', *, *, #31810, .T. ) ;
#18057 = ORIENTED_EDGE ( 'NONE', *, *, #12638, .F. ) ;
#18058 = CARTESIAN_POINT ( 'NONE',  ( 0.1526763070133267952, 1.611922144458495687, -2.245379599360889600 ) ) ;
#18059 = FACE_BOUND ( 'NONE', #47165, .T. ) ;
#18060 = ORIENTED_EDGE ( 'NONE', *, *, #21245, .T. ) ;
#18061 = VECTOR ( 'NONE', #42676, 39.37007874015748143 ) ;
#18062 = CONICAL_SURFACE ( 'NONE', #42805, 3.483074324928249421, 1.244861948955335196 ) ;
#18063 = DIRECTION ( 'NONE',  ( -8.032339854997315857E-17, 1.000000000000000000, -1.007223559679407077E-16 ) ) ;
#18064 = EDGE_CURVE ( 'NONE', #38331, #43301, #16127, .T. ) ;
#18065 = DIRECTION ( 'NONE',  ( 1.000000000000000000, 0.000000000000000000, 0.000000000000000000 ) ) ;
#18066 = ORIENTED_EDGE ( 'NONE', *, *, #34152, .T. ) ;
#18067 = EDGE_LOOP ( 'NONE', ( #34061, #19807, #38442, #19568 ) ) ;
#18068 = AXIS2_PLACEMENT_3D ( 'NONE', #24803, #33331, #9056 ) ;
#18069 = DIRECTION ( 'NONE',  ( 7.105427357601001859E-15, 0.000000000000000000, 1.000000000000000000 ) ) ;
#18070 = CARTESIAN_POINT ( 'NONE',  ( 1.015142113812069313, 3.346456692913386100, -1.102362204724405714 ) ) ;
#18071 = EDGE_CURVE ( 'NONE', #27247, #6147, #36775, .T. ) ;
#18072 = ORIENTED_EDGE ( 'NONE', *, *, #24860, .T. ) ;
#18073 = ORIENTED_EDGE ( 'NONE', *, *, #46326, .F. ) ;
#18074 = ORIENTED_EDGE ( 'NONE', *, *, #40138, .F. ) ;
#18075 = FACE_OUTER_BOUND ( 'NONE', #5712, .T. ) ;
#18076 = CARTESIAN_POINT ( 'NONE',  ( -2.734482843737247038, 1.572033689214636709, -1.115254632218712016 ) ) ;
#18077 = CARTESIAN_POINT ( 'NONE',  ( 0.000000000000000000, 7.874015748031496287, 0.000000000000000000 ) ) ;
#18078 = DIRECTION ( 'NONE',  ( 0.000000000000000000, 0.000000000000000000, 1.000000000000000000 ) ) ;
#18079 = ORIENTED_EDGE ( 'NONE', *, *, #21728, .F. ) ;
#18080 = ORIENTED_EDGE ( 'NONE', *, *, #34386, .T. ) ;
#18081 = FACE_OUTER_BOUND ( 'NONE', #726, .T. ) ;
#18082 = DIRECTION ( 'NONE',  ( -0.000000000000000000, 1.000000000000000000, -0.000000000000000000 ) ) ;
#18083 = CARTESIAN_POINT ( 'NONE',  ( -1.439733046521776583, 0.000000000000000000, 1.574803149606291530 ) ) ;
#18084 = EDGE_CURVE ( 'NONE', #19616, #46654, #12506, .T. ) ;
#18085 = CARTESIAN_POINT ( 'NONE',  ( 0.2719150483610129343, 1.617565011433980793, -2.472216738435130789 ) ) ;
#18086 = CARTESIAN_POINT ( 'NONE',  ( 1.983515723912132822, 0.6859011407150841233, 1.589814936510557386 ) ) ;
#18087 = CARTESIAN_POINT ( 'NONE',  ( 0.000000000000000000, 5.905511811023623991, 0.000000000000000000 ) ) ;
#18088 = AXIS2_PLACEMENT_3D ( 'NONE', #5469, #24837, #20961 ) ;
#18089 = DIRECTION ( 'NONE',  ( -1.000000000000000000, -0.000000000000000000, -0.000000000000000000 ) ) ;
#18090 = VERTEX_POINT ( 'NONE', #20513 ) ;
#18091 = CARTESIAN_POINT ( 'NONE',  ( -1.733853452330418987, 0.0001488292986583184614, 0.1852043564780690432 ) ) ;
#18092 = CARTESIAN_POINT ( 'NONE',  ( 1.363819533518803251, 3.267716535433071279, 0.4724409448818871482 ) ) ;
#18093 = VERTEX_POINT ( 'NONE', #32917 ) ;
#18094 = ORIENTED_EDGE ( 'NONE', *, *, #9436, .T. ) ;
#18095 = AXIS2_PLACEMENT_3D ( 'NONE', #26133, #10128, #18134 ) ;
#18096 = CARTESIAN_POINT ( 'NONE',  ( 2.592238343552378144, 1.756184615076457289, 0.8940144833510662581 ) ) ;
#18097 = ORIENTED_EDGE ( 'NONE', *, *, #11110, .T. ) ;
#18098 = AXIS2_PLACEMENT_3D ( 'NONE', #11993, #3997, #47060 ) ;
#18099 = EDGE_CURVE ( 'NONE', #8249, #37948, #5019, .T. ) ;
#18100 = ORIENTED_EDGE ( 'NONE', *, *, #36119, .T. ) ;
#18101 = CARTESIAN_POINT ( 'NONE',  ( 0.000000000000000000, 3.267716535433071279, -1.732283464566922726 ) ) ;
#18102 = ORIENTED_EDGE ( 'NONE', *, *, #35142, .F. ) ;
#18103 = EDGE_CURVE ( 'NONE', #4317, #183, #20761, .T. ) ;
#18104 = LINE ( 'NONE', #10856, #19394 ) ;
#18105 = LINE ( 'NONE', #10613, #42056 ) ;
#18106 = ADVANCED_FACE ( 'NONE', ( #48347 ), #16902, .F. ) ;
#18107 = EDGE_CURVE ( 'NONE', #9230, #20129, #24365, .T. ) ;
#18108 = ORIENTED_EDGE ( 'NONE', *, *, #18350, .T. ) ;
#18109 = ORIENTED_EDGE ( 'NONE', *, *, #40000, .F. ) ;
#18110 = DIRECTION ( 'NONE',  ( -0.000000000000000000, 1.000000000000000000, -0.000000000000000000 ) ) ;
#18111 = ORIENTED_EDGE ( 'NONE', *, *, #49241, .T. ) ;
#18112 = ORIENTED_EDGE ( 'NONE', *, *, #24402, .F. ) ;
#18113 = CARTESIAN_POINT ( 'NONE',  ( -2.695799277629577162, 1.677241212940233872, -1.205759334241492509 ) ) ;
#18114 = FACE_OUTER_BOUND ( 'NONE', #13307, .T. ) ;
#18115 = PLANE ( 'NONE',  #28476 ) ;
#18116 = ORIENTED_EDGE ( 'NONE', *, *, #34442, .T. ) ;
#18117 = DIRECTION ( 'NONE',  ( 0.000000000000000000, 1.000000000000000000, 0.000000000000000000 ) ) ;
#18118 = EDGE_CURVE ( 'NONE', #7052, #32688, #2105, .T. ) ;
#18119 = DIRECTION ( 'NONE',  ( 0.01601477604151182663, -0.9998717552508123996, 0.000000000000000000 ) ) ;
#18120 = VECTOR ( 'NONE', #34316, 39.37007874015748143 ) ;
#18121 = LINE ( 'NONE', #49318, #36890 ) ;
#18122 = ORIENTED_EDGE ( 'NONE', *, *, #18220, .T. ) ;
#18123 = DIRECTION ( 'NONE',  ( -0.01601477604151182663, 0.9998717552508123996, -0.000000000000000000 ) ) ;
#18124 = CARTESIAN_POINT ( 'NONE',  ( 1.001850874905584654E-35, 5.905511811023623991, -2.165354330708661568 ) ) ;
#18125 = DIRECTION ( 'NONE',  ( 1.000000000000000000, 0.000000000000000000, -3.469446951953613696E-16 ) ) ;
#18126 = EDGE_CURVE ( 'NONE', #2091, #40341, #48600, .T. ) ;
#18127 = EDGE_LOOP ( 'NONE', ( #24839, #25265, #42234, #3605 ) ) ;
#18128 = ORIENTED_EDGE ( 'NONE', *, *, #47329, .T. ) ;
#18129 = ADVANCED_BREP_SHAPE_REPRESENTATION ( '', ( #6895, #26741 ), #3635 ) ;
#18130 = VECTOR ( 'NONE', #36680, 39.37007874015748143 ) ;
#18131 = LINE ( 'NONE', #41121, #6045 ) ;
#18132 = EDGE_CURVE ( 'NONE', #44656, #34116, #35897, .T. ) ;
#18133 = DIRECTION ( 'NONE',  ( -0.000000000000000000, 1.000000000000000000, -0.000000000000000000 ) ) ;
#18134 = DIRECTION ( 'NONE',  ( 0.000000000000000000, 0.000000000000000000, 1.000000000000000000 ) ) ;
#18135 = VERTEX_POINT ( 'NONE', #25914 ) ;
#18136 = ORIENTED_EDGE ( 'NONE', *, *, #31435, .F. ) ;
#18137 = CARTESIAN_POINT ( 'NONE',  ( 1.747029694980739789, -1.511962954662943480E-16, 1.330264415365524533 ) ) ;
#18138 = CONICAL_SURFACE ( 'NONE', #33821, 2.244934639244524632, 1.554780866114618743 ) ;
#18139 = B_SPLINE_CURVE_WITH_KNOTS ( 'NONE', 3,
 ( #13889, #41762, #45603, #6651 ),
 .UNSPECIFIED., .F., .F.,
 ( 4, 4 ),
 ( 2.033027968835072235E-07, 0.01757837248110587572 ),
 .UNSPECIFIED. ) ;
#18140 = EDGE_LOOP ( 'NONE', ( #2134, #44690, #43338, #42243 ) ) ;
#18141 = DIRECTION ( 'NONE',  ( -0.000000000000000000, 1.000000000000000000, -0.000000000000000000 ) ) ;
#18142 = ADVANCED_FACE ( 'NONE', ( #37292 ), #41663, .F. ) ;
#18143 = DIRECTION ( 'NONE',  ( 1.042246309067994810E-16, 1.000000000000000000, 7.572362681945316160E-17 ) ) ;
#18144 = DIRECTION ( 'NONE',  ( -1.000000000000000000, 0.000000000000000000, 1.734723475976806848E-16 ) ) ;
#18145 = CARTESIAN_POINT ( 'NONE',  ( 0.000000000000000000, 1.574803149606302854, 0.000000000000000000 ) ) ;
#18146 = DIRECTION ( 'NONE',  ( -0.9510565162951544194, -3.583074652439903135E-17, 0.3090169943749447312 ) ) ;
#18147 = ORIENTED_EDGE ( 'NONE', *, *, #17215, .T. ) ;
#18148 = CARTESIAN_POINT ( 'NONE',  ( -1.536664496436148184E-16, 0.000000000000000000, 0.4330708661417287386 ) ) ;
#18149 = CARTESIAN_POINT ( 'NONE',  ( 0.2727639067037604947, 3.267716535433071279, -0.4724409448818886470 ) ) ;
#18150 = EDGE_CURVE ( 'NONE', #37382, #12364, #37801, .T. ) ;
#18151 = CARTESIAN_POINT ( 'NONE',  ( -0.5455278134075208785, 0.000000000000000000, 1.574803149606291974 ) ) ;
#18152 = EDGE_CURVE ( 'NONE', #8911, #11424, #13792, .T. ) ;
#18153 = EDGE_LOOP ( 'NONE', ( #37516, #34000, #15262, #26696 ) ) ;
#18154 = PLANE ( 'NONE',  #31475 ) ;
#18155 = CARTESIAN_POINT ( 'NONE',  ( -0.2727639067037602727, 3.346456692913386100, 1.850393700787392293 ) ) ;
#18156 = CARTESIAN_POINT ( 'NONE',  ( -1.478009596860490715, 1.585803725363800210, 1.616919955472289727 ) ) ;
#18157 = EDGE_LOOP ( 'NONE', ( #30499, #42068, #15194, #5132 ) ) ;
#18158 = DIRECTION ( 'NONE',  ( 0.01601477604151182663, -0.9998717552508123996, 0.000000000000000000 ) ) ;
#18159 = ORIENTED_EDGE ( 'NONE', *, *, #43319, .F. ) ;
#18160 = DIRECTION ( 'NONE',  ( 0.000000000000000000, 0.000000000000000000, -1.000000000000000000 ) ) ;
#18161 = CARTESIAN_POINT ( 'NONE',  ( 0.01639384210327993543, 1.514242943312319012, 2.952755905511811108 ) ) ;
#18162 = VERTEX_POINT ( 'NONE', #17663 ) ;
#18163 = CARTESIAN_POINT ( 'NONE',  ( 0.07982360342473591996, 1.709180471932028711, 0.000000000000000000 ) ) ;
#18164 = ADVANCED_FACE ( 'NONE', ( #34179 ), #13687, .T. ) ;
#18165 = AXIS2_PLACEMENT_3D ( 'NONE', #6460, #36939, #9307 ) ;
#18166 = LINE ( 'NONE', #21528, #42451 ) ;
#18167 = DIRECTION ( 'NONE',  ( 1.000000000000000000, 0.000000000000000000, 0.000000000000000000 ) ) ;
#18168 = DIRECTION ( 'NONE',  ( -0.9998717552508121775, -0.01601477604151182316, 0.000000000000000000 ) ) ;
#18169 = VECTOR ( 'NONE', #10705, 39.37007874015748854 ) ;
#18170 = EDGE_CURVE ( 'NONE', #15256, #24477, #25400, .T. ) ;
#18171 = ORIENTED_EDGE ( 'NONE', *, *, #47007, .F. ) ;
#18172 = ORIENTED_EDGE ( 'NONE', *, *, #8211, .F. ) ;
#18173 = CARTESIAN_POINT ( 'NONE',  ( 2.099568260077707027, 6.692913385826772199, -0.5296909464895783737 ) ) ;
#18174 = DIRECTION ( 'NONE',  ( -3.986037398843765983E-20, -1.000000000000000000, -1.160734090543304660E-16 ) ) ;
#18175 = EDGE_LOOP ( 'NONE', ( #14552, #27874, #25518, #31874 ) ) ;
#18176 = CARTESIAN_POINT ( 'NONE',  ( 0.000000000000000000, 3.267716535433071279, 0.9055118110236167750 ) ) ;
#18177 = LINE ( 'NONE', #10431, #25212 ) ;
#18178 = CONICAL_SURFACE ( 'NONE', #4160, 3.033577403570480779, 1.554780866114618743 ) ;
#18179 = CARTESIAN_POINT ( 'NONE',  ( 1.062992125984251413, 0.5905511811023621549, -6.146657985744589776E-17 ) ) ;
#18180 = ORIENTED_EDGE ( 'NONE', *, *, #43294, .T. ) ;
#18181 = ORIENTED_EDGE ( 'NONE', *, *, #38373, .F. ) ;
#18182 = PLANE ( 'NONE',  #49297 ) ;
#18183 = CARTESIAN_POINT ( 'NONE',  ( -0.3486774197067339376, 3.346456692913386100, -1.574803149606293529 ) ) ;
#18184 = CARTESIAN_POINT ( 'NONE',  ( 2.164823134740036625, 5.905511811023623991, -0.04796011690015061085 ) ) ;
#18185 = ORIENTED_EDGE ( 'NONE', *, *, #24776, .F. ) ;
#18186 = DIRECTION ( 'NONE',  ( -0.000000000000000000, 1.000000000000000000, -0.000000000000000000 ) ) ;
#18187 = CARTESIAN_POINT ( 'NONE',  ( 0.000000000000000000, 3.346456692913386100, 0.000000000000000000 ) ) ;
#18188 = ORIENTED_EDGE ( 'NONE', *, *, #20201, .T. ) ;
#18189 = DIRECTION ( 'NONE',  ( 1.000000000000000000, 0.000000000000000000, 0.000000000000000000 ) ) ;
#18190 = EDGE_LOOP ( 'NONE', ( #20022, #19965, #45725, #31707 ) ) ;
#18191 = EDGE_LOOP ( 'NONE', ( #17204, #17230, #17922, #45592 ) ) ;
#18192 = CARTESIAN_POINT ( 'NONE',  ( 1.363819533518803251, 0.000000000000000000, 1.417322834645662777 ) ) ;
#18193 = DIRECTION ( 'NONE',  ( -3.469446951953613696E-16, 0.000000000000000000, -1.000000000000000000 ) ) ;
#18194 = CARTESIAN_POINT ( 'NONE',  ( -1.679154924913551783, 0.000000000000000000, 0.4938453199301923724 ) ) ;
#18196 = ORIENTED_EDGE ( 'NONE', *, *, #30228, .F. ) ;
#18195 = EDGE_CURVE ( 'NONE', #37703, #48160, #44412, .T. ) ;
#18197 = DIRECTION ( 'NONE',  ( -0.000000000000000000, 1.000000000000000000, -0.000000000000000000 ) ) ;
#18198 = DIRECTION ( 'NONE',  ( 1.734723475976806848E-16, -0.000000000000000000, 1.000000000000000000 ) ) ;
#18199 = EDGE_LOOP ( 'NONE', ( #12558, #6958, #26034, #12425 ) ) ;
#18200 = VERTEX_POINT ( 'NONE', #21281 ) ;
#18201 = LINE ( 'NONE', #33962, #33552 ) ;
#18202 = EDGE_CURVE ( 'NONE', #48375, #47259, #14288, .T. ) ;
#18203 = CARTESIAN_POINT ( 'NONE',  ( -1.891439052599157122, 1.677607092856729709, 1.073712343777111222 ) ) ;
#18204 = VECTOR ( 'NONE', #34771, 39.37007874015748143 ) ;
#18205 = AXIS2_PLACEMENT_3D ( 'NONE', #27536, #24451, #19281 ) ;
#18206 = EDGE_CURVE ( 'NONE', #2602, #47863, #5530, .T. ) ;
#18207 = EDGE_CURVE ( 'NONE', #31796, #36931, #18420, .T. ) ;
#18208 = PLANE ( 'NONE',  #35478 ) ;
#18209 = CARTESIAN_POINT ( 'NONE',  ( -0.07591351300297277671, 0.000000000000000000, 1.102362204724404160 ) ) ;
#18210 = DIRECTION ( 'NONE',  ( 0.000000000000000000, -1.000000000000000000, 0.000000000000000000 ) ) ;
#18211 = ORIENTED_EDGE ( 'NONE', *, *, #2786, .F. ) ;
#18212 = DIRECTION ( 'NONE',  ( 0.000000000000000000, 1.000000000000000000, 0.000000000000000000 ) ) ;
#18213 = CIRCLE ( 'NONE', #25615, 2.244934639244525076 ) ;
#18214 = LINE ( 'NONE', #42203, #28127 ) ;
#18215 = VERTEX_POINT ( 'NONE', #41163 ) ;
#18216 = PLANE ( 'NONE',  #12452 ) ;
#18217 = LINE ( 'NONE', #44804, #9650 ) ;
#18218 = EDGE_LOOP ( 'NONE', ( #28436, #50893, #19166, #29855 ) ) ;
#18219 = CARTESIAN_POINT ( 'NONE',  ( -0.5455278134075214336, 3.346456692913386100, 0.3149606299212577287 ) ) ;
#18220 = EDGE_CURVE ( 'NONE', #47654, #183, #37035, .T. ) ;
#18221 = DIRECTION ( 'NONE',  ( 0.000000000000000000, 0.000000000000000000, -1.000000000000000000 ) ) ;
#18222 = CARTESIAN_POINT ( 'NONE',  ( -0.07591351300297273508, 3.267716535433071279, 2.633779063002547569E-17 ) ) ;
#18223 = ORIENTED_EDGE ( 'NONE', *, *, #32230, .T. ) ;
#18224 = DIRECTION ( 'NONE',  ( -0.9989930665413151445, 0.000000000000000000, 0.04486483035050446017 ) ) ;
#18225 = VERTEX_POINT ( 'NONE', #45759 ) ;
#18226 = FACE_BOUND ( 'NONE', #5976, .T. ) ;
#18227 = LINE ( 'NONE', #22359, #31693 ) ;
#18228 = EDGE_CURVE ( 'NONE', #45076, #3510, #29617, .T. ) ;
#18229 = PLANE ( 'NONE',  #3723 ) ;
#18230 = LINE ( 'NONE', #22610, #5385 ) ;
#18231 = EDGE_CURVE ( 'NONE', #49634, #46386, #21792, .T. ) ;
#18232 = EDGE_LOOP ( 'NONE', ( #50695, #8971, #33091, #48334 ) ) ;
#18233 = ORIENTED_EDGE ( 'NONE', *, *, #24027, .F. ) ;
#18234 = ADVANCED_FACE ( 'NONE', ( #29787 ), #33426, .F. ) ;
#18235 = CARTESIAN_POINT ( 'NONE',  ( 1.363819533518803029, 3.346456692913386100, -1.417322834645665219 ) ) ;
#18236 = CARTESIAN_POINT ( 'NONE',  ( 0.8182917201112817063, 3.346456692913386100, -2.047244094488181343 ) ) ;
#18237 = ORIENTED_EDGE ( 'NONE', *, *, #22125, .F. ) ;
#18238 = VECTOR ( 'NONE', #36688, 39.37007874015748143 ) ;
#18239 = CARTESIAN_POINT ( 'NONE',  ( -0.9914495361339011881, 1.536537968533926657, 2.781765111341808705 ) ) ;
#18240 = AXIS2_PLACEMENT_3D ( 'NONE', #22243, #45700, #10369 ) ;
#18241 = ORIENTED_EDGE ( 'NONE', *, *, #34924, .F. ) ;
#18242 = DIRECTION ( 'NONE',  ( -0.000000000000000000, 1.000000000000000000, -0.000000000000000000 ) ) ;
#18243 = CARTESIAN_POINT ( 'NONE',  ( 0.1450934409768597499, 5.905511811023623991, 2.161127057262026696 ) ) ;
#18244 = ORIENTED_EDGE ( 'NONE', *, *, #33959, .T. ) ;
#18245 = DIRECTION ( 'NONE',  ( -1.000000000000000000, -0.000000000000000000, -0.000000000000000000 ) ) ;
#18246 = VERTEX_POINT ( 'NONE', #37548 ) ;
#18247 = VECTOR ( 'NONE', #3120, 39.37007874015748143 ) ;
#18248 = EDGE_LOOP ( 'NONE', ( #8340, #5114, #48159, #20290 ) ) ;
#18249 = VECTOR ( 'NONE', #1961, 39.37007874015748143 ) ;
#18250 = EDGE_LOOP ( 'NONE', ( #42312, #35729, #21420, #11172 ) ) ;
#18251 = ORIENTED_EDGE ( 'NONE', *, *, #47172, .F. ) ;
#18252 = LINE ( 'NONE', #25238, #10425 ) ;
#18253 = ORIENTED_EDGE ( 'NONE', *, *, #19501, .F. ) ;
#18254 = DIRECTION ( 'NONE',  ( 0.000000000000000000, 0.7660444431189770143, 0.6427876096865403621 ) ) ;
#18255 = CARTESIAN_POINT ( 'NONE',  ( -0.2727639067037608278, 3.267716535433071279, 4.731699523581614055E-17 ) ) ;
#18256 = ADVANCED_FACE ( 'NONE', ( #33168 ), #48850, .T. ) ;
#18257 = ADVANCED_FACE ( 'NONE', ( #45251 ), #2165, .F. ) ;
#18258 = CARTESIAN_POINT ( 'NONE',  ( 1.833433833923351353, 0.000000000000000000, 1.377952755905504256 ) ) ;
#18259 = ADVANCED_FACE ( 'NONE', ( #6798 ), #46999, .F. ) ;
#18260 = CARTESIAN_POINT ( 'NONE',  ( 1.560669927219590747, 3.346456692913386100, 1.417322834645662777 ) ) ;
#18261 = PLANE ( 'NONE',  #8854 ) ;
#18262 = ORIENTED_EDGE ( 'NONE', *, *, #13507, .T. ) ;
#18263 = DIRECTION ( 'NONE',  ( -5.207613805427244364E-18, -1.000000000000000000, -1.159565308550900415E-16 ) ) ;
#18264 = CARTESIAN_POINT ( 'NONE',  ( 0.2727639067037604392, 3.346456692913386100, -0.03937007874015908959 ) ) ;
#18265 = LINE ( 'NONE', #2775, #16960 ) ;
#18266 = DIRECTION ( 'NONE',  ( -0.000000000000000000, 1.000000000000000000, -0.000000000000000000 ) ) ;
#18267 = VECTOR ( 'NONE', #25001, 39.37007874015748143 ) ;
#18268 = EDGE_CURVE ( 'NONE', #26586, #5952, #35934, .T. ) ;
#18269 = ORIENTED_EDGE ( 'NONE', *, *, #18118, .T. ) ;
#18270 = VECTOR ( 'NONE', #47085, 39.37007874015748143 ) ;
#18271 = PLANE ( 'NONE',  #35569 ) ;
#18272 = DIRECTION ( 'NONE',  ( 0.000000000000000000, 0.000000000000000000, 1.000000000000000000 ) ) ;
#18273 = ORIENTED_EDGE ( 'NONE', *, *, #10476, .T. ) ;
#18274 = CARTESIAN_POINT ( 'NONE',  ( -2.947574761915765063, 1.673315526576397261, -0.1816379373805333819 ) ) ;
#18275 = DIRECTION ( 'NONE',  ( 1.000000000000000000, -0.000000000000000000, 0.000000000000000000 ) ) ;
#18276 = AXIS2_PLACEMENT_3D ( 'NONE', #36017, #43226, #35500 ) ;
#18277 = ORIENTED_EDGE ( 'NONE', *, *, #22716, .F. ) ;
#18278 = VECTOR ( 'NONE', #37692, 39.37007874015748143 ) ;
#18279 = B_SPLINE_CURVE_WITH_KNOTS ( 'NONE', 3,
 ( #49309, #29729, #37995, #45446 ),
 .UNSPECIFIED., .F., .F.,
 ( 4, 4 ),
 ( 6.133893191261082042E-07, 0.001146920647357106129 ),
 .UNSPECIFIED. ) ;
#18280 = EDGE_CURVE ( 'NONE', #29782, #20718, #27415, .T. ) ;
#18281 = ORIENTED_EDGE ( 'NONE', *, *, #22824, .F. ) ;
#18282 = DIRECTION ( 'NONE',  ( -3.469446951953613696E-16, 0.000000000000000000, -1.000000000000000000 ) ) ;
#18283 = CARTESIAN_POINT ( 'NONE',  ( 0.9794755770252103755, 0.5070346321433210068, -5.663730925371873532E-17 ) ) ;
#18284 = VECTOR ( 'NONE', #23596, 39.37007874015748143 ) ;
#18285 = CARTESIAN_POINT ( 'NONE',  ( 1.387661672111481836, 0.000000000000000000, -1.663104731517921930 ) ) ;
#18286 = EDGE_CURVE ( 'NONE', #7103, #25998, #11179, .T. ) ;
#18287 = LINE ( 'NONE', #21653, #33371 ) ;
#18288 = PLANE ( 'NONE',  #27737 ) ;
#18289 = VERTEX_POINT ( 'NONE', #31559 ) ;
#18290 = EDGE_CURVE ( 'NONE', #8765, #39693, #7308, .T. ) ;
#18291 = PLANE ( 'NONE',  #10026 ) ;
#18292 = ORIENTED_EDGE ( 'NONE', *, *, #19547, .T. ) ;
#18293 = ORIENTED_EDGE ( 'NONE', *, *, #10105, .T. ) ;
#18294 = CARTESIAN_POINT ( 'NONE',  ( -2.182111253630085290, 3.346456692913386100, 0.7480314960629874665 ) ) ;
#18295 = EDGE_CURVE ( 'NONE', #28575, #7183, #3177, .T. ) ;
#18296 = VERTEX_POINT ( 'NONE', #23544 ) ;
#18297 = CARTESIAN_POINT ( 'NONE',  ( -0.8069532150559458605, 0.000000000000000000, -2.010061882867143268 ) ) ;
#18298 = CARTESIAN_POINT ( 'NONE',  ( -0.6214413264104945434, 3.346456692913386100, -1.102362204724405492 ) ) ;
#18299 = EDGE_CURVE ( 'NONE', #10637, #12169, #38800, .T. ) ;
#18300 = VERTEX_POINT ( 'NONE', #10924 ) ;
#18301 = CARTESIAN_POINT ( 'NONE',  ( -0.7874015748031498729, 0.000000000000000000, -1.138269997360109921E-16 ) ) ;
#18302 = CARTESIAN_POINT ( 'NONE',  ( 0.000000000000000000, 0.000000000000000000, -1.968503937007874072 ) ) ;
#18303 = CARTESIAN_POINT ( 'NONE',  ( 0.9914495361338625523, 1.734714548371065312, 2.781765111341823360 ) ) ;
#18304 = EDGE_LOOP ( 'NONE', ( #38406, #12341, #23945, #20917 ) ) ;
#18305 = ORIENTED_EDGE ( 'NONE', *, *, #17746, .F. ) ;
#18306 = PLANE ( 'NONE',  #32325 ) ;
#18307 = FACE_BOUND ( 'NONE', #42762, .T. ) ;
#18308 = ORIENTED_EDGE ( 'NONE', *, *, #41419, .T. ) ;
#18309 = VECTOR ( 'NONE', #20714, 39.37007874015748143 ) ;
#18310 = DIRECTION ( 'NONE',  ( 1.000000000000000000, 0.000000000000000000, 0.000000000000000000 ) ) ;
#18311 = DIRECTION ( 'NONE',  ( -3.469446951953613696E-16, 0.000000000000000000, -1.000000000000000000 ) ) ;
#18312 = ORIENTED_EDGE ( 'NONE', *, *, #23286, .T. ) ;
#18313 = ORIENTED_EDGE ( 'NONE', *, *, #13900, .T. ) ;
#18314 = CARTESIAN_POINT ( 'NONE',  ( -0.2727639067037607723, 0.000000000000000000, 0.1574803149606283648 ) ) ;
#18315 = VECTOR ( 'NONE', #14684, 39.37007874015748143 ) ;
#18316 = LINE ( 'NONE', #2826, #50901 ) ;
#18317 = ORIENTED_EDGE ( 'NONE', *, *, #49296, .F. ) ;
#18318 = ORIENTED_EDGE ( 'NONE', *, *, #45585, .T. ) ;
#18319 = VECTOR ( 'NONE', #33702, 39.37007874015748143 ) ;
#18320 = VERTEX_POINT ( 'NONE', #15302 ) ;
#18321 = LINE ( 'NONE', #49007, #48265 ) ;
#18322 = B_SPLINE_CURVE_WITH_KNOTS ( 'NONE', 3,
 ( #18751, #22876, #11003, #3762 ),
 .UNSPECIFIED., .F., .F.,
 ( 4, 4 ),
 ( 0.0003396899135061814587, 0.002839874597594404127 ),
 .UNSPECIFIED. ) ;
#18323 = AXIS2_PLACEMENT_3D ( 'NONE', #29194, #48776, #17586 ) ;
#18324 = DIRECTION ( 'NONE',  ( 1.734723475976806848E-16, -0.000000000000000000, 1.000000000000000000 ) ) ;
#18325 = CARTESIAN_POINT ( 'NONE',  ( -2.672362179832771467, 1.673511163758323539, 0.3123340015432766736 ) ) ;
#18326 = DIRECTION ( 'NONE',  ( 1.734723475976806848E-16, -0.000000000000000000, 1.000000000000000000 ) ) ;
#18327 = ORIENTED_EDGE ( 'NONE', *, *, #8048, .F. ) ;
#18328 = VERTEX_POINT ( 'NONE', #15558 ) ;
#18329 = EDGE_CURVE ( 'NONE', #22912, #17453, #49085, .T. ) ;
#18330 = CARTESIAN_POINT ( 'NONE',  ( -0.2727639067037607723, 3.346456692913386100, -0.1574803149606301411 ) ) ;
#18331 = DIRECTION ( 'NONE',  ( -0.000000000000000000, 1.000000000000000000, -0.000000000000000000 ) ) ;
#18332 = EDGE_CURVE ( 'NONE', #47632, #42820, #22800, .T. ) ;
#18333 = FACE_OUTER_BOUND ( 'NONE', #42241, .T. ) ;
#18334 = CARTESIAN_POINT ( 'NONE',  ( 2.134236802639954522, 0.000000000000000000, -2.040539317874581204 ) ) ;
#18335 = ADVANCED_FACE ( 'NONE', ( #50117 ), #4609, .T. ) ;
#18336 = FACE_OUTER_BOUND ( 'NONE', #3701, .T. ) ;
#18337 = DIRECTION ( 'NONE',  ( 0.000000000000000000, 1.160734090543304660E-16, -1.000000000000000000 ) ) ;
#18338 = CARTESIAN_POINT ( 'NONE',  ( 0.8182917201112817063, 3.346456692913386100, -1.929133858267711110 ) ) ;
#18339 = ORIENTED_EDGE ( 'NONE', *, *, #22832, .T. ) ;
#18340 = CARTESIAN_POINT ( 'NONE',  ( -1.220415235146723454, 0.5160455853568216567, -1.535490276664301046 ) ) ;
#18341 = CARTESIAN_POINT ( 'NONE',  ( 2.106197740627112402, 3.267716535433071279, 0.7874015748031456541 ) ) ;
#18342 = ORIENTED_EDGE ( 'NONE', *, *, #441, .F. ) ;
#18343 = ORIENTED_EDGE ( 'NONE', *, *, #33563, .T. ) ;
#18344 = VECTOR ( 'NONE', #48238, 39.37007874015748143 ) ;
#18345 = CARTESIAN_POINT ( 'NONE',  ( 1.695772546416037363, 1.647224322255602891, -2.417756147381349141 ) ) ;
#18346 = EDGE_CURVE ( 'NONE', #7396, #18861, #14803, .T. ) ;
#18347 = ORIENTED_EDGE ( 'NONE', *, *, #2189, .T. ) ;
#18348 = VECTOR ( 'NONE', #43235, 39.37007874015748143 ) ;
#18349 = EDGE_CURVE ( 'NONE', #7558, #40640, #18675, .T. ) ;
#18350 = EDGE_CURVE ( 'NONE', #49658, #22538, #30548, .T. ) ;
#18351 = ORIENTED_EDGE ( 'NONE', *, *, #12773, .T. ) ;
#18352 = DIRECTION ( 'NONE',  ( 1.734723475976806848E-16, -0.000000000000000000, 1.000000000000000000 ) ) ;
#18353 = VECTOR ( 'NONE', #46138, 39.37007874015748143 ) ;
#18354 = ORIENTED_EDGE ( 'NONE', *, *, #6234, .T. ) ;
#18355 = VECTOR ( 'NONE', #50579, 39.37007874015748143 ) ;
#18356 = VECTOR ( 'NONE', #9142, 39.37007874015748143 ) ;
#18357 = DIRECTION ( 'NONE',  ( -0.000000000000000000, 1.000000000000000000, -0.000000000000000000 ) ) ;
#18358 = CARTESIAN_POINT ( 'NONE',  ( 0.000000000000000000, 3.346456692913386100, 0.000000000000000000 ) ) ;
#18359 = ORIENTED_EDGE ( 'NONE', *, *, #6520, .F. ) ;
#18360 = B_SPLINE_CURVE_WITH_KNOTS ( 'NONE', 3,
 ( #5265, #17148, #31885, #12767 ),
 .UNSPECIFIED., .F., .F.,
 ( 4, 4 ),
 ( 5.466635587719015859E-05, 0.002554690799234834650 ),
 .UNSPECIFIED. ) ;
#18361 = ORIENTED_EDGE ( 'NONE', *, *, #9388, .T. ) ;
#18362 = LINE ( 'NONE', #14489, #30433 ) ;
#18363 = VERTEX_POINT ( 'NONE', #19668 ) ;
#18364 = ORIENTED_EDGE ( 'NONE', *, *, #35021, .F. ) ;
#18365 = CARTESIAN_POINT ( 'NONE',  ( 0.000000000000000000, 3.267716535433071279, -0.3543307086614173040 ) ) ;
#18366 = CARTESIAN_POINT ( 'NONE',  ( -0.6214413264104945434, 0.000000000000000000, -1.299212598425193210 ) ) ;
#18367 = PLANE ( 'NONE',  #5895 ) ;
#18368 = CARTESIAN_POINT ( 'NONE',  ( -0.07591351300297333182, 3.346456692913386100, 0.4724409448818869817 ) ) ;
#18369 = ORIENTED_EDGE ( 'NONE', *, *, #23046, .T. ) ;
#18370 = DIRECTION ( 'NONE',  ( -1.000000000000000000, -0.000000000000000000, -0.000000000000000000 ) ) ;
#18371 = CARTESIAN_POINT ( 'NONE',  ( 0.1968503937007873017, 3.267716535433071279, -0.9448818897637765168 ) ) ;
#18372 = CARTESIAN_POINT ( 'NONE',  ( 1.287906020515829919, 3.346456692913386100, -1.889763779527552368 ) ) ;
#18373 = VERTEX_POINT ( 'NONE', #7806 ) ;
#18374 = CARTESIAN_POINT ( 'NONE',  ( 1.636583440222563857, 0.000000000000000000, -0.5118110236220471121 ) ) ;
#18375 = CARTESIAN_POINT ( 'NONE',  ( -1.363819533518803473, 3.346456692913386100, -1.614173228346451605 ) ) ;
#18376 = EDGE_LOOP ( 'NONE', ( #8467, #16177, #47948, #49696 ) ) ;
#18377 = ORIENTED_EDGE ( 'NONE', *, *, #30158, .F. ) ;
#18378 =( NAMED_UNIT ( * ) PLANE_ANGLE_UNIT ( ) SI_UNIT ( $, .RADIAN. ) );
#18379 = CARTESIAN_POINT ( 'NONE',  ( 0.8182917201112817063, 3.267716535433071279, -1.614173228346451605 ) ) ;
#18380 = LINE ( 'NONE', #15267, #12120 ) ;
#18381 = FACE_OUTER_BOUND ( 'NONE', #20063, .T. ) ;
#18382 = ORIENTED_EDGE ( 'NONE', *, *, #5990, .F. ) ;
#18383 = ORIENTED_EDGE ( 'NONE', *, *, #36304, .T. ) ;
#18384 = AXIS2_PLACEMENT_3D ( 'NONE', #45454, #29484, #2116 ) ;
#18385 = EDGE_CURVE ( 'NONE', #26820, #42568, #50607, .T. ) ;
#18386 = LINE ( 'NONE', #41198, #41981 ) ;
#18387 = ADVANCED_FACE ( 'NONE', ( #27162 ), #39299, .F. ) ;
#18388 = CARTESIAN_POINT ( 'NONE',  ( -0.4369915662458470074, 0.02092044581182531462, -1.768387524372482034 ) ) ;
#18389 = EDGE_LOOP ( 'NONE', ( #40990, #26095, #1579, #47021, #10880 ) ) ;
#18390 = LINE ( 'NONE', #34150, #43060 ) ;
#18391 = CARTESIAN_POINT ( 'NONE',  ( 1.670330979180827180, 3.346456692913386100, 1.377952755905504256 ) ) ;
#18392 = EDGE_CURVE ( 'NONE', #27908, #10859, #22542, .T. ) ;
#18393 = VECTOR ( 'NONE', #30198, 39.37007874015748854 ) ;
#18394 = VECTOR ( 'NONE', #40495, 39.37007874015748143 ) ;
#18395 = EDGE_CURVE ( 'NONE', #22312, #47699, #37677, .T. ) ;
#18396 = EDGE_CURVE ( 'NONE', #33096, #10269, #15051, .T. ) ;
#18397 = DIRECTION ( 'NONE',  ( 1.000000000000000000, 0.000000000000000000, 0.000000000000000000 ) ) ;
#18398 = CARTESIAN_POINT ( 'NONE',  ( -1.712496953225537188, 3.346456692913386100, 0.9055118110236167750 ) ) ;
#18399 = DIRECTION ( 'NONE',  ( -0.9998717552508122886, -0.01601477604151182316, 0.000000000000000000 ) ) ;
#18400 = CIRCLE ( 'NONE', #47198, 1.743387098533651480 ) ;
#18401 = ORIENTED_EDGE ( 'NONE', *, *, #33761, .F. ) ;
#18402 = LINE ( 'NONE', #42642, #23395 ) ;
#18403 = LINE ( 'NONE', #26396, #21929 ) ;
#18404 = FACE_OUTER_BOUND ( 'NONE', #8917, .T. ) ;
#18405 = ORIENTED_EDGE ( 'NONE', *, *, #35719, .F. ) ;
#18406 = DIRECTION ( 'NONE',  ( 1.000000000000000000, 0.000000000000000000, 0.000000000000000000 ) ) ;
#18407 = CARTESIAN_POINT ( 'NONE',  ( -1.962403044864191592, 1.049866565877817681, -0.4983838812038057786 ) ) ;
#18408 = ADVANCED_FACE ( 'NONE', ( #47512 ), #20692, .F. ) ;
#18409 = DIRECTION ( 'NONE',  ( 0.000000000000000000, 0.000000000000000000, -1.000000000000000000 ) ) ;
#18410 = VERTEX_POINT ( 'NONE', #49240 ) ;
#18411 = CARTESIAN_POINT ( 'NONE',  ( -0.07591351300297283222, 3.267716535433071279, 2.633779063002550959E-17 ) ) ;
#18412 = EDGE_CURVE ( 'NONE', #48423, #29935, #44184, .T. ) ;
#18413 = ORIENTED_EDGE ( 'NONE', *, *, #23808, .T. ) ;
#18414 = LINE ( 'NONE', #38046, #20440 ) ;
#18415 = B_SPLINE_CURVE_WITH_KNOTS ( 'NONE', 3,
 ( #18962, #34716, #11222, #47044 ),
 .UNSPECIFIED., .F., .F.,
 ( 4, 4 ),
 ( 0.001721583058954078652, 0.004221656532247743121 ),
 .UNSPECIFIED. ) ;
#18416 = ORIENTED_EDGE ( 'NONE', *, *, #25204, .T. ) ;
#18417 = DIRECTION ( 'NONE',  ( -0.01601477604151182663, 0.9998717552508123996, -0.000000000000000000 ) ) ;
#18418 = DIRECTION ( 'NONE',  ( 0.3930250316539147803, -1.160734090543304660E-16, 0.9195277725514544587 ) ) ;
#18419 = DIRECTION ( 'NONE',  ( 0.000000000000000000, 0.000000000000000000, -1.000000000000000000 ) ) ;
#18420 = LINE ( 'NONE', #49860, #35121 ) ;
#18421 = EDGE_CURVE ( 'NONE', #15390, #12933, #32078, .T. ) ;
#18422 = AXIS2_PLACEMENT_3D ( 'NONE', #28710, #49317, #17863 ) ;
#18423 = VERTEX_POINT ( 'NONE', #16061 ) ;
#18424 = ORIENTED_EDGE ( 'NONE', *, *, #44416, .T. ) ;
#18425 = CARTESIAN_POINT ( 'NONE',  ( -1.025452293874513199, 0.4349011127721510994, -1.051609096396380671 ) ) ;
#18426 = CARTESIAN_POINT ( 'NONE',  ( -0.07591351300297363713, 3.346456692913386100, -2.164023224473873963 ) ) ;
#18427 = ORIENTED_EDGE ( 'NONE', *, *, #42782, .F. ) ;
#18428 = VECTOR ( 'NONE', #44740, 39.37007874015748143 ) ;
#18429 = CARTESIAN_POINT ( 'NONE',  ( 2.122091976112992828, 0.000000000000000000, 0.4338754535133130252 ) ) ;
#18430 = DIRECTION ( 'NONE',  ( 0.000000000000000000, -1.000000000000000000, 0.000000000000000000 ) ) ;
#18431 = LINE ( 'NONE', #29797, #14572 ) ;
#18432 = ADVANCED_FACE ( 'NONE', ( #47768 ), #31821, .F. ) ;
#18433 = VECTOR ( 'NONE', #46913, 39.37007874015748143 ) ;
#18434 = VECTOR ( 'NONE', #27642, 39.37007874015748143 ) ;
#18435 = ORIENTED_EDGE ( 'NONE', *, *, #38998, .F. ) ;
#18436 = ORIENTED_EDGE ( 'NONE', *, *, #23738, .T. ) ;
#18437 = CARTESIAN_POINT ( 'NONE',  ( 0.000000000000000000, 3.267716535433071279, 1.062992125984246083 ) ) ;
#18438 = FACE_OUTER_BOUND ( 'NONE', #47762, .T. ) ;
#18439 = DIRECTION ( 'NONE',  ( 0.000000000000000000, 0.000000000000000000, -1.000000000000000000 ) ) ;
#18440 = ORIENTED_EDGE ( 'NONE', *, *, #23852, .F. ) ;
#18441 = FACE_OUTER_BOUND ( 'NONE', #16385, .T. ) ;
#18442 = FACE_BOUND ( 'NONE', #34039, .T. ) ;
#18443 = VECTOR ( 'NONE', #2148, 39.37007874015748143 ) ;
#18444 = ORIENTED_EDGE ( 'NONE', *, *, #22011, .T. ) ;
#18445 = B_SPLINE_CURVE_WITH_KNOTS ( 'NONE', 3,
 ( #8232, #24239, #35603, #47429 ),
 .UNSPECIFIED., .F., .F.,
 ( 4, 4 ),
 ( 2.051444086415969096E-07, 0.002500220145220648053 ),
 .UNSPECIFIED. ) ;
#18446 = CARTESIAN_POINT ( 'NONE',  ( -1.636583440222564301, 3.346456692913386100, -0.9448818897637762948 ) ) ;
#18447 = ORIENTED_EDGE ( 'NONE', *, *, #22337, .F. ) ;
#18448 = ORIENTED_EDGE ( 'NONE', *, *, #45465, .T. ) ;
#18449 = DIRECTION ( 'NONE',  ( -0.9998717552508121775, -0.01601477604151182663, 0.000000000000000000 ) ) ;
#18450 = CARTESIAN_POINT ( 'NONE',  ( 0.000000000000000000, 3.267716535433071279, 0.000000000000000000 ) ) ;
#18451 = CARTESIAN_POINT ( 'NONE',  ( -2.182111253630085290, 0.000000000000000000, -0.1968503937007880511 ) ) ;
#18452 = CARTESIAN_POINT ( 'NONE',  ( -2.394539146693994702, 1.677872874819792859, 1.232670874412874040 ) ) ;
#18453 = UNCERTAINTY_MEASURE_WITH_UNIT (LENGTH_MEASURE( 1.000000000000000082E-05 ), #2633, 'distance_accuracy_value', 'NONE');
#18454 = DIRECTION ( 'NONE',  ( -0.01601477604151182663, 0.9998717552508123996, -0.000000000000000000 ) ) ;
#18455 = ORIENTED_EDGE ( 'NONE', *, *, #37357, .F. ) ;
#18456 = ORIENTED_EDGE ( 'NONE', *, *, #33378, .F. ) ;
#18457 = DIRECTION ( 'NONE',  ( -3.469446951953613696E-16, 0.000000000000000000, -1.000000000000000000 ) ) ;
#18458 = LINE ( 'NONE', #7094, #26743 ) ;
#18459 = EDGE_CURVE ( 'NONE', #12011, #2745, #43924, .T. ) ;
#18460 = CARTESIAN_POINT ( 'NONE',  ( -1.363819533518803473, 3.346456692913386100, 1.732283464566920950 ) ) ;
#18461 = EDGE_CURVE ( 'NONE', #19150, #31480, #4911, .T. ) ;
#18462 = AXIS2_PLACEMENT_3D ( 'NONE', #20007, #35773, #44016 ) ;
#18463 = CARTESIAN_POINT ( 'NONE',  ( -1.772999178993743152, 2.755905511811027164, -1.009977129983215649 ) ) ;
#18464 = CARTESIAN_POINT ( 'NONE',  ( 1.560669927219590303, 0.000000000000000000, -1.299212598425193210 ) ) ;
#18465 = ORIENTED_EDGE ( 'NONE', *, *, #36522, .F. ) ;
#18466 = VECTOR ( 'NONE', #48757, 39.37007874015748143 ) ;
#18467 = PLANE ( 'NONE',  #15955 ) ;
#18468 = AXIS2_PLACEMENT_3D ( 'NONE', #7986, #229, #31743 ) ;
#18469 = DIRECTION ( 'NONE',  ( 1.000000000000000000, 0.000000000000000000, 0.000000000000000000 ) ) ;
#18470 = AXIS2_PLACEMENT_3D ( 'NONE', #28749, #5775, #16893 ) ;
#18471 = AXIS2_PLACEMENT_3D ( 'NONE', #4679, #44667, #20418 ) ;
#18472 = ORIENTED_EDGE ( 'NONE', *, *, #25611, .T. ) ;
#18473 = CARTESIAN_POINT ( 'NONE',  ( 0.5455278134075216556, 3.267716535433071279, 1.062992125984246083 ) ) ;
#18474 = DIRECTION ( 'NONE',  ( 1.000000000000000000, -0.000000000000000000, 0.000000000000000000 ) ) ;
#18475 = ORIENTED_EDGE ( 'NONE', *, *, #13328, .F. ) ;
#18476 = DIRECTION ( 'NONE',  ( -0.000000000000000000, 1.000000000000000000, -0.000000000000000000 ) ) ;
#18477 = CARTESIAN_POINT ( 'NONE',  ( 2.378961647330872786, 3.267716535433071279, -8.253681236146643855E-16 ) ) ;
#18478 = CARTESIAN_POINT ( 'NONE',  ( 0.000000000000000000, 3.267716535433071279, 1.574803149606291974 ) ) ;
#18479 = VECTOR ( 'NONE', #46430, 39.37007874015748143 ) ;
#18480 = ORIENTED_EDGE ( 'NONE', *, *, #2245, .T. ) ;
#18481 = DIRECTION ( 'NONE',  ( -0.000000000000000000, 1.000000000000000000, -0.000000000000000000 ) ) ;
#18482 = ORIENTED_EDGE ( 'NONE', *, *, #37087, .T. ) ;
#18483 = FACE_BOUND ( 'NONE', #18680, .T. ) ;
#18484 = FACE_OUTER_BOUND ( 'NONE', #5921, .T. ) ;
#18485 = LINE ( 'NONE', #34240, #15251 ) ;
#18486 = CARTESIAN_POINT ( 'NONE',  ( -0.3486774197067334380, 3.346456692913386100, 1.889763779527550369 ) ) ;
#18487 = EDGE_CURVE ( 'NONE', #36908, #31407, #28434, .T. ) ;
#18488 = VERTEX_POINT ( 'NONE', #27928 ) ;
#18489 = VERTEX_POINT ( 'NONE', #48984 ) ;
#18490 = FACE_OUTER_BOUND ( 'NONE', #37320, .T. ) ;
#18491 = CARTESIAN_POINT ( 'NONE',  ( -2.168245791271168343, 1.685466330048090322, -2.004968704497279930 ) ) ;
#18492 = LINE ( 'NONE', #40781, #4600 ) ;
#18493 = FACE_OUTER_BOUND ( 'NONE', #2828, .T. ) ;
#18494 = EDGE_CURVE ( 'NONE', #46941, #6476, #33555, .T. ) ;
#18495 = DIRECTION ( 'NONE',  ( -0.01601477604151182663, 0.9998717552508123996, -0.000000000000000000 ) ) ;
#18496 = VERTEX_POINT ( 'NONE', #40336 ) ;
#18497 = B_SPLINE_CURVE_WITH_KNOTS ( 'NONE', 3,
 ( #20635, #40778, #4891, #5400 ),
 .UNSPECIFIED., .F., .F.,
 ( 4, 4 ),
 ( 0.1211775127643062444, 0.1625894504277921315 ),
 .UNSPECIFIED. ) ;
#18498 = VERTEX_POINT ( 'NONE', #29408 ) ;
#18499 = PLANE ( 'NONE',  #29067 ) ;
#18500 = EDGE_CURVE ( 'NONE', #4594, #40457, #45131, .T. ) ;
#18501 = CARTESIAN_POINT ( 'NONE',  ( 2.491402175429654253, 1.758084086496218612, -1.585592796919505609 ) ) ;
#18502 = VECTOR ( 'NONE', #31658, 39.37007874015748143 ) ;
#18503 = ORIENTED_EDGE ( 'NONE', *, *, #40980, .F. ) ;
#18504 = ADVANCED_FACE ( 'NONE', ( #27667 ), #41289, .F. ) ;
#18505 = CARTESIAN_POINT ( 'NONE',  ( 4.268512490100411402E-16, 3.346456692913386100, 0.9448818897637749625 ) ) ;
#18506 = VECTOR ( 'NONE', #25624, 39.37007874015748143 ) ;
#18507 = ORIENTED_EDGE ( 'NONE', *, *, #41769, .F. ) ;
#18508 = ORIENTED_EDGE ( 'NONE', *, *, #20237, .F. ) ;
#18509 = VECTOR ( 'NONE', #37411, 39.37007874015748143 ) ;
#18510 = EDGE_CURVE ( 'NONE', #58, #7441, #5911, .T. ) ;
#18511 = AXIS2_PLACEMENT_3D ( 'NONE', #42775, #46872, #15421 ) ;
#18512 = ORIENTED_EDGE ( 'NONE', *, *, #49302, .F. ) ;
#18513 = ORIENTED_EDGE ( 'NONE', *, *, #20126, .T. ) ;
#18514 = LINE ( 'NONE', #34763, #22806 ) ;
#18515 = VECTOR ( 'NONE', #35865, 39.37007874015748143 ) ;
#18516 = ORIENTED_EDGE ( 'NONE', *, *, #34545, .F. ) ;
#18517 = LINE ( 'NONE', #18004, #12231 ) ;
#18518 = CARTESIAN_POINT ( 'NONE',  ( 1.033334490728470723, 1.724452693827607908, -2.032317711754626277 ) ) ;
#18519 = ADVANCED_FACE ( 'NONE', ( #35944 ), #8312, .F. ) ;
#18520 = CARTESIAN_POINT ( 'NONE',  ( 1.810607833951273227, 0.05691986357332023266, -0.7203715021987137090 ) ) ;
#18521 = EDGE_CURVE ( 'NONE', #12259, #3361, #41697, .T. ) ;
#18522 = CARTESIAN_POINT ( 'NONE',  ( 2.576863348864710801, 1.660943078747768364, 1.442554885838449819 ) ) ;
#18523 = DIRECTION ( 'NONE',  ( 1.000000000000000000, 0.000000000000000000, -3.469446951953613696E-16 ) ) ;
#18524 = EDGE_CURVE ( 'NONE', #19657, #39052, #28180, .T. ) ;
#18525 = ORIENTED_EDGE ( 'NONE', *, *, #27106, .T. ) ;
#18526 = DIRECTION ( 'NONE',  ( -0.000000000000000000, 1.000000000000000000, -0.000000000000000000 ) ) ;
#18527 = PLANE ( 'NONE',  #50501 ) ;
#18528 = FACE_OUTER_BOUND ( 'NONE', #41909, .T. ) ;
#18529 = CARTESIAN_POINT ( 'NONE',  ( -1.693234526714950228, 0.000000000000000000, -0.4369479234249735167 ) ) ;
#18530 = VERTEX_POINT ( 'NONE', #32333 ) ;
#18531 = CARTESIAN_POINT ( 'NONE',  ( 0.000000000000000000, 3.267716535433071279, -0.5118110236220467790 ) ) ;
#18532 = LINE ( 'NONE', #37910, #44239 ) ;
#18533 = VERTEX_POINT ( 'NONE', #26297 ) ;
#18534 = CARTESIAN_POINT ( 'NONE',  ( -0.8942052331142547050, 0.000000000000000000, 0.6299212598425164567 ) ) ;
#18535 = CARTESIAN_POINT ( 'NONE',  ( 1.363819533518803251, 3.267716535433071279, -0.3543307086614178592 ) ) ;
#18536 = ORIENTED_EDGE ( 'NONE', *, *, #11922, .T. ) ;
#18537 = CONICAL_SURFACE ( 'NONE', #5339, 1.850107469027523210, 0.6386652850508578450 ) ;
#18538 = AXIS2_PLACEMENT_3D ( 'NONE', #32053, #28153, #20937 ) ;
#18539 = CARTESIAN_POINT ( 'NONE',  ( 1.956192433058983493, 0.05925166736471587647, -0.03859050128386512513 ) ) ;
#18540 = ORIENTED_EDGE ( 'NONE', *, *, #30443, .T. ) ;
#18541 = CARTESIAN_POINT ( 'NONE',  ( 1.122047244094487972, 0.4724409448818892576, 1.122047244094487750 ) ) ;
#18542 = AXIS2_PLACEMENT_3D ( 'NONE', #17403, #49104, #5528 ) ;
#18543 = DIRECTION ( 'NONE',  ( 1.000000000000000000, 0.000000000000000000, 0.000000000000000000 ) ) ;
#18544 = LINE ( 'NONE', #19034, #28684 ) ;
#18545 = FACE_OUTER_BOUND ( 'NONE', #8460, .T. ) ;
#18546 = CARTESIAN_POINT ( 'NONE',  ( 0.8182917201112819283, 3.346456692913386100, -0.4724409448818889246 ) ) ;
#18547 = VERTEX_POINT ( 'NONE', #2553 ) ;
#18548 = EDGE_CURVE ( 'NONE', #21385, #2753, #25216, .T. ) ;
#18549 = DIRECTION ( 'NONE',  ( -0.000000000000000000, 1.000000000000000000, -0.000000000000000000 ) ) ;
#18550 = VECTOR ( 'NONE', #36417, 39.37007874015748143 ) ;
#18551 = VERTEX_POINT ( 'NONE', #29916 ) ;
#18552 = VERTEX_POINT ( 'NONE', #6933 ) ;
#18553 = B_SPLINE_CURVE_WITH_KNOTS ( 'NONE', 3,
 ( #24385, #40141, #9404, #48093 ),
 .UNSPECIFIED., .F., .F.,
 ( 4, 4 ),
 ( 6.098493025361481195E-07, 0.001073452918374830957 ),
 .UNSPECIFIED. ) ;
#18554 = CARTESIAN_POINT ( 'NONE',  ( -2.952069331832154919, 5.118110236220475784, 1.181102362204724310 ) ) ;
#18555 = EDGE_LOOP ( 'NONE', ( #39896, #14987, #3158, #36061 ) ) ;
#18556 = DIRECTION ( 'NONE',  ( -0.000000000000000000, 1.000000000000000000, -0.000000000000000000 ) ) ;
#18557 = CARTESIAN_POINT ( 'NONE',  ( 0.000000000000000000, 3.267716535433071279, -2.086614173228339641 ) ) ;
#18558 = ORIENTED_EDGE ( 'NONE', *, *, #10806, .F. ) ;
#18559 = CARTESIAN_POINT ( 'NONE',  ( 0.1968503937007872462, 3.346456692913386100, -1.141732283464564013 ) ) ;
#18560 = EDGE_CURVE ( 'NONE', #7137, #7249, #34558, .T. ) ;
#18561 = CARTESIAN_POINT ( 'NONE',  ( 0.07982360342473591996, 1.709180471932028711, 0.000000000000000000 ) ) ;
#18562 = ADVANCED_FACE ( 'NONE', ( #42043 ), #22679, .F. ) ;
#18563 = ADVANCED_FACE ( 'NONE', ( #10296 ), #34054, .F. ) ;
#18564 = PLANE ( 'NONE',  #24722 ) ;
#18565 = ORIENTED_EDGE ( 'NONE', *, *, #21356, .T. ) ;
#18566 = VERTEX_POINT ( 'NONE', #10044 ) ;
#18567 = DIRECTION ( 'NONE',  ( -1.000000000000000000, 0.000000000000000000, 0.000000000000000000 ) ) ;
#18568 = FACE_BOUND ( 'NONE', #16791, .T. ) ;
#18569 = ORIENTED_EDGE ( 'NONE', *, *, #50407, .F. ) ;
#18570 = CARTESIAN_POINT ( 'NONE',  ( -1.363819533518803473, 0.000000000000000000, -1.299212598425192544 ) ) ;
#18571 = LINE ( 'NONE', #47347, #34967 ) ;
#18572 = VERTEX_POINT ( 'NONE', #18298 ) ;
#18573 = VERTEX_POINT ( 'NONE', #38187 ) ;
#18574 = DIRECTION ( 'NONE',  ( 1.734723475976806848E-16, -0.000000000000000000, 1.000000000000000000 ) ) ;
#18575 = CONICAL_SURFACE ( 'NONE', #24312, 2.246510896728926010, 0.01601546068027819014 ) ;
#18576 = LINE ( 'NONE', #34334, #27846 ) ;
#18577 = VECTOR ( 'NONE', #21421, 39.37007874015748143 ) ;
#18578 = VECTOR ( 'NONE', #23461, 39.37007874015748143 ) ;
#18579 = ORIENTED_EDGE ( 'NONE', *, *, #18843, .F. ) ;
#18580 = EDGE_CURVE ( 'NONE', #32558, #26618, #49740, .T. ) ;
#18581 = AXIS2_PLACEMENT_3D ( 'NONE', #14547, #27160, #42903 ) ;
#18582 = ORIENTED_EDGE ( 'NONE', *, *, #28903, .F. ) ;
#18583 = CARTESIAN_POINT ( 'NONE',  ( -0.8942052331142559263, 3.267716535433071279, 3.102397620449225439E-16 ) ) ;
#18584 = CARTESIAN_POINT ( 'NONE',  ( -0.9914495361339011881, 1.536537968533926657, 2.781765111341808705 ) ) ;
#18585 = EDGE_CURVE ( 'NONE', #7499, #22686, #45632, .T. ) ;
#18586 = FACE_OUTER_BOUND ( 'NONE', #43725, .T. ) ;
#18587 = EDGE_CURVE ( 'NONE', #22163, #15713, #2297, .T. ) ;
#18588 = ORIENTED_EDGE ( 'NONE', *, *, #19319, .F. ) ;
#18589 = ORIENTED_EDGE ( 'NONE', *, *, #32727, .T. ) ;
#18590 = VECTOR ( 'NONE', #14867, 39.37007874015748143 ) ;
#18591 = CARTESIAN_POINT ( 'NONE',  ( -0.8942052331142552601, 0.000000000000000000, 2.007874015748021268 ) ) ;
#18592 = CARTESIAN_POINT ( 'NONE',  ( 0.5455278134075212115, 0.000000000000000000, -0.9448818897637765168 ) ) ;
#18593 = ADVANCED_FACE ( 'NONE', ( #30430 ), #45890, .T. ) ;
#18594 = LINE ( 'NONE', #14714, #5193 ) ;
#18595 = CARTESIAN_POINT ( 'NONE',  ( 0.3136974817028393425, 1.625700591256411531, -2.936457595020219635 ) ) ;
#18596 = DIRECTION ( 'NONE',  ( 0.000000000000000000, 0.000000000000000000, 1.000000000000000000 ) ) ;
#18597 = CARTESIAN_POINT ( 'NONE',  ( -1.636583440222563635, 3.267716535433071279, -4.780733988912460139E-16 ) ) ;
#18598 = CARTESIAN_POINT ( 'NONE',  ( -0.8182917201112814842, 3.346456692913386100, 0.7874015748031456541 ) ) ;
#18599 = ORIENTED_EDGE ( 'NONE', *, *, #47124, .T. ) ;
#18600 = CARTESIAN_POINT ( 'NONE',  ( 1.834323595590318989, 5.905511811023623991, 1.151859023884926447 ) ) ;
#18601 = DIRECTION ( 'NONE',  ( -0.000000000000000000, 1.000000000000000000, -0.000000000000000000 ) ) ;
#18602 = EDGE_LOOP ( 'NONE', ( #28156, #43686, #38204, #2864 ) ) ;
#18603 = EDGE_LOOP ( 'NONE', ( #28954, #48350, #28103, #48709 ) ) ;
#18604 = LINE ( 'NONE', #42336, #18428 ) ;
#18605 = PLANE ( 'NONE',  #26194 ) ;
#18606 = ORIENTED_EDGE ( 'NONE', *, *, #45290, .T. ) ;
#18607 = AXIS2_PLACEMENT_3D ( 'NONE', #9896, #8680, #6277 ) ;
#18608 = VECTOR ( 'NONE', #48752, 39.37007874015748143 ) ;
#18609 = ORIENTED_EDGE ( 'NONE', *, *, #2825, .F. ) ;
#18610 = CARTESIAN_POINT ( 'NONE',  ( -1.195183497228115035E-16, 3.267716535433071279, -1.259842519685035134 ) ) ;
#18611 = VECTOR ( 'NONE', #14297, 39.37007874015748143 ) ;
#18612 = ORIENTED_EDGE ( 'NONE', *, *, #462, .T. ) ;
#18613 = CARTESIAN_POINT ( 'NONE',  ( 1.091055626815042423, 3.346456692913386100, -1.771653543307081691 ) ) ;
#18614 = DIRECTION ( 'NONE',  ( -0.000000000000000000, 1.000000000000000000, -0.000000000000000000 ) ) ;
#18615 = EDGE_CURVE ( 'NONE', #42119, #24025, #22931, .T. ) ;
#18616 = AXIS2_PLACEMENT_3D ( 'NONE', #18187, #33445, #10186 ) ;
#18617 = VERTEX_POINT ( 'NONE', #38431 ) ;
#18618 = EDGE_CURVE ( 'NONE', #41248, #20003, #26544, .T. ) ;
#18619 = AXIS2_PLACEMENT_3D ( 'NONE', #1074, #36458, #13664 ) ;
#18620 = DIRECTION ( 'NONE',  ( -3.469446951953613696E-16, 0.000000000000000000, -1.000000000000000000 ) ) ;
#18621 = EDGE_CURVE ( 'NONE', #31414, #32045, #10554, .T. ) ;
#18622 = VERTEX_POINT ( 'NONE', #18807 ) ;
#18623 = ORIENTED_EDGE ( 'NONE', *, *, #25806, .F. ) ;
#18624 = CARTESIAN_POINT ( 'NONE',  ( -0.8942052331142552601, 3.346456692913386100, 2.204724409448808764 ) ) ;
#18625 = DIRECTION ( 'NONE',  ( -0.000000000000000000, 1.000000000000000000, -0.000000000000000000 ) ) ;
#18626 = LINE ( 'NONE', #34376, #40508 ) ;
#18627 = DIRECTION ( 'NONE',  ( 0.000000000000000000, 0.000000000000000000, -1.000000000000000000 ) ) ;
#18628 = EDGE_CURVE ( 'NONE', #7592, #50730, #22429, .T. ) ;
#18629 = ORIENTED_EDGE ( 'NONE', *, *, #31062, .T. ) ;
#18630 = DIRECTION ( 'NONE',  ( 0.000000000000000000, 0.000000000000000000, -1.000000000000000000 ) ) ;
#18631 = CARTESIAN_POINT ( 'NONE',  ( 0.5455278134075216556, 3.346456692913386100, 1.377952755905504256 ) ) ;
#18632 = CARTESIAN_POINT ( 'NONE',  ( 0.8668862056626265300, 0.04180443457634609727, -1.686684286392636789 ) ) ;
#18633 = VERTEX_POINT ( 'NONE', #30678 ) ;
#18634 = DIRECTION ( 'NONE',  ( -0.000000000000000000, -1.000000000000000000, -0.000000000000000000 ) ) ;
#18635 = ORIENTED_EDGE ( 'NONE', *, *, #2947, .F. ) ;
#18636 = ORIENTED_EDGE ( 'NONE', *, *, #43710, .T. ) ;
#18637 = EDGE_CURVE ( 'NONE', #21915, #14529, #3305, .T. ) ;
#18638 = CARTESIAN_POINT ( 'NONE',  ( 0.000000000000000000, 0.000000000000000000, 0.000000000000000000 ) ) ;
#18639 = CARTESIAN_POINT ( 'NONE',  ( 0.4374213808359648237, 1.623899391754041854, 2.686003462684949827 ) ) ;
#18640 = ADVANCED_FACE ( 'NONE', ( #6173 ), #6429, .F. ) ;
#18642 = CARTESIAN_POINT ( 'NONE',  ( 1.930379001715699872, 1.650868500535964012, 2.234429108663295693 ) ) ;
#18641 = VECTOR ( 'NONE', #9637, 39.37007874015748143 ) ;
#18643 = LINE ( 'NONE', #34395, #46107 ) ;
#18644 = ORIENTED_EDGE ( 'NONE', *, *, #8929, .T. ) ;
#18645 = ORIENTED_EDGE ( 'NONE', *, *, #5183, .F. ) ;
#18646 = CONICAL_SURFACE ( 'NONE', #35106, 2.244934639244524632, 1.554780866114618743 ) ;
#18647 = VECTOR ( 'NONE', #21375, 39.37007874015748143 ) ;
#18648 = EDGE_CURVE ( 'NONE', #2383, #50578, #49491, .T. ) ;
#18649 = CARTESIAN_POINT ( 'NONE',  ( 2.113646359261424745, 1.643330668647667858, -0.9569352356128659753 ) ) ;
#18650 = ORIENTED_EDGE ( 'NONE', *, *, #4988, .T. ) ;
#18651 = DIRECTION ( 'NONE',  ( 1.156482317317871478E-16, -0.000000000000000000, 1.000000000000000000 ) ) ;
#18652 = LINE ( 'NONE', #34402, #29249 ) ;
#18653 = AXIS2_PLACEMENT_3D ( 'NONE', #19490, #34999, #3246 ) ;
#18654 = VECTOR ( 'NONE', #11952, 39.37007874015748143 ) ;
#18655 = CARTESIAN_POINT ( 'NONE',  ( 0.2957575371695307376, 0.01082520027161247393, 1.905371342176711114 ) ) ;
#18656 = CARTESIAN_POINT ( 'NONE',  ( 2.651794250122221246E-16, 0.000000000000000000, 2.165354330708661568 ) ) ;
#18657 = CARTESIAN_POINT ( 'NONE',  ( 0.2727639067037604947, 0.000000000000000000, -0.1574803149606298636 ) ) ;
#18658 = VECTOR ( 'NONE', #16138, 39.37007874015748143 ) ;
#18659 = ORIENTED_EDGE ( 'NONE', *, *, #30199, .T. ) ;
#18660 = LINE ( 'NONE', #50340, #33344 ) ;
#18661 = CARTESIAN_POINT ( 'NONE',  ( -1.636583440222564301, 3.267716535433071279, -1.771653543307080581 ) ) ;
#18662 = CARTESIAN_POINT ( 'NONE',  ( 0.000000000000000000, 3.346456692913386100, 0.000000000000000000 ) ) ;
#18663 = EDGE_LOOP ( 'NONE', ( #31526, #2365, #43844, #30128 ) ) ;
#18664 = DIRECTION ( 'NONE',  ( 0.000000000000000000, -1.000000000000000000, 0.000000000000000000 ) ) ;
#18665 = DIRECTION ( 'NONE',  ( -0.000000000000000000, -1.000000000000000000, -0.000000000000000000 ) ) ;
#18666 = CARTESIAN_POINT ( 'NONE',  ( 1.062992125984252079, 0.5905511811023621549, -1.014069264286642014 ) ) ;
#18667 = ORIENTED_EDGE ( 'NONE', *, *, #8952, .F. ) ;
#18668 = CARTESIAN_POINT ( 'NONE',  ( -2.437180031585919782, 1.566133505135788750, -1.667735833703134274 ) ) ;
#18669 = ORIENTED_EDGE ( 'NONE', *, *, #2015, .F. ) ;
#18670 = DIRECTION ( 'NONE',  ( -0.000000000000000000, 1.000000000000000000, -0.000000000000000000 ) ) ;
#18671 = EDGE_LOOP ( 'NONE', ( #3885, #12400, #46218, #12656 ) ) ;
#18672 = LINE ( 'NONE', #25908, #50888 ) ;
#18673 = CARTESIAN_POINT ( 'NONE',  ( -0.3136974817027967100, 1.714375164834789356, -2.936457595020224520 ) ) ;
#18674 = DIRECTION ( 'NONE',  ( -3.986037398843765983E-20, -1.000000000000000000, -1.160734090543304660E-16 ) ) ;
#18675 = LINE ( 'NONE', #31306, #7888 ) ;
#18676 = VECTOR ( 'NONE', #35039, 39.37007874015748143 ) ;
#18677 = ORIENTED_EDGE ( 'NONE', *, *, #6968, .T. ) ;
#18678 = ADVANCED_FACE ( 'NONE', ( #37931 ), #8454, .F. ) ;
#18679 = ORIENTED_EDGE ( 'NONE', *, *, #6739, .F. ) ;
#18680 = EDGE_LOOP ( 'NONE', ( #38747, #44780, #10352, #12910 ) ) ;
#18681 = DIRECTION ( 'NONE',  ( 0.000000000000000000, -1.000000000000000000, 0.000000000000000000 ) ) ;
#18682 = VECTOR ( 'NONE', #5619, 39.37007874015748143 ) ;
#18683 = LINE ( 'NONE', #14555, #43564 ) ;
#18684 = EDGE_CURVE ( 'NONE', #22386, #20489, #27805, .T. ) ;
#18685 = VECTOR ( 'NONE', #47804, 39.37007874015748143 ) ;
#18686 = ORIENTED_EDGE ( 'NONE', *, *, #17244, .F. ) ;
#18687 = CARTESIAN_POINT ( 'NONE',  ( 1.191535142427733174, 0.000000000000000000, -1.668040279728017605 ) ) ;
#18688 = CARTESIAN_POINT ( 'NONE',  ( -1.091055626815042645, 0.000000000000000000, 1.889763779527550147 ) ) ;
#18689 = CARTESIAN_POINT ( 'NONE',  ( 1.363819533518803251, 0.000000000000000000, -0.03937007874015908959 ) ) ;
#18690 = ADVANCED_FACE ( 'NONE', ( #186 ), #50485, .F. ) ;
#18691 = ORIENTED_EDGE ( 'NONE', *, *, #18862, .F. ) ;
#18692 = EDGE_LOOP ( 'NONE', ( #2247, #19850, #17820, #23635 ) ) ;
#18693 = DIRECTION ( 'NONE',  ( 1.734723475976806848E-16, -0.000000000000000000, 1.000000000000000000 ) ) ;
#18694 = CARTESIAN_POINT ( 'NONE',  ( 2.715141060683428531, 0.000000000000000000, -1.160506983230063405 ) ) ;
#18695 = AXIS2_PLACEMENT_3D ( 'NONE', #8667, #47612, #8161 ) ;
#18696 = CARTESIAN_POINT ( 'NONE',  ( -0.3486774197067334935, 3.267716535433071279, 1.377952755905504256 ) ) ;
#18697 = EDGE_CURVE ( 'NONE', #42744, #4851, #512, .T. ) ;
#18698 = ORIENTED_EDGE ( 'NONE', *, *, #42809, .T. ) ;
#18699 = PRESENTATION_STYLE_ASSIGNMENT (( #42178 ) ) ;
#18700 = DIRECTION ( 'NONE',  ( 0.000000000000000000, -0.000000000000000000, 1.000000000000000000 ) ) ;
#18701 = ORIENTED_EDGE ( 'NONE', *, *, #42239, .T. ) ;
#18702 = LINE ( 'NONE', #14061, #42226 ) ;
#18703 = VERTEX_POINT ( 'NONE', #39692 ) ;
#18704 = VERTEX_POINT ( 'NONE', #7436 ) ;
#18705 = CARTESIAN_POINT ( 'NONE',  ( 1.636583440222563857, 3.346456692913386100, 1.259842519685033135 ) ) ;
#18706 = DIRECTION ( 'NONE',  ( -0.04486483035050446017, 0.000000000000000000, -0.9989930665413151445 ) ) ;
#18707 = DIRECTION ( 'NONE',  ( 0.5508969814521065267, 0.000000000000000000, -0.8345732537212999791 ) ) ;
#18708 = EDGE_CURVE ( 'NONE', #29664, #1395, #39949, .T. ) ;
#18709 = CARTESIAN_POINT ( 'NONE',  ( -0.4532322590609024759, 0.000000000000000000, -1.827234353172969561 ) ) ;
#18710 = DIRECTION ( 'NONE',  ( 1.000000000000000000, -0.000000000000000000, 0.000000000000000000 ) ) ;
#18711 = EDGE_LOOP ( 'NONE', ( #21724, #28904, #24726, #9958 ) ) ;
#18712 = APPLICATION_CONTEXT ( 'automotive_design' ) ;
#18713 = ADVANCED_FACE ( 'NONE', ( #43037 ), #15182, .F. ) ;
#18714 = ORIENTED_EDGE ( 'NONE', *, *, #37536, .F. ) ;
#18715 = CARTESIAN_POINT ( 'NONE',  ( 1.091055626815042645, 0.000000000000000000, -8.878505979408855953E-16 ) ) ;
#18716 = CARTESIAN_POINT ( 'NONE',  ( -0.5455278134075208785, 3.346456692913386100, 0.9448818897637749625 ) ) ;
#18717 = VECTOR ( 'NONE', #2659, 39.37007874015748143 ) ;
#18718 = DIRECTION ( 'NONE',  ( -0.6579387259397136978, 0.000000000000000000, 0.7530714660036097463 ) ) ;
#18719 = CARTESIAN_POINT ( 'NONE',  ( 0.1155636338427008941, -0.5222242541845523167, 0.000000000000000000 ) ) ;
#18720 = DIRECTION ( 'NONE',  ( 0.000000000000000000, 0.000000000000000000, 1.000000000000000000 ) ) ;
#18721 = VECTOR ( 'NONE', #37900, 39.37007874015748143 ) ;
#18722 = ORIENTED_EDGE ( 'NONE', *, *, #41371, .T. ) ;
#18723 = CARTESIAN_POINT ( 'NONE',  ( 0.8182917201112819283, 3.346456692913386100, 1.102362204724403938 ) ) ;
#18724 = EDGE_CURVE ( 'NONE', #16641, #25262, #17842, .T. ) ;
#18725 = DIRECTION ( 'NONE',  ( 1.000000000000000000, -0.000000000000000000, 0.000000000000000000 ) ) ;
#18726 = ORIENTED_EDGE ( 'NONE', *, *, #7225, .F. ) ;
#18727 = PLANE ( 'NONE',  #43840 ) ;
#18728 = PLANE ( 'NONE',  #38509 ) ;
#18729 = ORIENTED_EDGE ( 'NONE', *, *, #40017, .T. ) ;
#18730 = CARTESIAN_POINT ( 'NONE',  ( -1.621934931400436541, 0.000000000000000000, -0.6753680165623594522 ) ) ;
#18731 = VECTOR ( 'NONE', #43187, 39.37007874015748143 ) ;
#18732 = CARTESIAN_POINT ( 'NONE',  ( -0.3486774197067339376, 3.346456692913386100, -0.3149606299212593941 ) ) ;
#18733 = DIRECTION ( 'NONE',  ( 1.000000000000000000, -0.000000000000000000, 0.000000000000000000 ) ) ;
#18734 = VERTEX_POINT ( 'NONE', #31957 ) ;
#18735 = CARTESIAN_POINT ( 'NONE',  ( -2.889674983507169337, 1.205361022782829114E-17, -0.6090712660038032356 ) ) ;
#18736 = ORIENTED_EDGE ( 'NONE', *, *, #46265, .T. ) ;
#18737 = FACE_BOUND ( 'NONE', #27934, .T. ) ;
#18738 = CARTESIAN_POINT ( 'NONE',  ( -1.461363083917493588, 1.574803149606302854, 1.597866488315563327 ) ) ;
#18739 = CARTESIAN_POINT ( 'NONE',  ( -0.6214413264104939882, 3.346456692913386100, 1.417322834645662777 ) ) ;
#18740 = ORIENTED_EDGE ( 'NONE', *, *, #5388, .T. ) ;
#18741 = EDGE_LOOP ( 'NONE', ( #10157, #9786, #39623, #39344 ) ) ;
#18742 = CARTESIAN_POINT ( 'NONE',  ( -1.091055626815042645, 3.346456692913386100, 2.007874015748021268 ) ) ;
#18743 = DIRECTION ( 'NONE',  ( 0.000000000000000000, -1.000000000000000000, 0.000000000000000000 ) ) ;
#18744 = FACE_OUTER_BOUND ( 'NONE', #46901, .T. ) ;
#18745 = FACE_OUTER_BOUND ( 'NONE', #45210, .T. ) ;
#18746 = ADVANCED_FACE ( 'NONE', ( #47396 ), #23944, .F. ) ;
#18747 = CARTESIAN_POINT ( 'NONE',  ( -1.195183497228115035E-16, 0.000000000000000000, -1.259842519685035134 ) ) ;
#18748 = EDGE_LOOP ( 'NONE', ( #39819, #2758, #50621, #25625 ) ) ;
#18749 = EDGE_CURVE ( 'NONE', #15665, #13810, #23685, .T. ) ;
#18750 = ORIENTED_EDGE ( 'NONE', *, *, #45173, .F. ) ;
#18751 = CARTESIAN_POINT ( 'NONE',  ( -1.330356682269850044, 1.588168657012911877, -1.747353411991260819 ) ) ;
#18752 = VECTOR ( 'NONE', #35451, 39.37007874015748143 ) ;
#18753 = AXIS2_PLACEMENT_3D ( 'NONE', #34105, #10603, #38731 ) ;
#18754 = EDGE_CURVE ( 'NONE', #2997, #3878, #3800, .T. ) ;
#18755 = CARTESIAN_POINT ( 'NONE',  ( -0.3486774197067340486, 3.267716535433071279, -1.771653543307081025 ) ) ;
#18756 = VECTOR ( 'NONE', #23914, 39.37007874015748143 ) ;
#18757 = ORIENTED_EDGE ( 'NONE', *, *, #24034, .T. ) ;
#18758 = CARTESIAN_POINT ( 'NONE',  ( 3.927031490892378253E-16, 3.346456692913386100, 0.7480314960629874665 ) ) ;
#18759 = EDGE_LOOP ( 'NONE', ( #25921, #24159, #26114, #6655 ) ) ;
#18760 = ORIENTED_EDGE ( 'NONE', *, *, #43343, .T. ) ;
#18761 = EDGE_CURVE ( 'NONE', #20976, #20329, #8201, .T. ) ;
#18762 = ORIENTED_EDGE ( 'NONE', *, *, #18769, .T. ) ;
#18763 = ORIENTED_EDGE ( 'NONE', *, *, #50899, .F. ) ;
#18764 = CARTESIAN_POINT ( 'NONE',  ( -0.5440951526915226433, 1.699187271209207983, -2.156468654116168171 ) ) ;
#18765 = ADVANCED_FACE ( 'NONE', ( #43293 ), #23175, .T. ) ;
#18767 = CARTESIAN_POINT ( 'NONE',  ( -1.985260859929297794, 0.000000000000000000, -0.1968503937007880511 ) ) ;
#18766 = VECTOR ( 'NONE', #16167, 39.37007874015748143 ) ;
#18768 = PLANE ( 'NONE',  #20292 ) ;
#18769 = EDGE_CURVE ( 'NONE', #2318, #9779, #50737, .T. ) ;
#18770 = DIRECTION ( 'NONE',  ( -1.000000000000000000, -0.000000000000000000, -0.000000000000000000 ) ) ;
#18771 = LINE ( 'NONE', #30645, #12935 ) ;
#18772 = CARTESIAN_POINT ( 'NONE',  ( -1.010509689441836390, 0.01173450346422093109, -1.474572740271697047 ) ) ;
#18773 = EDGE_LOOP ( 'NONE', ( #24110, #32220, #14578, #16927 ) ) ;
#18774 = CARTESIAN_POINT ( 'NONE',  ( 0.2727639067037604947, 0.000000000000000000, -0.7874015748031473194 ) ) ;
#18775 = CARTESIAN_POINT ( 'NONE',  ( -2.160407304981126764, 1.574803149606302854, -0.1462862061266896330 ) ) ;
#18776 = CARTESIAN_POINT ( 'NONE',  ( 1.834499544866850851, 1.737284818394516206, 1.400019292979238772 ) ) ;
#18777 = EDGE_CURVE ( 'NONE', #45538, #23634, #11667, .T. ) ;
#18778 = DIRECTION ( 'NONE',  ( -0.9909497617679332571, 0.000000000000000000, -0.1342332658176667304 ) ) ;
#18779 = VERTEX_POINT ( 'NONE', #42793 ) ;
#18780 = CARTESIAN_POINT ( 'NONE',  ( -1.636583440222563635, 3.346456692913386100, 0.7480314960629874665 ) ) ;
#18781 = DIRECTION ( 'NONE',  ( -1.000000000000000000, 0.000000000000000000, 1.734723475976806848E-16 ) ) ;
#18782 = VERTEX_POINT ( 'NONE', #27295 ) ;
#18783 = CARTESIAN_POINT ( 'NONE',  ( 1.295655976102049600E-16, 0.000000000000000000, -4.324626651086886948E-17 ) ) ;
#18784 = VECTOR ( 'NONE', #17401, 39.37007874015748143 ) ;
#18785 = VECTOR ( 'NONE', #28421, 39.37007874015748143 ) ;
#18786 = CARTESIAN_POINT ( 'NONE',  ( 2.947574761915768171, 1.447536563168191126, -0.1816379373804911657 ) ) ;
#18787 = ADVANCED_FACE ( 'NONE', ( #23422 ), #39178, .F. ) ;
#18788 = VECTOR ( 'NONE', #15507, 39.37007874015748143 ) ;
#18789 = PLANE ( 'NONE',  #2657 ) ;
#18790 = ORIENTED_EDGE ( 'NONE', *, *, #22691, .F. ) ;
#18791 = DIRECTION ( 'NONE',  ( 0.9797780297642105785, 0.000000000000000000, 0.2000875118326022883 ) ) ;
#18792 = ADVANCED_FACE ( 'NONE', ( #15681 ), #47135, .F. ) ;
#18793 = LINE ( 'NONE', #21910, #36605 ) ;
#18794 = AXIS2_PLACEMENT_3D ( 'NONE', #7116, #6614, #22358 ) ;
#18795 = CARTESIAN_POINT ( 'NONE',  ( -1.909347346926324462, 0.000000000000000000, 1.102362204724404160 ) ) ;
#18796 = DIRECTION ( 'NONE',  ( -1.000000000000000000, 0.000000000000000000, 1.734723475976806848E-16 ) ) ;
#18797 = LINE ( 'NONE', #21914, #43390 ) ;
#18798 = ORIENTED_EDGE ( 'NONE', *, *, #25701, .T. ) ;
#18799 = CONICAL_SURFACE ( 'NONE', #665, 2.165354330708661568, 0.2617993877991570129 ) ;
#18800 = CARTESIAN_POINT ( 'NONE',  ( 0.1155636338427008941, -0.5222242541845523167, 0.000000000000000000 ) ) ;
#18801 = ORIENTED_EDGE ( 'NONE', *, *, #21356, .F. ) ;
#18802 = ORIENTED_EDGE ( 'NONE', *, *, #27556, .T. ) ;
#18803 = DIRECTION ( 'NONE',  ( -3.469446951953613696E-16, 0.000000000000000000, -1.000000000000000000 ) ) ;
#18804 = ORIENTED_EDGE ( 'NONE', *, *, #8208, .T. ) ;
#18805 = CARTESIAN_POINT ( 'NONE',  ( -1.712496953225537633, 3.346456692913386100, 1.325184350462985883 ) ) ;
#18806 = AXIS2_PLACEMENT_3D ( 'NONE', #19643, #9259, #17013 ) ;
#18807 = CARTESIAN_POINT ( 'NONE',  ( -0.3486774197067339376, 3.267716535433071279, 2.204724409448808764 ) ) ;
#18808 = VERTEX_POINT ( 'NONE', #40468 ) ;
#18809 = EDGE_CURVE ( 'NONE', #4725, #31145, #40982, .T. ) ;
#18810 = CARTESIAN_POINT ( 'NONE',  ( -1.712496953225537188, 0.000000000000000000, 0.1574803149606286423 ) ) ;
#18811 = DIRECTION ( 'NONE',  ( 0.000000000000000000, 0.000000000000000000, -1.000000000000000000 ) ) ;
#18812 = ADVANCED_FACE ( 'NONE', ( #44321 ), #31030, .F. ) ;
#18813 = EDGE_CURVE ( 'NONE', #9339, #31055, #9736, .T. ) ;
#18814 = CARTESIAN_POINT ( 'NONE',  ( 0.1968503937007877735, 0.000000000000000000, 1.692913385826762873 ) ) ;
#18815 = VERTEX_POINT ( 'NONE', #13353 ) ;
#18816 = ORIENTED_EDGE ( 'NONE', *, *, #34919, .T. ) ;
#18817 = LINE ( 'NONE', #34566, #2619 ) ;
#18818 = FACE_BOUND ( 'NONE', #20398, .T. ) ;
#18819 = VERTEX_POINT ( 'NONE', #28834 ) ;
#18820 = CARTESIAN_POINT ( 'NONE',  ( 1.232620761116212105, 1.574803149606302854, -1.780282403660734980 ) ) ;
#18821 = VECTOR ( 'NONE', #30426, 39.37007874015748143 ) ;
#18822 = EDGE_LOOP ( 'NONE', ( #47096, #55, #32226, #17121 ) ) ;
#18823 = ORIENTED_EDGE ( 'NONE', *, *, #40143, .F. ) ;
#18824 = LINE ( 'NONE', #34575, #5957 ) ;
#18825 = CARTESIAN_POINT ( 'NONE',  ( 0.08139965876239094178, 1.610780518492231694, 0.000000000000000000 ) ) ;
#18826 = ORIENTED_EDGE ( 'NONE', *, *, #12441, .T. ) ;
#18827 = VECTOR ( 'NONE', #10951, 39.37007874015748143 ) ;
#18828 = LINE ( 'NONE', #47416, #10545 ) ;
#18829 = EDGE_LOOP ( 'NONE', ( #6678, #19736, #13582, #9217 ) ) ;
#18830 = DIRECTION ( 'NONE',  ( 1.000000000000000000, 0.000000000000000000, -3.469446951953613696E-16 ) ) ;
#18831 = CARTESIAN_POINT ( 'NONE',  ( -2.074049943651441019, 1.574803149606302854, 0.6221544894623937116 ) ) ;
#18832 = VECTOR ( 'NONE', #2097, 39.37007874015748143 ) ;
#18833 = EDGE_CURVE ( 'NONE', #46201, #33355, #29347, .T. ) ;
#18834 = PLANE ( 'NONE',  #1649 ) ;
#18835 = VECTOR ( 'NONE', #13880, 39.37007874015748143 ) ;
#18836 = ORIENTED_EDGE ( 'NONE', *, *, #22347, .F. ) ;
#18837 = ORIENTED_EDGE ( 'NONE', *, *, #4846, .F. ) ;
#18838 = DIRECTION ( 'NONE',  ( 0.8865472742777344983, -0.000000000000000000, 0.4626380123495248964 ) ) ;
#18839 = LINE ( 'NONE', #45666, #22198 ) ;
#18840 = CARTESIAN_POINT ( 'NONE',  ( 1.287906020515829919, 3.346456692913386100, -1.574803149606294417 ) ) ;
#18841 = CIRCLE ( 'NONE', #17228, 2.106299212598425008 ) ;
#18842 = CARTESIAN_POINT ( 'NONE',  ( -1.205290937646080307, -0.2057703422145251981, -2.141165755267305126 ) ) ;
#18843 = EDGE_CURVE ( 'NONE', #30490, #27988, #44568, .T. ) ;
#18844 = CARTESIAN_POINT ( 'NONE',  ( 0.2727639067037609943, 3.267716535433071279, 1.535433070866133898 ) ) ;
#18845 = ADVANCED_FACE ( 'NONE', ( #45075 ), #32987, .F. ) ;
#18846 = DIRECTION ( 'NONE',  ( 0.000000000000000000, 1.000000000000000000, 0.000000000000000000 ) ) ;
#18847 = EDGE_CURVE ( 'NONE', #129, #28656, #44061, .T. ) ;
#18848 = CARTESIAN_POINT ( 'NONE',  ( 1.709950266952970921, 0.000000000000000000, -0.3398067978735070382 ) ) ;
#18849 = ORIENTED_EDGE ( 'NONE', *, *, #1324, .F. ) ;
#18850 = CARTESIAN_POINT ( 'NONE',  ( 0.4696143004045484903, 0.000000000000000000, 2.362204724409437961 ) ) ;
#18851 = CARTESIAN_POINT ( 'NONE',  ( -0.2810367729153296912, 1.520692402626517170, -2.939397112015448066 ) ) ;
#18852 = ORIENTED_EDGE ( 'NONE', *, *, #28685, .F. ) ;
#18853 = VERTEX_POINT ( 'NONE', #708 ) ;
#18854 = DIRECTION ( 'NONE',  ( 1.000000000000000000, 0.000000000000000000, -3.469446951953613696E-16 ) ) ;
#18855 = CARTESIAN_POINT ( 'NONE',  ( 1.181102362204724310, 0.5905511811023621549, -1.181102362204724754 ) ) ;
#18856 = VECTOR ( 'NONE', #4009, 39.37007874015747433 ) ;
#18857 = ORIENTED_EDGE ( 'NONE', *, *, #8840, .T. ) ;
#18858 = ADVANCED_FACE ( 'NONE', ( #24719 ), #25471, .F. ) ;
#18859 = VERTEX_POINT ( 'NONE', #40212 ) ;
#18860 = CARTESIAN_POINT ( 'NONE',  ( -1.387661672111457412, 1.205361022782829114E-17, -1.663104731517942136 ) ) ;
#18861 = VERTEX_POINT ( 'NONE', #29083 ) ;
#18862 = EDGE_CURVE ( 'NONE', #42794, #38226, #36849, .T. ) ;
#18863 = B_SPLINE_CURVE_WITH_KNOTS ( 'NONE', 3,
 ( #19684, #15814, #31574, #11948 ),
 .UNSPECIFIED., .F., .F.,
 ( 4, 4 ),
 ( 2.033027418798480799E-07, 0.01771249989147270082 ),
 .UNSPECIFIED. ) ;
#18864 = CIRCLE ( 'NONE', #27911, 1.850107469027523432 ) ;
#18865 = DIRECTION ( 'NONE',  ( 2.866708903754326305E-17, 1.000000000000000000, 1.255987235303924321E-16 ) ) ;
#18866 = PLANE ( 'NONE',  #47751 ) ;
#18867 = EDGE_CURVE ( 'NONE', #37726, #47811, #44821, .T. ) ;
#18868 = EDGE_CURVE ( 'NONE', #19280, #29009, #16719, .T. ) ;
#18869 = PRESENTATION_LAYER_ASSIGNMENT (  '', '', ( #34540 ) ) ;
#18870 = VERTEX_POINT ( 'NONE', #24460 ) ;
#18871 = CARTESIAN_POINT ( 'NONE',  ( 0.9914495361338626633, 0.000000000000000000, 2.781765111341823360 ) ) ;
#18873 = ORIENTED_EDGE ( 'NONE', *, *, #38599, .T. ) ;
#18872 = EDGE_CURVE ( 'NONE', #22659, #5755, #1469, .T. ) ;
#18874 = ORIENTED_EDGE ( 'NONE', *, *, #51011, .T. ) ;
#18875 = CARTESIAN_POINT ( 'NONE',  ( -1.166969139818015977, 3.267716535433071279, -1.732283464566922726 ) ) ;
#18876 = CARTESIAN_POINT ( 'NONE',  ( -2.182111253630085290, 3.267716535433071279, -6.146657985744592735E-16 ) ) ;
#18877 = DIRECTION ( 'NONE',  ( -0.7484689079293680436, 0.000000000000000000, -0.6631698831091618063 ) ) ;
#18878 = VECTOR ( 'NONE', #13270, 39.37007874015748143 ) ;
#18879 = ORIENTED_EDGE ( 'NONE', *, *, #25687, .T. ) ;
#18880 = PLANE ( 'NONE',  #43501 ) ;
#18881 = DIRECTION ( 'NONE',  ( -0.08963930890344089242, 0.000000000000000000, 0.9959742939952384022 ) ) ;
#18882 = ORIENTED_EDGE ( 'NONE', *, *, #32079, .F. ) ;
#18883 = CARTESIAN_POINT ( 'NONE',  ( 0.000000000000000000, 6.692913385826772199, 0.000000000000000000 ) ) ;
#18884 = VERTEX_POINT ( 'NONE', #8708 ) ;
#18885 = VERTEX_POINT ( 'NONE', #33239 ) ;
#18886 = LINE ( 'NONE', #38760, #11099 ) ;
#18887 = DIRECTION ( 'NONE',  ( 0.000000000000000000, 0.000000000000000000, -1.000000000000000000 ) ) ;
#18888 =( BOUNDED_CURVE ( )  B_SPLINE_CURVE ( 3, ( #40752, #41012, #5378, #36884 ),
 .UNSPECIFIED., .F., .F. ) 
 B_SPLINE_CURVE_WITH_KNOTS ( ( 4, 4 ),
 ( 5.617161475044070151, 5.667964663408525894 ),
 .UNSPECIFIED. ) 
 CURVE ( )  GEOMETRIC_REPRESENTATION_ITEM ( )  RATIONAL_B_SPLINE_CURVE ( ( 1.000000000000000000, 0.9997849312356386076, 0.9997849312356386076, 1.000000000000000000 ) ) 
 REPRESENTATION_ITEM ( '' )  );
#18889 = AXIS2_PLACEMENT_3D ( 'NONE', #2932, #30301, #30046 ) ;
#18890 = DIRECTION ( 'NONE',  ( 1.734723475976806848E-16, -0.000000000000000000, 1.000000000000000000 ) ) ;
#18891 = DIRECTION ( 'NONE',  ( -0.000000000000000000, 1.000000000000000000, -0.000000000000000000 ) ) ;
#18892 = ORIENTED_EDGE ( 'NONE', *, *, #44581, .T. ) ;
#18893 = ORIENTED_EDGE ( 'NONE', *, *, #8400, .F. ) ;
#18894 = SURFACE_SIDE_STYLE ('',( #38274 ) ) ;
#18895 = LINE ( 'NONE', #42378, #36672 ) ;
#18896 = VERTEX_POINT ( 'NONE', #28316 ) ;
#18897 = CARTESIAN_POINT ( 'NONE',  ( 0.2156353639037333347, 0.03137346048107473445, -1.846898229409209558 ) ) ;
#18898 = CARTESIAN_POINT ( 'NONE',  ( 0.4696143004045479352, 3.346456692913386100, -0.1574803149606298636 ) ) ;
#18899 = VECTOR ( 'NONE', #44469, 39.37007874015748143 ) ;
#18900 = EDGE_CURVE ( 'NONE', #9322, #10377, #20839, .T. ) ;
#18901 = AXIS2_PLACEMENT_3D ( 'NONE', #7365, #3489, #34735 ) ;
#18902 = CARTESIAN_POINT ( 'NONE',  ( -0.8942052331142552601, 0.000000000000000000, -0.3149606299212593941 ) ) ;
#18903 = EDGE_CURVE ( 'NONE', #48838, #49994, #13607, .T. ) ;
#18904 = CARTESIAN_POINT ( 'NONE',  ( 2.182111253630085290, 3.346456692913386100, 0.1181102362204698858 ) ) ;
#18905 = DIRECTION ( 'NONE',  ( -0.000000000000000000, 1.000000000000000000, -0.000000000000000000 ) ) ;
#18906 = EDGE_LOOP ( 'NONE', ( #42752, #3437, #5049, #20181, #47201 ) ) ;
#18907 = DIRECTION ( 'NONE',  ( 1.000000000000000000, 0.000000000000000000, 0.000000000000000000 ) ) ;
#18908 = CARTESIAN_POINT ( 'NONE',  ( -1.312442655063644770, 0.006898494447474761912, -1.186737126055851022 ) ) ;
#18909 = ORIENTED_EDGE ( 'NONE', *, *, #25513, .F. ) ;
#18910 = DIRECTION ( 'NONE',  ( -0.000000000000000000, 0.000000000000000000, 1.000000000000000000 ) ) ;
#18911 = DIRECTION ( 'NONE',  ( -3.469446951953613696E-16, 0.000000000000000000, -1.000000000000000000 ) ) ;
#18912 = DIRECTION ( 'NONE',  ( 0.000000000000000000, -1.000000000000000000, 0.000000000000000000 ) ) ;
#18913 = ORIENTED_EDGE ( 'NONE', *, *, #34945, .F. ) ;
#18914 = DIRECTION ( 'NONE',  ( -3.986037398843765983E-20, -1.000000000000000000, -1.160734090543304660E-16 ) ) ;
#18915 = ORIENTED_EDGE ( 'NONE', *, *, #5901, .F. ) ;
#18916 = CARTESIAN_POINT ( 'NONE',  ( -4.268512490100411402E-16, 3.346456692913386100, -2.086614173228339641 ) ) ;
#18918 = EDGE_LOOP ( 'NONE', ( #38171, #50953, #44272, #27010 ) ) ;
#18917 = ADVANCED_FACE ( 'NONE', ( #16458 ), #36335, .F. ) ;
#18919 = CARTESIAN_POINT ( 'NONE',  ( -1.439733046521777249, 3.267716535433071279, 4.995077429881869829E-16 ) ) ;
#18920 = ORIENTED_EDGE ( 'NONE', *, *, #26204, .F. ) ;
#18921 = DIRECTION ( 'NONE',  ( -0.01601477604151182663, 0.9998717552508123996, -0.000000000000000000 ) ) ;
#18922 = ADVANCED_FACE ( 'NONE', ( #34251 ), #10998, .F. ) ;
#18923 = CARTESIAN_POINT ( 'NONE',  ( 1.015142113812069091, 0.000000000000000000, -2.047244094488181343 ) ) ;
#18924 = CARTESIAN_POINT ( 'NONE',  ( -1.195183497228115035E-16, 3.346456692913386100, -0.9448818897637765168 ) ) ;
#18925 = VECTOR ( 'NONE', #4526, 39.37007874015748143 ) ;
#18926 = EDGE_CURVE ( 'NONE', #37379, #38729, #1982, .T. ) ;
#18927 = ORIENTED_EDGE ( 'NONE', *, *, #30003, .F. ) ;
#18928 = ORIENTED_EDGE ( 'NONE', *, *, #15711, .F. ) ;
#18929 = ORIENTED_EDGE ( 'NONE', *, *, #15052, .T. ) ;
#18930 = DIRECTION ( 'NONE',  ( 0.000000000000000000, 0.000000000000000000, 1.000000000000000000 ) ) ;
#18931 = CARTESIAN_POINT ( 'NONE',  ( -1.171400696859933532, 1.590714628027123823, 1.864644694871980590 ) ) ;
#18932 = ADVANCED_FACE ( 'NONE', ( #33496 ), #42229, .F. ) ;
#18933 = VERTEX_POINT ( 'NONE', #18236 ) ;
#18934 = CARTESIAN_POINT ( 'NONE',  ( -1.166969139818015977, 3.346456692913386100, -1.753476375576570323 ) ) ;
#18935 = CARTESIAN_POINT ( 'NONE',  ( 1.560669927219590525, 3.267716535433071279, 0.5905511811023579360 ) ) ;
#18936 = CARTESIAN_POINT ( 'NONE',  ( -0.6214413264104945434, 3.267716535433071279, -1.299212598425193210 ) ) ;
#18937 = CIRCLE ( 'NONE', #25533, 2.106299212598425008 ) ;
#18938 = VERTEX_POINT ( 'NONE', #42485 ) ;
#18939 = ORIENTED_EDGE ( 'NONE', *, *, #40897, .T. ) ;
#18940 = CARTESIAN_POINT ( 'NONE',  ( -1.834323595590334977, 5.905511811023623991, 1.151859023884901356 ) ) ;
#18941 = DIRECTION ( 'NONE',  ( -1.000000000000000000, 0.000000000000000000, 1.734723475976806848E-16 ) ) ;
#18942 = CARTESIAN_POINT ( 'NONE',  ( -1.363819533518803029, 0.000000000000000000, 1.220472440944875281 ) ) ;
#18943 = ORIENTED_EDGE ( 'NONE', *, *, #21625, .F. ) ;
#18944 = DIRECTION ( 'NONE',  ( 1.734723475976806848E-16, 0.000000000000000000, 1.000000000000000000 ) ) ;
#18945 = DIRECTION ( 'NONE',  ( -1.000000000000000000, 0.000000000000000000, -0.000000000000000000 ) ) ;
#18946 = ORIENTED_EDGE ( 'NONE', *, *, #46054, .T. ) ;
#18947 = DIRECTION ( 'NONE',  ( -1.000000000000000000, -0.000000000000000000, -0.000000000000000000 ) ) ;
#18948 = VERTEX_POINT ( 'NONE', #46088 ) ;
#18949 = VERTEX_POINT ( 'NONE', #41988 ) ;
#18950 = VECTOR ( 'NONE', #26354, 39.37007874015748143 ) ;
#18951 = DIRECTION ( 'NONE',  ( -0.000000000000000000, 0.000000000000000000, 1.000000000000000000 ) ) ;
#18952 = LINE ( 'NONE', #46289, #19255 ) ;
#18953 = CARTESIAN_POINT ( 'NONE',  ( 1.461363083917469163, 6.692913385826772199, 1.597866488315585087 ) ) ;
#18954 = DIRECTION ( 'NONE',  ( 0.000000000000000000, 0.000000000000000000, -1.000000000000000000 ) ) ;
#18955 = PLANE ( 'NONE',  #4893 ) ;
#18956 = ORIENTED_EDGE ( 'NONE', *, *, #8032, .F. ) ;
#18957 = VERTEX_POINT ( 'NONE', #46336 ) ;
#18958 = CARTESIAN_POINT ( 'NONE',  ( -0.1227720337126170513, 0.000000000000000000, -1.913115909999223652 ) ) ;
#18959 = CARTESIAN_POINT ( 'NONE',  ( -0.04921259842519706829, 1.707113721008201024, 2.241222193722145484 ) ) ;
#18960 = EDGE_CURVE ( 'NONE', #2592, #22332, #20914, .T. ) ;
#18961 = LINE ( 'NONE', #42453, #41828 ) ;
#18962 = CARTESIAN_POINT ( 'NONE',  ( 2.064489077472676737, 1.642543324816299277, 1.055063358597729595 ) ) ;
#18963 = ORIENTED_EDGE ( 'NONE', *, *, #30796, .T. ) ;
#18964 = ADVANCED_FACE ( 'NONE', ( #26238, #6872 ), #6106, .T. ) ;
#18965 = LINE ( 'NONE', #10720, #39882 ) ;
#18966 = CARTESIAN_POINT ( 'NONE',  ( -2.009899395340762673, 3.346456692913386100, 0.6299212598425164567 ) ) ;
#18967 = EDGE_CURVE ( 'NONE', #49786, #29523, #7923, .T. ) ;
#18968 = VECTOR ( 'NONE', #47163, 39.37007874015748854 ) ;
#18969 = ORIENTED_EDGE ( 'NONE', *, *, #4912, .T. ) ;
#18970 = LINE ( 'NONE', #34227, #47908 ) ;
#18971 = AXIS2_PLACEMENT_3D ( 'NONE', #855, #12989, #4729 ) ;
#18972 = CARTESIAN_POINT ( 'NONE',  ( -0.2727639067037607723, 0.000000000000000000, 0.4724409448818869817 ) ) ;
#18973 = CARTESIAN_POINT ( 'NONE',  ( -1.091055626815042201, 3.346456692913386100, 0.3149606299212580063 ) ) ;
#18974 = DIRECTION ( 'NONE',  ( -1.000000000000000000, 0.000000000000000000, 1.734723475976806848E-16 ) ) ;
#18975 = DIRECTION ( 'NONE',  ( 1.734723475976806848E-16, 0.000000000000000000, 1.000000000000000000 ) ) ;
#18976 = LINE ( 'NONE', #18222, #21932 ) ;
#18977 = ORIENTED_EDGE ( 'NONE', *, *, #41942, .F. ) ;
#18978 = CARTESIAN_POINT ( 'NONE',  ( 0.000000000000000000, 3.267716535433071279, 0.1574803149606285035 ) ) ;
#18979 = VECTOR ( 'NONE', #7439, 39.37007874015748143 ) ;
#18980 = VERTEX_POINT ( 'NONE', #26480 ) ;
#18981 = FACE_BOUND ( 'NONE', #14108, .T. ) ;
#18982 = CARTESIAN_POINT ( 'NONE',  ( 0.5455278134075212115, 3.346456692913386100, 0.6299212598425161236 ) ) ;
#18983 = EDGE_CURVE ( 'NONE', #41982, #47028, #26736, .T. ) ;
#18984 = EDGE_CURVE ( 'NONE', #17666, #15979, #50757, .T. ) ;
#18985 = CARTESIAN_POINT ( 'NONE',  ( -1.794796351285542491, 3.267716535433071279, 1.102362204724404160 ) ) ;
#18986 = VERTEX_POINT ( 'NONE', #17984 ) ;
#18987 = ORIENTED_EDGE ( 'NONE', *, *, #41484, .F. ) ;
#18988 = CARTESIAN_POINT ( 'NONE',  ( 0.002207914879453961535, -5.712274067634378313E-18, 0.04916304461325374242 ) ) ;
#18989 = CARTESIAN_POINT ( 'NONE',  ( -0.3382312733057318832, 6.692913385826772199, -2.139420919314970693 ) ) ;
#18990 = EDGE_CURVE ( 'NONE', #11767, #1340, #21604, .T. ) ;
#18991 = DIRECTION ( 'NONE',  ( -0.000000000000000000, 1.000000000000000000, -0.000000000000000000 ) ) ;
#18992 = CARTESIAN_POINT ( 'NONE',  ( 1.773598097765477277, 1.637884173412089250, 1.477342561509449759 ) ) ;
#18993 = PLANE ( 'NONE',  #40106 ) ;
#18994 = CARTESIAN_POINT ( 'NONE',  ( -1.439733046521776139, 3.267716535433071279, 4.995077429881866871E-16 ) ) ;
#18995 = EDGE_LOOP ( 'NONE', ( #7843, #35883, #50972, #30299 ) ) ;
#18996 = VERTEX_POINT ( 'NONE', #14363 ) ;
#18997 = CARTESIAN_POINT ( 'NONE',  ( -2.695799277629577162, 1.578813927010291218, -1.205759334241492731 ) ) ;
#18998 = CARTESIAN_POINT ( 'NONE',  ( -1.909347346926324906, 0.000000000000000000, -0.4724409448818884805 ) ) ;
#18999 = EDGE_LOOP ( 'NONE', ( #26418, #25852, #45353, #16111 ) ) ;
#19000 = LINE ( 'NONE', #34756, #11713 ) ;
#19001 = EDGE_LOOP ( 'NONE', ( #36905, #15621, #10202, #7918 ) ) ;
#19002 = ORIENTED_EDGE ( 'NONE', *, *, #48548, .F. ) ;
#19003 = EDGE_CURVE ( 'NONE', #34452, #4494, #25985, .T. ) ;
#19004 = VECTOR ( 'NONE', #16291, 39.37007874015748143 ) ;
#19005 = VECTOR ( 'NONE', #27425, 39.37007874015748143 ) ;
#19006 = ORIENTED_EDGE ( 'NONE', *, *, #30468, .T. ) ;
#19007 = ORIENTED_EDGE ( 'NONE', *, *, #27044, .T. ) ;
#19008 = DIRECTION ( 'NONE',  ( 1.000000000000000000, -0.000000000000000000, 0.000000000000000000 ) ) ;
#19009 = VECTOR ( 'NONE', #15443, 39.37007874015748143 ) ;
#19010 = DIRECTION ( 'NONE',  ( -3.469446951953613696E-16, 0.000000000000000000, -1.000000000000000000 ) ) ;
#19011 = LINE ( 'NONE', #42507, #9580 ) ;
#19012 = LINE ( 'NONE', #50701, #44500 ) ;
#19013 = LINE ( 'NONE', #23143, #3859 ) ;
#19014 = CARTESIAN_POINT ( 'NONE',  ( 1.775400203342704986, 1.746929418358725172, -2.359903268218703332 ) ) ;
#19015 = ORIENTED_EDGE ( 'NONE', *, *, #37789, .T. ) ;
#19016 = ADVANCED_FACE ( 'NONE', ( #30112 ), #37364, .F. ) ;
#19017 = LINE ( 'NONE', #34775, #36546 ) ;
#19018 = DIRECTION ( 'NONE',  ( 1.000000000000000000, 0.000000000000000000, 0.000000000000000000 ) ) ;
#19019 = CARTESIAN_POINT ( 'NONE',  ( 1.560669927219590747, 0.000000000000000000, 0.1574803149606283648 ) ) ;
#19020 = CARTESIAN_POINT ( 'NONE',  ( 2.009930929872536964, 2.755905511811027164, -0.8055662819783819817 ) ) ;
#19021 = ADVANCED_FACE ( 'NONE', ( #18493 ), #10494, .F. ) ;
#19022 = VERTEX_POINT ( 'NONE', #2238 ) ;
#19023 = CARTESIAN_POINT ( 'NONE',  ( 0.000000000000000000, 3.267716535433071279, 1.417322834645662777 ) ) ;
#19024 = EDGE_CURVE ( 'NONE', #50937, #30224, #33523, .T. ) ;
#19025 = DIRECTION ( 'NONE',  ( 0.000000000000000000, 0.000000000000000000, -1.000000000000000000 ) ) ;
#19026 = VERTEX_POINT ( 'NONE', #34500 ) ;
#19027 = DIRECTION ( 'NONE',  ( -0.9998717552508122886, -0.01601477604151185785, 0.000000000000000000 ) ) ;
#19028 = ADVANCED_FACE ( 'NONE', ( #18745 ), #30617, .F. ) ;
#19029 = DIRECTION ( 'NONE',  ( -0.000000000000000000, 1.000000000000000000, -0.000000000000000000 ) ) ;
#19030 = CARTESIAN_POINT ( 'NONE',  ( 2.224044434511903923, 1.677907295117183617, 0.6708906538694197064 ) ) ;
#19031 = EDGE_LOOP ( 'NONE', ( #33348, #20278, #13252, #40346 ) ) ;
#19032 = LINE ( 'NONE', #34295, #47818 ) ;
#19033 = CARTESIAN_POINT ( 'NONE',  ( -0.5455278134075214336, 3.267716535433071279, -2.034427629037601104 ) ) ;
#19034 = CARTESIAN_POINT ( 'NONE',  ( -0.2727639067037608278, 3.346456692913386100, 0.2755905511810995412 ) ) ;
#19035 = VECTOR ( 'NONE', #30121, 39.37007874015748143 ) ;
#19036 = DIRECTION ( 'NONE',  ( 1.000000000000000000, 0.000000000000000000, 0.000000000000000000 ) ) ;
#19037 = EDGE_CURVE ( 'NONE', #6926, #10313, #27120, .T. ) ;
#19038 = DIRECTION ( 'NONE',  ( 0.000000000000000000, 1.000000000000000000, -0.000000000000000000 ) ) ;
#19039 = ORIENTED_EDGE ( 'NONE', *, *, #7322, .F. ) ;
#19040 = ORIENTED_EDGE ( 'NONE', *, *, #48239, .F. ) ;
#19041 = ORIENTED_EDGE ( 'NONE', *, *, #6101, .T. ) ;
#19042 = LINE ( 'NONE', #23171, #35329 ) ;
#19043 = ORIENTED_EDGE ( 'NONE', *, *, #2595, .F. ) ;
#19044 = ADVANCED_FACE ( 'NONE', ( #38870 ), #43231, .F. ) ;
#19045 = LINE ( 'NONE', #23684, #13092 ) ;
#19046 = VECTOR ( 'NONE', #41234, 39.37007874015748143 ) ;
#19047 = CARTESIAN_POINT ( 'NONE',  ( 1.097585813245683717, 0.000000000000000000, 0.9794755770252102645 ) ) ;
#19048 = ORIENTED_EDGE ( 'NONE', *, *, #35951, .F. ) ;
#19049 = DIRECTION ( 'NONE',  ( 1.000000000000000000, 0.000000000000000000, 0.000000000000000000 ) ) ;
#19050 = VECTOR ( 'NONE', #14907, 39.37007874015748143 ) ;
#19051 = ADVANCED_FACE ( 'NONE', ( #35254 ), #18993, .F. ) ;
#19052 = CARTESIAN_POINT ( 'NONE',  ( -1.775400203342670569, 1.205361022782829114E-17, -2.359903268218729089 ) ) ;
#19053 = CARTESIAN_POINT ( 'NONE',  ( 1.443330927545150910, 3.346456692913386100, -1.614173228346452715 ) ) ;
#19054 = ORIENTED_EDGE ( 'NONE', *, *, #2500, .F. ) ;
#19055 = ORIENTED_EDGE ( 'NONE', *, *, #28206, .F. ) ;
#19056 = LINE ( 'NONE', #11070, #19110 ) ;
#19057 = FACE_BOUND ( 'NONE', #49118, .T. ) ;
#19058 = ORIENTED_EDGE ( 'NONE', *, *, #2141, .T. ) ;
#19059 = EDGE_CURVE ( 'NONE', #17713, #33946, #11751, .T. ) ;
#19060 = CARTESIAN_POINT ( 'NONE',  ( -0.2727639067037602172, 0.000000000000000000, 2.047244094488179567 ) ) ;
#19061 = ORIENTED_EDGE ( 'NONE', *, *, #23285, .T. ) ;
#19062 = ORIENTED_EDGE ( 'NONE', *, *, #42861, .F. ) ;
#19063 = CARTESIAN_POINT ( 'NONE',  ( 0.000000000000000000, 3.267716535433071279, 0.000000000000000000 ) ) ;
#19064 = DIRECTION ( 'NONE',  ( -0.5508969814521065267, 1.288287287306305283E-16, 0.8345732537212999791 ) ) ;
#19065 = EDGE_CURVE ( 'NONE', #44866, #18296, #17002, .T. ) ;
#19066 = ORIENTED_EDGE ( 'NONE', *, *, #1075, .F. ) ;
#19067 = DIRECTION ( 'NONE',  ( 0.000000000000000000, 0.000000000000000000, 1.000000000000000000 ) ) ;
#19068 = VERTEX_POINT ( 'NONE', #46584 ) ;
#19069 = CARTESIAN_POINT ( 'NONE',  ( -2.122907315177388288, 1.559117831781008601, -2.052389032744492248 ) ) ;
#19070 = AXIS2_PLACEMENT_3D ( 'NONE', #28808, #49409, #6345 ) ;
#19071 = DIRECTION ( 'NONE',  ( -0.01601477604151182663, 0.9998717552508123996, -0.000000000000000000 ) ) ;
#19072 = VECTOR ( 'NONE', #133, 39.37007874015748143 ) ;
#19073 = CARTESIAN_POINT ( 'NONE',  ( -1.276224672482803912, 0.5249316497054298258, 1.385958525741132874 ) ) ;
#19074 = ORIENTED_EDGE ( 'NONE', *, *, #10764, .T. ) ;
#19075 = ORIENTED_EDGE ( 'NONE', *, *, #43693, .F. ) ;
#19076 = VECTOR ( 'NONE', #31122, 39.37007874015748143 ) ;
#19077 = CARTESIAN_POINT ( 'NONE',  ( 0.4788131938641111973, 1.504819983455083277, 2.914091152102192162 ) ) ;
#19078 = DIRECTION ( 'NONE',  ( 0.3930250316539278810, -1.160734090543304907E-16, -0.9195277725514489076 ) ) ;
#19079 = DIRECTION ( 'NONE',  ( 1.000000000000000000, -0.000000000000000000, 0.000000000000000000 ) ) ;
#19080 = AXIS2_PLACEMENT_3D ( 'NONE', #13295, #32156, #16660 ) ;
#19081 = CARTESIAN_POINT ( 'NONE',  ( -1.743516651958532115, 0.0004834999639498430428, -4.958524412099369637E-19 ) ) ;
#19082 = DIRECTION ( 'NONE',  ( -0.9998717552508121775, -0.01601477604151182663, 0.000000000000000000 ) ) ;
#19083 = EDGE_CURVE ( 'NONE', #45220, #29397, #27492, .T. ) ;
#19084 = AXIS2_PLACEMENT_3D ( 'NONE', #24629, #24884, #21010 ) ;
#19085 = CARTESIAN_POINT ( 'NONE',  ( 1.346254456287517387, 0.000000000000000000, 1.565948643837855814 ) ) ;
#19086 = EDGE_CURVE ( 'NONE', #50405, #3086, #3248, .T. ) ;
#19087 = LINE ( 'NONE', #42828, #30892 ) ;
#19088 = ORIENTED_EDGE ( 'NONE', *, *, #32088, .T. ) ;
#19089 = CARTESIAN_POINT ( 'NONE',  ( 2.277873973731426194, 1.656288013650806912, 1.879489153247668076 ) ) ;
#19090 = LINE ( 'NONE', #34846, #24431 ) ;
#19091 = ORIENTED_EDGE ( 'NONE', *, *, #3125, .T. ) ;
#19092 = ORIENTED_EDGE ( 'NONE', *, *, #36179, .T. ) ;
#19093 = LINE ( 'NONE', #26838, #2762 ) ;
#19094 = CARTESIAN_POINT ( 'NONE',  ( 2.164658444855302122, 5.905511811023623991, -0.04795272066889885720 ) ) ;
#19095 = VERTEX_POINT ( 'NONE', #19744 ) ;
#19096 = CARTESIAN_POINT ( 'NONE',  ( -1.621795816027382875, 0.000000000000000000, -0.6396693727619442438 ) ) ;
#19097 = ORIENTED_EDGE ( 'NONE', *, *, #23006, .T. ) ;
#19098 = LINE ( 'NONE', #30484, #45186 ) ;
#19099 = VERTEX_POINT ( 'NONE', #23119 ) ;
#19100 = VECTOR ( 'NONE', #14786, 39.37007874015748143 ) ;
#19101 = DIRECTION ( 'NONE',  ( -0.000000000000000000, 1.000000000000000000, -0.000000000000000000 ) ) ;
#19102 = DIRECTION ( 'NONE',  ( -1.000000000000000000, 0.000000000000000000, -0.000000000000000000 ) ) ;
#19103 = EDGE_CURVE ( 'NONE', #38248, #2104, #47333, .T. ) ;
#19104 = ORIENTED_EDGE ( 'NONE', *, *, #2335, .F. ) ;
#19105 = VECTOR ( 'NONE', #25027, 39.37007874015748143 ) ;
#19106 = CARTESIAN_POINT ( 'NONE',  ( -0.2727639067037608278, 3.346456692913386100, -1.929133858267710000 ) ) ;
#19107 = EDGE_LOOP ( 'NONE', ( #41533, #7353, #7799, #14214 ) ) ;
#19108 = ORIENTED_EDGE ( 'NONE', *, *, #26005, .T. ) ;
#19109 = LINE ( 'NONE', #18366, #7034 ) ;
#19111 = FACE_OUTER_BOUND ( 'NONE', #49377, .T. ) ;
#19110 = VECTOR ( 'NONE', #30182, 39.37007874015748143 ) ;
#19112 = CARTESIAN_POINT ( 'NONE',  ( 0.8515791614234311524, 0.000000000000000000, 1.521253268579216167 ) ) ;
#19113 = EDGE_CURVE ( 'NONE', #30581, #19191, #26489, .T. ) ;
#19114 = AXIS2_PLACEMENT_3D ( 'NONE', #23529, #292, #23281 ) ;
#19115 = ORIENTED_EDGE ( 'NONE', *, *, #28603, .F. ) ;
#19116 = EDGE_CURVE ( 'NONE', #28931, #19562, #39376, .T. ) ;
#19117 = CARTESIAN_POINT ( 'NONE',  ( -2.454875160333845674, 3.232777166330581320, 0.1574803149606286423 ) ) ;
#19118 = DIRECTION ( 'NONE',  ( -0.000000000000000000, 1.000000000000000000, -0.000000000000000000 ) ) ;
#19119 = EDGE_CURVE ( 'NONE', #9992, #34145, #39630, .T. ) ;
#19120 = ORIENTED_EDGE ( 'NONE', *, *, #15804, .T. ) ;
#19121 = CARTESIAN_POINT ( 'NONE',  ( 0.000000000000000000, 3.267716535433071279, -0.6692913385826760875 ) ) ;
#19122 = EDGE_CURVE ( 'NONE', #2745, #9737, #46830, .T. ) ;
#19123 = ORIENTED_EDGE ( 'NONE', *, *, #13986, .T. ) ;
#19124 = EDGE_LOOP ( 'NONE', ( #15509, #13744, #34803, #8824 ) ) ;
#19125 = LENGTH_MEASURE_WITH_UNIT ( LENGTH_MEASURE( 0.02539999999999999897 ), #26623 );
#19127 = ADVANCED_FACE ( 'NONE', ( #47588 ), #11253, .F. ) ;
#19126 = ORIENTED_EDGE ( 'NONE', *, *, #21092, .T. ) ;
#19128 = FACE_OUTER_BOUND ( 'NONE', #8132, .T. ) ;
#19129 = DIRECTION ( 'NONE',  ( -0.1342332658176667304, -1.160734090543304907E-16, 0.9909497617679332571 ) ) ;
#19130 = CARTESIAN_POINT ( 'NONE',  ( 1.909828200462996062, 1.049866565877818125, 0.6722859869522012088 ) ) ;
#19131 = CARTESIAN_POINT ( 'NONE',  ( 0.7423782071083090406, 3.267716535433071279, -2.575641807848711180E-16 ) ) ;
#19132 = VERTEX_POINT ( 'NONE', #28003 ) ;
#19133 = ORIENTED_EDGE ( 'NONE', *, *, #39966, .T. ) ;
#19134 = SURFACE_SIDE_STYLE ('',( #24029 ) ) ;
#19135 = LINE ( 'NONE', #12158, #48163 ) ;
#19136 = ORIENTED_EDGE ( 'NONE', *, *, #20545, .F. ) ;
#19137 = DIRECTION ( 'NONE',  ( 0.000000000000000000, -1.000000000000000000, 0.000000000000000000 ) ) ;
#19138 = CARTESIAN_POINT ( 'NONE',  ( 1.695772546416036919, 1.205361022782829114E-17, -2.417756147381349141 ) ) ;
#19139 = EDGE_CURVE ( 'NONE', #47679, #12647, #37645, .T. ) ;
#19140 = VECTOR ( 'NONE', #17051, 39.37007874015748143 ) ;
#19141 = ADVANCED_FACE ( 'NONE', ( #42735 ), #23617, .F. ) ;
#19142 = DIRECTION ( 'NONE',  ( 1.000000000000000000, 0.000000000000000000, 0.000000000000000000 ) ) ;
#19143 = DIRECTION ( 'NONE',  ( 1.734723475976806848E-16, -0.000000000000000000, 1.000000000000000000 ) ) ;
#19145 = LINE ( 'NONE', #23272, #41910 ) ;
#19144 = AXIS2_PLACEMENT_3D ( 'NONE', #36598, #28579, #12849 ) ;
#19146 = ORIENTED_EDGE ( 'NONE', *, *, #37927, .F. ) ;
#19147 = EDGE_CURVE ( 'NONE', #41494, #1578, #27236, .T. ) ;
#19148 = DIRECTION ( 'NONE',  ( 0.000000000000000000, -1.000000000000000000, 0.000000000000000000 ) ) ;
#19149 = VECTOR ( 'NONE', #49885, 39.37007874015748143 ) ;
#19150 = VERTEX_POINT ( 'NONE', #44760 ) ;
#19151 = DIRECTION ( 'NONE',  ( -0.000000000000000000, 1.000000000000000000, -0.000000000000000000 ) ) ;
#19152 = CARTESIAN_POINT ( 'NONE',  ( -0.8942052331142547050, 3.267716535433071279, 1.259842519685033357 ) ) ;
#19153 = CARTESIAN_POINT ( 'NONE',  ( -1.481515513156636876, 0.000000000000000000, -0.9189724476880739568 ) ) ;
#19154 = VERTEX_POINT ( 'NONE', #37045 ) ;
#19155 = EDGE_CURVE ( 'NONE', #9746, #47004, #13038, .T. ) ;
#19156 = DIRECTION ( 'NONE',  ( -0.000000000000000000, 1.000000000000000000, -0.000000000000000000 ) ) ;
#19157 = VERTEX_POINT ( 'NONE', #28771 ) ;
#19158 = DIRECTION ( 'NONE',  ( 0.000000000000000000, 0.000000000000000000, 1.000000000000000000 ) ) ;
#19159 = EDGE_LOOP ( 'NONE', ( #51036, #49225, #41907, #29222 ) ) ;
#19160 = DIRECTION ( 'NONE',  ( 1.000000000000000000, 0.000000000000000000, -3.469446951953613696E-16 ) ) ;
#19161 = ORIENTED_EDGE ( 'NONE', *, *, #49429, .F. ) ;
#19162 = DIRECTION ( 'NONE',  ( -1.000000000000000000, 0.000000000000000000, 0.000000000000000000 ) ) ;
#19163 = CARTESIAN_POINT ( 'NONE',  ( 1.266373210825830764, 1.738989517266293472, -2.667458607394062486 ) ) ;
#19164 = DIRECTION ( 'NONE',  ( 0.9998717552508121775, 0.01601477604151182663, 0.000000000000000000 ) ) ;
#19165 = ORIENTED_EDGE ( 'NONE', *, *, #40433, .F. ) ;
#19166 = ORIENTED_EDGE ( 'NONE', *, *, #11220, .T. ) ;
#19167 = ORIENTED_EDGE ( 'NONE', *, *, #17337, .T. ) ;
#19168 = PLANE ( 'NONE',  #16670 ) ;
#19169 = DIRECTION ( 'NONE',  ( -0.01601477604151182663, 0.9998717552508123996, -0.000000000000000000 ) ) ;
#19170 = ORIENTED_EDGE ( 'NONE', *, *, #35313, .F. ) ;
#19171 = ORIENTED_EDGE ( 'NONE', *, *, #35471, .F. ) ;
#19172 = CARTESIAN_POINT ( 'NONE',  ( 1.388309139374679146, 1.631713065620022274, -1.827118126197171399 ) ) ;
#19173 = DIRECTION ( 'NONE',  ( -1.000000000000000000, 0.000000000000000000, 1.734723475976806848E-16 ) ) ;
#19174 = CARTESIAN_POINT ( 'NONE',  ( 0.4696143004045484903, 3.267716535433071279, 1.417322834645662777 ) ) ;
#19175 = ORIENTED_EDGE ( 'NONE', *, *, #48885, .F. ) ;
#19176 = ORIENTED_EDGE ( 'NONE', *, *, #45402, .T. ) ;
#19177 = EDGE_CURVE ( 'NONE', #12919, #34200, #29023, .T. ) ;
#19178 = CARTESIAN_POINT ( 'NONE',  ( -0.07591351300297277671, 0.000000000000000000, 2.047244094488179567 ) ) ;
#19179 = FACE_OUTER_BOUND ( 'NONE', #36850, .T. ) ;
#19180 = CARTESIAN_POINT ( 'NONE',  ( -1.514466370293032993, 0.000000000000000000, 2.534789744887398388 ) ) ;
#19181 = EDGE_CURVE ( 'NONE', #1516, #19985, #22741, .T. ) ;
#19182 = ORIENTED_EDGE ( 'NONE', *, *, #44369, .T. ) ;
#19183 = CARTESIAN_POINT ( 'NONE',  ( 0.3136974817028393425, 1.724153038295522800, -2.936457595020219635 ) ) ;
#19184 = ADVANCED_FACE ( 'NONE', ( #39887 ), #36014, .T. ) ;
#19185 = VECTOR ( 'NONE', #17360, 39.37007874015748143 ) ;
#19186 = DIRECTION ( 'NONE',  ( 1.734723475976806848E-16, -0.000000000000000000, 1.000000000000000000 ) ) ;
#19187 = VERTEX_POINT ( 'NONE', #33178 ) ;
#19188 = CARTESIAN_POINT ( 'NONE',  ( -1.901641471869980782, 5.905511811023623991, 1.079202499698819651 ) ) ;
#19189 = ORIENTED_EDGE ( 'NONE', *, *, #35472, .T. ) ;
#19190 = VECTOR ( 'NONE', #27189, 39.37007874015748143 ) ;
#19191 = VERTEX_POINT ( 'NONE', #28254 ) ;
#19192 = DIRECTION ( 'NONE',  ( -0.000000000000000000, 0.000000000000000000, 1.000000000000000000 ) ) ;
#19193 = DIRECTION ( 'NONE',  ( -3.469446951953613696E-16, 0.000000000000000000, -1.000000000000000000 ) ) ;
#19194 = AXIS2_PLACEMENT_3D ( 'NONE', #14392, #26012, #10015 ) ;
#19195 = VECTOR ( 'NONE', #49358, 39.37007874015748143 ) ;
#19196 = CARTESIAN_POINT ( 'NONE',  ( -0.8329809839909436686, 1.533199950842965453, -2.833254665166566877 ) ) ;
#19197 = LINE ( 'NONE', #2702, #10439 ) ;
#19198 = CARTESIAN_POINT ( 'NONE',  ( 0.6233543567505464011, 1.574803149606302854, -2.073689640095370379 ) ) ;
#19199 = ORIENTED_EDGE ( 'NONE', *, *, #23681, .T. ) ;
#19200 = VECTOR ( 'NONE', #11477, 39.37007874015748143 ) ;
#19201 = ADVANCED_FACE ( 'NONE', ( #1155 ), #28512, .T. ) ;
#19202 = ORIENTED_EDGE ( 'NONE', *, *, #17366, .T. ) ;
#19203 = FACE_OUTER_BOUND ( 'NONE', #42357, .T. ) ;
#19204 = DIRECTION ( 'NONE',  ( -5.207613805427244364E-18, -1.000000000000000000, -1.159565308550900415E-16 ) ) ;
#19205 = EDGE_CURVE ( 'NONE', #9948, #3567, #48611, .T. ) ;
#19206 = EDGE_CURVE ( 'NONE', #23218, #2123, #4518, .T. ) ;
#19207 = CARTESIAN_POINT ( 'NONE',  ( -1.166969139818015977, 0.000000000000000000, -1.417322834645664109 ) ) ;
#19208 = CARTESIAN_POINT ( 'NONE',  ( -1.363819533518803473, 3.267716535433071279, -1.299212598425192544 ) ) ;
#19209 = LINE ( 'NONE', #34969, #45971 ) ;
#19210 = ORIENTED_EDGE ( 'NONE', *, *, #1953, .F. ) ;
#19211 = CARTESIAN_POINT ( 'NONE',  ( 0.07982360342473591996, 1.709180471932028711, 0.000000000000000000 ) ) ;
#19212 = ADVANCED_FACE ( 'NONE', ( #48860 ), #8392, .F. ) ;
#19213 = DIRECTION ( 'NONE',  ( 1.000000000000000000, 0.000000000000000000, 0.000000000000000000 ) ) ;
#19214 = ORIENTED_EDGE ( 'NONE', *, *, #12150, .F. ) ;
#19215 = DIRECTION ( 'NONE',  ( 1.000000000000000000, 0.000000000000000000, -3.469446951953613696E-16 ) ) ;
#19216 = DIRECTION ( 'NONE',  ( 0.000000000000000000, -1.000000000000000000, 0.000000000000000000 ) ) ;
#19217 = DIRECTION ( 'NONE',  ( 1.000000000000000000, 0.000000000000000000, 0.000000000000000000 ) ) ;
#19218 = B_SPLINE_CURVE_WITH_KNOTS ( 'NONE', 3,
 ( #27223, #35238, #34986, #14351 ),
 .UNSPECIFIED., .F., .F.,
 ( 4, 4 ),
 ( 2.219923784601946562E-07, 0.01886371725601659888 ),
 .UNSPECIFIED. ) ;
#19219 = CARTESIAN_POINT ( 'NONE',  ( -0.07591351300297288773, 3.267716535433071279, 2.633779063002553116E-17 ) ) ;
#19220 = CARTESIAN_POINT ( 'NONE',  ( 1.091055626815042645, 0.000000000000000000, -0.8267716535433055070 ) ) ;
#19221 = CARTESIAN_POINT ( 'NONE',  ( -0.8942052331142552601, 3.346456692913386100, -0.3149606299212593941 ) ) ;
#19222 = VECTOR ( 'NONE', #24529, 39.37007874015748854 ) ;
#19223 = ORIENTED_EDGE ( 'NONE', *, *, #31093, .F. ) ;
#19224 = AXIS2_PLACEMENT_3D ( 'NONE', #16638, #28492, #40391 ) ;
#19225 = DIRECTION ( 'NONE',  ( -1.206139481778042838E-16, 1.000000000000000000, 4.526717189434675613E-17 ) ) ;
#19226 = ORIENTED_EDGE ( 'NONE', *, *, #563, .F. ) ;
#19227 = FACE_OUTER_BOUND ( 'NONE', #20249, .T. ) ;
#19228 = AXIS2_PLACEMENT_3D ( 'NONE', #36419, #28661, #9046 ) ;
#19229 = VECTOR ( 'NONE', #30714, 39.37007874015748143 ) ;
#19230 = CARTESIAN_POINT ( 'NONE',  ( -1.363819533518803029, 3.346456692913386100, 1.220472440944875281 ) ) ;
#19231 = DIRECTION ( 'NONE',  ( 1.000000000000000000, 0.000000000000000000, 0.000000000000000000 ) ) ;
#19232 = VERTEX_POINT ( 'NONE', #44262 ) ;
#19233 = ORIENTED_EDGE ( 'NONE', *, *, #5033, .F. ) ;
#19234 = LINE ( 'NONE', #15118, #45442 ) ;
#19235 = LINE ( 'NONE', #22614, #21335 ) ;
#19236 = DIRECTION ( 'NONE',  ( -0.000000000000000000, 1.000000000000000000, -0.000000000000000000 ) ) ;
#19237 = DIRECTION ( 'NONE',  ( -1.000000000000000000, 0.000000000000000000, -0.000000000000000000 ) ) ;
#19238 = DIRECTION ( 'NONE',  ( -3.469446951953613696E-16, 0.000000000000000000, -1.000000000000000000 ) ) ;
#19239 = PLANE ( 'NONE',  #42916 ) ;
#19240 = VERTEX_POINT ( 'NONE', #44515 ) ;
#19241 = CARTESIAN_POINT ( 'NONE',  ( -1.536664496436148184E-16, 0.000000000000000000, -1.771653543307081025 ) ) ;
#19242 = DIRECTION ( 'NONE',  ( -0.000000000000000000, 1.000000000000000000, -0.000000000000000000 ) ) ;
#19243 = DIRECTION ( 'NONE',  ( -3.469446951953613696E-16, 0.000000000000000000, -1.000000000000000000 ) ) ;
#19244 = EDGE_CURVE ( 'NONE', #22473, #18996, #46127, .T. ) ;
#19245 = ORIENTED_EDGE ( 'NONE', *, *, #8530, .F. ) ;
#19246 = EDGE_CURVE ( 'NONE', #35070, #26916, #21037, .T. ) ;
#19247 = CARTESIAN_POINT ( 'NONE',  ( 0.2810168695315136689, 1.016046776276138708, -2.573346254327823157 ) ) ;
#19248 = EDGE_LOOP ( 'NONE', ( #39109, #18347, #40464, #48185 ) ) ;
#19249 = VERTEX_POINT ( 'NONE', #32671 ) ;
#19250 = ADVANCED_FACE ( 'NONE', ( #20257 ), #8901, .F. ) ;
#19251 = ORIENTED_EDGE ( 'NONE', *, *, #2747, .T. ) ;
#19252 = ORIENTED_EDGE ( 'NONE', *, *, #7192, .F. ) ;
#19253 = CARTESIAN_POINT ( 'NONE',  ( -1.909347346926324906, 3.346456692913386100, -0.9842519685039344823 ) ) ;
#19254 = ORIENTED_EDGE ( 'NONE', *, *, #46423, .T. ) ;
#19255 = VECTOR ( 'NONE', #39329, 39.37007874015748143 ) ;
#19256 = VECTOR ( 'NONE', #33282, 39.37007874015748143 ) ;
#19257 = DIRECTION ( 'NONE',  ( -1.000000000000000000, 0.000000000000000000, -0.000000000000000000 ) ) ;
#19258 = FACE_OUTER_BOUND ( 'NONE', #20446, .T. ) ;
#19259 = DIRECTION ( 'NONE',  ( 0.000000000000000000, -1.000000000000000000, 0.000000000000000000 ) ) ;
#19260 = VECTOR ( 'NONE', #42974, 39.37007874015748143 ) ;
#19261 = AXIS2_PLACEMENT_3D ( 'NONE', #30905, #36244, #19269 ) ;
#19262 = EDGE_CURVE ( 'NONE', #22025, #48160, #8646, .T. ) ;
#19263 = CARTESIAN_POINT ( 'NONE',  ( 2.339241080213585899, 1.755713673067765379, 1.802537235681918037 ) ) ;
#19264 = FACE_OUTER_BOUND ( 'NONE', #3178, .T. ) ;
#19265 = PLANE ( 'NONE',  #47576 ) ;
#19266 = VECTOR ( 'NONE', #34599, 39.37007874015748143 ) ;
#19267 = ORIENTED_EDGE ( 'NONE', *, *, #46727, .F. ) ;
#19268 = CARTESIAN_POINT ( 'NONE',  ( -2.287922694693813913E-16, 3.267716535433071279, 3.968913209705475983E-32 ) ) ;
#19269 = DIRECTION ( 'NONE',  ( -0.9998717552508122886, -0.01601477604151182316, 0.000000000000000000 ) ) ;
#19270 = EDGE_CURVE ( 'NONE', #4582, #12335, #48356, .T. ) ;
#19271 = LINE ( 'NONE', #39408, #40867 ) ;
#19272 = DIRECTION ( 'NONE',  ( -0.1342332658176667026, 0.000000000000000000, 0.9909497617679331460 ) ) ;
#19273 = EDGE_LOOP ( 'NONE', ( #19923, #12653, #34484, #5476 ) ) ;
#19274 = FACE_OUTER_BOUND ( 'NONE', #42282, .T. ) ;
#19275 = DIRECTION ( 'NONE',  ( 1.734723475976806848E-16, 0.000000000000000000, 1.000000000000000000 ) ) ;
#19276 = ORIENTED_EDGE ( 'NONE', *, *, #48659, .F. ) ;
#19277 = FACE_OUTER_BOUND ( 'NONE', #37949, .T. ) ;
#19278 = CARTESIAN_POINT ( 'NONE',  ( 0.04921259842519669359, 1.614036899992937313, 2.481772132991067803 ) ) ;
#19279 = DIRECTION ( 'NONE',  ( 1.000000000000000000, 0.000000000000000000, 0.000000000000000000 ) ) ;
#19280 = VERTEX_POINT ( 'NONE', #47844 ) ;
#19281 = DIRECTION ( 'NONE',  ( -0.9998717552508122886, -0.01601477604151180928, 0.000000000000000000 ) ) ;
#19282 = DIRECTION ( 'NONE',  ( -0.01601477604151182663, 0.9998717552508123996, -0.000000000000000000 ) ) ;
#19283 = FACE_OUTER_BOUND ( 'NONE', #24482, .T. ) ;
#19284 = PLANE ( 'NONE',  #39142 ) ;
#19285 = ORIENTED_EDGE ( 'NONE', *, *, #28160, .T. ) ;
#19286 = AXIS2_PLACEMENT_3D ( 'NONE', #14065, #29813, #26191 ) ;
#19287 = ORIENTED_EDGE ( 'NONE', *, *, #23545, .F. ) ;
#19288 = EDGE_LOOP ( 'NONE', ( #33853, #21730, #9731, #49504 ) ) ;
#19289 = AXIS2_PLACEMENT_3D ( 'NONE', #36421, #9305, #21692 ) ;
#19290 = DIRECTION ( 'NONE',  ( -3.469446951953613696E-16, 0.000000000000000000, -1.000000000000000000 ) ) ;
#19291 = ORIENTED_EDGE ( 'NONE', *, *, #43343, .F. ) ;
#19292 = CARTESIAN_POINT ( 'NONE',  ( 0.000000000000000000, 6.692913385826772199, 0.000000000000000000 ) ) ;
#19293 = CARTESIAN_POINT ( 'NONE',  ( 0.000000000000000000, 0.000000000000000000, 0.000000000000000000 ) ) ;
#19294 = VERTEX_POINT ( 'NONE', #40153 ) ;
#19295 = AXIS2_PLACEMENT_3D ( 'NONE', #22051, #33932, #30049 ) ;
#19296 = AXIS2_PLACEMENT_3D ( 'NONE', #35157, #23519, #4420 ) ;
#19297 = CARTESIAN_POINT ( 'NONE',  ( 1.091055626815042645, 3.267716535433071279, 0.1181102362204704270 ) ) ;
#19298 = VERTEX_POINT ( 'NONE', #20523 ) ;
#19299 = PLANE ( 'NONE',  #10064 ) ;
#19300 = ADVANCED_FACE ( 'NONE', ( #21291 ), #36278, .T. ) ;
#19301 = AXIS2_PLACEMENT_3D ( 'NONE', #16116, #47313, #19971 ) ;
#19302 = ORIENTED_EDGE ( 'NONE', *, *, #42774, .T. ) ;
#19304 = EDGE_LOOP ( 'NONE', ( #42808, #6244, #33768, #8564 ) ) ;
#19303 = ADVANCED_FACE ( 'NONE', ( #6566 ), #49121, .F. ) ;
#19305 = CARTESIAN_POINT ( 'NONE',  ( -1.363819533518803473, 0.000000000000000000, 1.850393700787392293 ) ) ;
#19306 = ORIENTED_EDGE ( 'NONE', *, *, #44124, .T. ) ;
#19307 = EDGE_CURVE ( 'NONE', #36491, #49628, #2435, .T. ) ;
#19308 = CARTESIAN_POINT ( 'NONE',  ( 0.3546377434558362074, 1.615156926475952881, 2.229828021450985798 ) ) ;
#19310 = ORIENTED_EDGE ( 'NONE', *, *, #4749, .F. ) ;
#19309 = EDGE_CURVE ( 'NONE', #3695, #32172, #49620, .T. ) ;
#19311 = ORIENTED_EDGE ( 'NONE', *, *, #1210, .F. ) ;
#19312 = CARTESIAN_POINT ( 'NONE',  ( 0.000000000000000000, 3.267716535433071279, -1.417322834645665219 ) ) ;
#19313 = DIRECTION ( 'NONE',  ( 1.000000000000000000, -0.000000000000000000, 0.000000000000000000 ) ) ;
#19314 = VERTEX_POINT ( 'NONE', #42169 ) ;
#19315 = CARTESIAN_POINT ( 'NONE',  ( 2.106197740627112402, 3.267716535433071279, 0.02067487291359298637 ) ) ;
#19316 = ORIENTED_EDGE ( 'NONE', *, *, #16505, .F. ) ;
#19317 = DIRECTION ( 'NONE',  ( 0.7071067811865486830, 0.000000000000000000, 0.7071067811865462405 ) ) ;
#19318 = DIRECTION ( 'NONE',  ( -0.000000000000000000, 0.000000000000000000, 1.000000000000000000 ) ) ;
#19319 = EDGE_CURVE ( 'NONE', #1960, #25880, #14050, .T. ) ;
#19320 = DIRECTION ( 'NONE',  ( 0.7071067811865483499, -0.000000000000000000, 0.7071067811865466846 ) ) ;
#19321 = ORIENTED_EDGE ( 'NONE', *, *, #7668, .F. ) ;
#19322 = EDGE_LOOP ( 'NONE', ( #23431, #8213, #8819, #17391 ) ) ;
#19323 = VECTOR ( 'NONE', #18706, 39.37007874015748143 ) ;
#19324 = DIRECTION ( 'NONE',  ( 0.000000000000000000, 0.000000000000000000, -1.000000000000000000 ) ) ;
#19325 = DIRECTION ( 'NONE',  ( 1.000000000000000000, -0.000000000000000000, 0.000000000000000000 ) ) ;
#19326 = CIRCLE ( 'NONE', #16879, 0.8858267716535433989 ) ;
#19327 = DIRECTION ( 'NONE',  ( 1.000000000000000000, 0.000000000000000000, 0.000000000000000000 ) ) ;
#19328 = EDGE_CURVE ( 'NONE', #9804, #47774, #17925, .T. ) ;
#19329 = VECTOR ( 'NONE', #39779, 39.37007874015748143 ) ;
#19330 = DIRECTION ( 'NONE',  ( 3.986037398843765983E-20, 1.000000000000000000, 1.160734090543304660E-16 ) ) ;
#19331 = VECTOR ( 'NONE', #17024, 39.37007874015748143 ) ;
#19332 = FACE_OUTER_BOUND ( 'NONE', #31803, .T. ) ;
#19333 = VECTOR ( 'NONE', #41775, 39.37007874015748143 ) ;
#19334 = DIRECTION ( 'NONE',  ( 0.2225209339563184452, 1.131543365815173240E-16, -0.9749279121818227312 ) ) ;
#19335 = CARTESIAN_POINT ( 'NONE',  ( -0.8182917201112819283, 0.000000000000000000, 0.1574803149606285035 ) ) ;
#19336 = VECTOR ( 'NONE', #40804, 39.37007874015748143 ) ;
#19337 = ORIENTED_EDGE ( 'NONE', *, *, #6158, .F. ) ;
#19338 = PLANE ( 'NONE',  #13581 ) ;
#19339 = ORIENTED_EDGE ( 'NONE', *, *, #4004, .T. ) ;
#19340 = EDGE_CURVE ( 'NONE', #13566, #50909, #33688, .T. ) ;
#19341 = ORIENTED_EDGE ( 'NONE', *, *, #3402, .T. ) ;
#19342 = PLANE ( 'NONE',  #6077 ) ;
#19343 = LINE ( 'NONE', #6477, #31132 ) ;
#19344 = ORIENTED_EDGE ( 'NONE', *, *, #21668, .F. ) ;
#19345 = DIRECTION ( 'NONE',  ( -0.000000000000000000, 1.000000000000000000, -0.000000000000000000 ) ) ;
#19346 = VERTEX_POINT ( 'NONE', #22053 ) ;
#19347 = FACE_OUTER_BOUND ( 'NONE', #16093, .T. ) ;
#19348 = ORIENTED_EDGE ( 'NONE', *, *, #31656, .T. ) ;
#19349 = DIRECTION ( 'NONE',  ( 1.000000000000000000, 0.000000000000000000, -0.000000000000000000 ) ) ;
#19350 = CARTESIAN_POINT ( 'NONE',  ( -0.2727639067037608278, 3.346456692913386100, 2.165354330708650465 ) ) ;
#19351 = ORIENTED_EDGE ( 'NONE', *, *, #6982, .F. ) ;
#19352 = DIRECTION ( 'NONE',  ( -0.000000000000000000, 1.000000000000000000, -0.000000000000000000 ) ) ;
#19353 = VECTOR ( 'NONE', #33335, 39.37007874015748143 ) ;
#19354 = VERTEX_POINT ( 'NONE', #25409 ) ;
#19355 = VERTEX_POINT ( 'NONE', #38318 ) ;
#19356 = VECTOR ( 'NONE', #10932, 39.37007874015748143 ) ;
#19357 = VECTOR ( 'NONE', #31734, 39.37007874015748143 ) ;
#19358 = CARTESIAN_POINT ( 'NONE',  ( 1.287906020515830141, 3.267716535433071279, 0.4330708661417287386 ) ) ;
#19359 = LINE ( 'NONE', #24270, #10836 ) ;
#19360 = DIRECTION ( 'NONE',  ( -1.000000000000000000, 0.000000000000000000, -0.000000000000000000 ) ) ;
#19361 = AXIS2_PLACEMENT_3D ( 'NONE', #32981, #17466, #9466 ) ;
#19362 = ADVANCED_FACE ( 'NONE', ( #37811 ), #28595, .T. ) ;
#19363 = VERTEX_POINT ( 'NONE', #6807 ) ;
#19364 = CARTESIAN_POINT ( 'NONE',  ( -0.4349608091551079303, 6.692913385826772199, 2.121218629000294342 ) ) ;
#19365 = DIRECTION ( 'NONE',  ( -0.000000000000000000, 1.000000000000000000, -0.000000000000000000 ) ) ;
#19366 = EDGE_CURVE ( 'NONE', #18533, #13717, #34438, .T. ) ;
#19367 = VERTEX_POINT ( 'NONE', #2680 ) ;
#19368 = CARTESIAN_POINT ( 'NONE',  ( -0.9970034594589531896, 1.699817861067899116, 2.516448948158077403 ) ) ;
#19369 = VECTOR ( 'NONE', #50177, 39.37007874015748143 ) ;
#19370 = VERTEX_POINT ( 'NONE', #49871 ) ;
#19371 = VERTEX_POINT ( 'NONE', #1921 ) ;
#19372 = DIRECTION ( 'NONE',  ( 0.09013854046061978154, -0.8080977755150033914, -0.5821108388711998538 ) ) ;
#19373 = EDGE_LOOP ( 'NONE', ( #25633, #12872, #45734, #39831 ) ) ;
#19374 = CYLINDRICAL_SURFACE ( 'NONE', #49016, 2.164630168518208109 ) ;
#19375 = DIRECTION ( 'NONE',  ( -1.000000000000000000, -0.000000000000000000, -0.000000000000000000 ) ) ;
#19376 = FACE_OUTER_BOUND ( 'NONE', #8894, .T. ) ;
#19377 = CARTESIAN_POINT ( 'NONE',  ( -0.07591351300297284610, 3.267716535433071279, 1.535433070866133898 ) ) ;
#19378 = ORIENTED_EDGE ( 'NONE', *, *, #38559, .F. ) ;
#19379 = ORIENTED_EDGE ( 'NONE', *, *, #14445, .F. ) ;
#19380 = CARTESIAN_POINT ( 'NONE',  ( -1.166969139818016199, 3.346456692913386100, -1.929133858267710000 ) ) ;
#19381 = ORIENTED_EDGE ( 'NONE', *, *, #3385, .T. ) ;
#19382 = CARTESIAN_POINT ( 'NONE',  ( -1.901721518280075296, 3.267716535433071279, 0.9055118110236167750 ) ) ;
#19383 = CARTESIAN_POINT ( 'NONE',  ( 0.000000000000000000, 3.267716535433071279, -1.417322834645664109 ) ) ;
#19384 = EDGE_CURVE ( 'NONE', #39693, #39803, #5795, .T. ) ;
#19385 = CARTESIAN_POINT ( 'NONE',  ( 0.000000000000000000, 3.267716535433071279, 1.889763779527550369 ) ) ;
#19386 = CARTESIAN_POINT ( 'NONE',  ( 1.636583440222563857, 0.000000000000000000, 0.7480314960629872445 ) ) ;
#19387 = FACE_OUTER_BOUND ( 'NONE', #5804, .T. ) ;
#19388 = ORIENTED_EDGE ( 'NONE', *, *, #10469, .F. ) ;
#19389 = VECTOR ( 'NONE', #26268, 39.37007874015748143 ) ;
#19390 = FACE_OUTER_BOUND ( 'NONE', #5247, .T. ) ;
#19391 = LENGTH_MEASURE_WITH_UNIT ( LENGTH_MEASURE( 0.02539999999999999897 ), #22279 );
#19392 = CIRCLE ( 'NONE', #41684, 2.246510896728926010 ) ;
#19393 = ADVANCED_FACE ( 'NONE', ( #22309 ), #13801, .T. ) ;
#19394 = VECTOR ( 'NONE', #18357, 39.37007874015748143 ) ;
#19395 = ORIENTED_EDGE ( 'NONE', *, *, #15654, .T. ) ;
#19396 = DIRECTION ( 'NONE',  ( 0.000000000000000000, 0.000000000000000000, 1.000000000000000000 ) ) ;
#19397 = DIRECTION ( 'NONE',  ( 1.734723475976806848E-16, 0.000000000000000000, 1.000000000000000000 ) ) ;
#19398 = CARTESIAN_POINT ( 'NONE',  ( 2.093903048064389427, 0.000000000000000000, -0.4274415146361335571 ) ) ;
#19399 = VECTOR ( 'NONE', #2448, 39.37007874015748143 ) ;
#19400 = VERTEX_POINT ( 'NONE', #29284 ) ;
#19401 = VECTOR ( 'NONE', #38684, 39.37007874015748143 ) ;
#19402 = EDGE_CURVE ( 'NONE', #7644, #35147, #33934, .T. ) ;
#19403 = EDGE_LOOP ( 'NONE', ( #37260, #21867, #16422, #25324 ) ) ;
#19404 = CARTESIAN_POINT ( 'NONE',  ( -1.091055626815042645, 3.346456692913386100, -7.512581982576723358E-16 ) ) ;
#19405 = EDGE_LOOP ( 'NONE', ( #25369, #15022, #15880, #44109 ) ) ;
#19406 = CARTESIAN_POINT ( 'NONE',  ( -1.236813753895213308, 0.000000000000000000, -2.681693691597581974 ) ) ;
#19407 = ORIENTED_EDGE ( 'NONE', *, *, #46856, .F. ) ;
#19408 = EDGE_CURVE ( 'NONE', #42847, #16575, #4801, .T. ) ;
#19409 = CARTESIAN_POINT ( 'NONE',  ( 0.000000000000000000, 5.905511811023623991, 0.000000000000000000 ) ) ;
#19410 = CARTESIAN_POINT ( 'NONE',  ( -0.06966273521059175577, 2.755905511811024056, 0.3674709282358789575 ) ) ;
#19411 = DIRECTION ( 'NONE',  ( 3.986037398843765983E-20, 1.000000000000000000, 1.160734090543304660E-16 ) ) ;
#19412 = ORIENTED_EDGE ( 'NONE', *, *, #12916, .F. ) ;
#19413 = ORIENTED_EDGE ( 'NONE', *, *, #49137, .F. ) ;
#19414 = ORIENTED_EDGE ( 'NONE', *, *, #22416, .F. ) ;
#19415 = DIRECTION ( 'NONE',  ( 1.734723475976806848E-16, 0.000000000000000000, 1.000000000000000000 ) ) ;
#19416 = CARTESIAN_POINT ( 'NONE',  ( -0.8942052331142552601, 0.000000000000000000, -0.6299212598425177889 ) ) ;
#19417 = ORIENTED_EDGE ( 'NONE', *, *, #24272, .T. ) ;
#19418 = ORIENTED_EDGE ( 'NONE', *, *, #46128, .F. ) ;
#19419 = CARTESIAN_POINT ( 'NONE',  ( -2.277873973731453727, 1.683757167080951245, 1.879489153247634992 ) ) ;
#19420 = LINE ( 'NONE', #3693, #30220 ) ;
#19421 = LINE ( 'NONE', #34688, #22822 ) ;
#19422 = EDGE_CURVE ( 'NONE', #32147, #20825, #2177, .T. ) ;
#19423 = ORIENTED_EDGE ( 'NONE', *, *, #5451, .T. ) ;
#19424 = ORIENTED_EDGE ( 'NONE', *, *, #3547, .T. ) ;
#19425 = DIRECTION ( 'NONE',  ( 7.237058681235334921E-17, -1.000000000000000000, -9.074984547606431700E-17 ) ) ;
#19426 = DIRECTION ( 'NONE',  ( 0.3930250316539147803, 0.000000000000000000, 0.9195277725514544587 ) ) ;
#19427 = LINE ( 'NONE', #24079, #48374 ) ;
#19428 = EDGE_CURVE ( 'NONE', #23628, #32481, #18431, .T. ) ;
#19429 = ADVANCED_FACE ( 'NONE', ( #10174 ), #5499, .F. ) ;
#19430 = VERTEX_POINT ( 'NONE', #30306 ) ;
#19431 = DIRECTION ( 'NONE',  ( 1.000000000000000000, -0.000000000000000000, -0.000000000000000000 ) ) ;
#19432 = CARTESIAN_POINT ( 'NONE',  ( -1.091055626815042645, 3.256072117181358472, 2.192599532798640283 ) ) ;
#19433 = VECTOR ( 'NONE', #34408, 39.37007874015748143 ) ;
#19434 = ORIENTED_EDGE ( 'NONE', *, *, #20009, .F. ) ;
#19435 = AXIS2_PLACEMENT_3D ( 'NONE', #1558, #45657, #1809 ) ;
#19436 = DIRECTION ( 'NONE',  ( 0.000000000000000000, 0.000000000000000000, -1.000000000000000000 ) ) ;
#19437 = ORIENTED_EDGE ( 'NONE', *, *, #3402, .F. ) ;
#19438 = ORIENTED_EDGE ( 'NONE', *, *, #23976, .T. ) ;
#19439 = CARTESIAN_POINT ( 'NONE',  ( 0.000000000000000000, 6.692913385826772199, 0.000000000000000000 ) ) ;
#19440 = CARTESIAN_POINT ( 'NONE',  ( 2.164823134740036625, 6.692913385826772199, -0.04796011690015051371 ) ) ;
#19441 = VECTOR ( 'NONE', #4380, 39.37007874015748143 ) ;
#19442 = DIRECTION ( 'NONE',  ( -0.000000000000000000, 1.000000000000000000, -0.000000000000000000 ) ) ;
#19443 = VECTOR ( 'NONE', #15072, 39.37007874015748143 ) ;
#19444 = PLANE ( 'NONE',  #8803 ) ;
#19445 = EDGE_CURVE ( 'NONE', #35668, #31067, #46025, .T. ) ;
#19446 = CARTESIAN_POINT ( 'NONE',  ( 0.1155636338427008941, -0.5222242541845523167, 0.000000000000000000 ) ) ;
#19447 = ORIENTED_EDGE ( 'NONE', *, *, #19307, .F. ) ;
#19448 = ORIENTED_EDGE ( 'NONE', *, *, #2853, .T. ) ;
#19449 = VECTOR ( 'NONE', #21354, 39.37007874015748143 ) ;
#19450 = B_SPLINE_CURVE_WITH_KNOTS ( 'NONE', 3,
 ( #20221, #32121, #47809, #4743 ),
 .UNSPECIFIED., .F., .F.,
 ( 4, 4 ),
 ( 2.018269040657474853E-07, 0.002500207291903820076 ),
 .UNSPECIFIED. ) ;
#19451 = B_SPLINE_CURVE_WITH_KNOTS ( 'NONE', 3,
 ( #5352, #16981, #13613, #40988 ),
 .UNSPECIFIED., .F., .F.,
 ( 4, 4 ),
 ( 0.0006212445558864886043, 0.003121509373039683521 ),
 .UNSPECIFIED. ) ;
#19452 = VERTEX_POINT ( 'NONE', #42917 ) ;
#19453 = LINE ( 'NONE', #27454, #7149 ) ;
#19454 = DIRECTION ( 'NONE',  ( -0.000000000000000000, 1.000000000000000000, -0.000000000000000000 ) ) ;
#19455 = EDGE_CURVE ( 'NONE', #34848, #42663, #6078, .T. ) ;
#19456 = CARTESIAN_POINT ( 'NONE',  ( -2.165354330708661568, 3.346456692913386100, -6.146657985744592735E-16 ) ) ;
#19457 = LINE ( 'NONE', #46058, #27816 ) ;
#19458 = ORIENTED_EDGE ( 'NONE', *, *, #11162, .T. ) ;
#19459 = CARTESIAN_POINT ( 'NONE',  ( -2.685185609606552060, 1.673311766001163825, -0.1698540269626902244 ) ) ;
#19460 = CARTESIAN_POINT ( 'NONE',  ( 1.836571684270173588, 0.01857023198900394079, 0.9324157793583920384 ) ) ;
#19461 = EDGE_CURVE ( 'NONE', #11818, #2547, #31317, .T. ) ;
#19462 = ORIENTED_EDGE ( 'NONE', *, *, #44012, .T. ) ;
#19463 = DIRECTION ( 'NONE',  ( -0.7071067811865481278, 0.7071067811865469066, -1.221861889385012670E-15 ) ) ;
#19464 = EDGE_CURVE ( 'NONE', #3461, #3180, #46692, .T. ) ;
#19465 = CARTESIAN_POINT ( 'NONE',  ( 1.833433833923351353, 3.267716535433071279, -1.259842519685035800 ) ) ;
#19466 = CARTESIAN_POINT ( 'NONE',  ( 0.2727639067037604392, 3.267716535433071279, -0.9842519685039348154 ) ) ;
#19468 = ADVANCED_FACE ( 'NONE', ( #39056 ), #12088, .T. ) ;
#19467 = ORIENTED_EDGE ( 'NONE', *, *, #44196, .F. ) ;
#19469 = VECTOR ( 'NONE', #19143, 39.37007874015748143 ) ;
#19470 = CARTESIAN_POINT ( 'NONE',  ( -0.2727639067037607723, 3.267716535433071279, -1.417322834645664331 ) ) ;
#19471 = CARTESIAN_POINT ( 'NONE',  ( -2.162130742952123263, 3.346456692913386100, 0.1181102362204704270 ) ) ;
#19472 = CARTESIAN_POINT ( 'NONE',  ( 2.592406080853238315, 1.455338980885439337, 1.413671649984625356 ) ) ;
#19473 = VECTOR ( 'NONE', #34353, 39.37007874015748143 ) ;
#19474 = VECTOR ( 'NONE', #44340, 39.37007874015748143 ) ;
#19475 = VERTEX_POINT ( 'NONE', #27175 ) ;
#19476 = PLANE ( 'NONE',  #42010 ) ;
#19477 = ORIENTED_EDGE ( 'NONE', *, *, #4587, .T. ) ;
#19478 = DIRECTION ( 'NONE',  ( 1.734723475976806848E-16, 0.000000000000000000, 1.000000000000000000 ) ) ;
#19479 = VECTOR ( 'NONE', #34686, 39.37007874015748143 ) ;
#19480 = DIRECTION ( 'NONE',  ( 1.000000000000000000, -0.000000000000000000, 0.000000000000000000 ) ) ;
#19481 = LINE ( 'NONE', #35244, #4576 ) ;
#19482 = CIRCLE ( 'NONE', #41755, 2.165354330708661568 ) ;
#19483 = AXIS2_PLACEMENT_3D ( 'NONE', #37104, #48666, #962 ) ;
#19484 = ORIENTED_EDGE ( 'NONE', *, *, #18043, .F. ) ;
#19485 = EDGE_LOOP ( 'NONE', ( #43588, #47346, #11802, #7044 ) ) ;
#19486 = CARTESIAN_POINT ( 'NONE',  ( 0.1968503937007874405, 3.267716535433071279, 0.000000000000000000 ) ) ;
#19487 = CARTESIAN_POINT ( 'NONE',  ( 1.736189279010248887, 0.03661913449923154956, 0.9901688781355542091 ) ) ;
#19488 = VERTEX_POINT ( 'NONE', #30809 ) ;
#19489 = CARTESIAN_POINT ( 'NONE',  ( -1.734268221780295827, 0.000000000000000000, 0.1852605408175444779 ) ) ;
#19490 = CARTESIAN_POINT ( 'NONE',  ( -0.5455278134075214336, 0.000000000000000000, 2.007874015748021268 ) ) ;
#19491 = EDGE_CURVE ( 'NONE', #28656, #29807, #23304, .T. ) ;
#19492 = DIRECTION ( 'NONE',  ( -1.000000000000000000, 0.000000000000000000, -0.000000000000000000 ) ) ;
#19493 = CARTESIAN_POINT ( 'NONE',  ( 1.015142113812069979, 3.267716535433071279, 1.417322834645662777 ) ) ;
#19494 = EDGE_LOOP ( 'NONE', ( #40256, #22363, #14944, #36696 ) ) ;
#19495 = ORIENTED_EDGE ( 'NONE', *, *, #29061, .F. ) ;
#19496 = CARTESIAN_POINT ( 'NONE',  ( -2.721588301589615622, 1.578403504144545888, -1.145422913280063071 ) ) ;
#19497 = EDGE_CURVE ( 'NONE', #13500, #7335, #43428, .T. ) ;
#19498 = EDGE_CURVE ( 'NONE', #38358, #41084, #19421, .T. ) ;
#19499 = LINE ( 'NONE', #8149, #28984 ) ;
#19500 = ORIENTED_EDGE ( 'NONE', *, *, #35245, .T. ) ;
#19501 = EDGE_CURVE ( 'NONE', #27924, #12064, #15809, .T. ) ;
#19502 = DIRECTION ( 'NONE',  ( 3.986037398843765983E-20, 1.000000000000000000, 1.160734090543304660E-16 ) ) ;
#19503 = EDGE_LOOP ( 'NONE', ( #1971, #30394, #27280, #5374, #35932, #7693, #26067, #26048 ) ) ;
#19504 = VERTEX_POINT ( 'NONE', #39567 ) ;
#19505 = CARTESIAN_POINT ( 'NONE',  ( -3.414809992080329023E-17, 3.267716535433071279, -0.1968503937007874405 ) ) ;
#19506 = VECTOR ( 'NONE', #39413, 39.37007874015748143 ) ;
#19507 = ORIENTED_EDGE ( 'NONE', *, *, #42291, .T. ) ;
#19508 = VERTEX_POINT ( 'NONE', #7568 ) ;
#19509 = DIRECTION ( 'NONE',  ( -0.000000000000000000, 1.000000000000000000, -0.000000000000000000 ) ) ;
#19510 = VERTEX_POINT ( 'NONE', #23556 ) ;
#19511 = CONICAL_SURFACE ( 'NONE', #26122, 2.089297179032357121, 0.2617993877991570129 ) ;
#19512 = DIRECTION ( 'NONE',  ( -0.000000000000000000, 1.000000000000000000, -0.000000000000000000 ) ) ;
#19513 = DIRECTION ( 'NONE',  ( -0.8805955318567391110, 0.000000000000000000, 0.4738686624729965269 ) ) ;
#19514 = DIRECTION ( 'NONE',  ( 0.000000000000000000, 0.000000000000000000, -1.000000000000000000 ) ) ;
#19515 = VECTOR ( 'NONE', #28723, 39.37007874015748854 ) ;
#19516 = CARTESIAN_POINT ( 'NONE',  ( -1.198202975868768005, 3.267716535433071279, 1.732283464566920950 ) ) ;
#19517 = VECTOR ( 'NONE', #24139, 39.37007874015748143 ) ;
#19518 = LINE ( 'NONE', #50963, #28618 ) ;
#19519 = CARTESIAN_POINT ( 'NONE',  ( 1.363819533518803251, 0.000000000000000000, 1.417322834645662777 ) ) ;
#19520 = ORIENTED_EDGE ( 'NONE', *, *, #13771, .T. ) ;
#19521 = DIRECTION ( 'NONE',  ( 1.000000000000000000, -0.000000000000000000, 0.000000000000000000 ) ) ;
#19522 = CARTESIAN_POINT ( 'NONE',  ( -2.295914061060153610, 1.576889242737733676, 0.7977328874972187123 ) ) ;
#19523 = CARTESIAN_POINT ( 'NONE',  ( 0.000000000000000000, 3.267716535433071279, 2.047244094488179567 ) ) ;
#19524 = ORIENTED_EDGE ( 'NONE', *, *, #4519, .F. ) ;
#19525 = CARTESIAN_POINT ( 'NONE',  ( -0.1324246528408225543, 1.049866565877817681, -2.020365292430061022 ) ) ;
#19526 = ADVANCED_FACE ( 'NONE', ( #14813 ), #46523, .F. ) ;
#19527 = DIRECTION ( 'NONE',  ( 1.000000000000000000, 0.000000000000000000, -3.469446951953613696E-16 ) ) ;
#19528 = EDGE_LOOP ( 'NONE', ( #14046, #40050, #41308, #13962 ) ) ;
#19529 = CARTESIAN_POINT ( 'NONE',  ( 0.2727639067037602172, 3.267716535433071279, -1.929133858267710000 ) ) ;
#19530 = FACE_OUTER_BOUND ( 'NONE', #45533, .T. ) ;
#19531 = ADVANCED_FACE ( 'NONE', ( #19926 ), #37688, .T. ) ;
#19532 = FACE_OUTER_BOUND ( 'NONE', #33171, .T. ) ;
#19533 = VERTEX_POINT ( 'NONE', #38813 ) ;
#19534 = CARTESIAN_POINT ( 'NONE',  ( -2.151809081513409438, 1.673437530708463017, 0.2418202932658340965 ) ) ;
#19535 = DIRECTION ( 'NONE',  ( 0.9998717552508121775, 0.01601477604151182663, 0.000000000000000000 ) ) ;
#19536 = DIRECTION ( 'NONE',  ( -0.3090169943749447867, -1.160734090543305153E-16, -0.9510565162951545304 ) ) ;
#19537 = CARTESIAN_POINT ( 'NONE',  ( -1.037524086854360261, 5.905511811023623991, 2.764473043227569260 ) ) ;
#19538 = VERTEX_POINT ( 'NONE', #50370 ) ;
#19539 = VECTOR ( 'NONE', #29130, 39.37007874015748143 ) ;
#19540 = VECTOR ( 'NONE', #18474, 39.37007874015748143 ) ;
#19541 = AXIS2_PLACEMENT_3D ( 'NONE', #34715, #30841, #46552 ) ;
#19542 = ORIENTED_EDGE ( 'NONE', *, *, #46770, .T. ) ;
#19543 = ORIENTED_EDGE ( 'NONE', *, *, #19778, .F. ) ;
#19544 = CARTESIAN_POINT ( 'NONE',  ( 2.734482843737263025, 1.761870738172414796, -1.115254632218672493 ) ) ;
#19545 = VERTEX_POINT ( 'NONE', #3948 ) ;
#19546 = DIRECTION ( 'NONE',  ( -0.000000000000000000, 1.000000000000000000, -0.000000000000000000 ) ) ;
#19547 = EDGE_CURVE ( 'NONE', #17945, #4326, #19680, .T. ) ;
#19548 = CARTESIAN_POINT ( 'NONE',  ( -1.636583440222563635, 0.000000000000000000, 0.3149606299212578953 ) ) ;
#19549 = EDGE_LOOP ( 'NONE', ( #15252, #17598, #41474, #22503 ) ) ;
#19550 = FACE_OUTER_BOUND ( 'NONE', #9719, .T. ) ;
#19551 = EDGE_CURVE ( 'NONE', #1805, #7241, #493, .T. ) ;
#19552 = EDGE_LOOP ( 'NONE', ( #47274, #33574, #11698, #32176 ) ) ;
#19553 = CARTESIAN_POINT ( 'NONE',  ( -0.8942052331142547050, 3.346456692913386100, 1.377952755905504256 ) ) ;
#19554 = CARTESIAN_POINT ( 'NONE',  ( -1.567214440306964107, 0.002817858044914879883, 0.7874684655159520652 ) ) ;
#19555 = EDGE_LOOP ( 'NONE', ( #21533, #1332, #10348, #12321 ) ) ;
#19556 = VERTEX_POINT ( 'NONE', #19174 ) ;
#19557 = ADVANCED_FACE ( 'NONE', ( #10933 ), #16220, .T. ) ;
#19558 = CARTESIAN_POINT ( 'NONE',  ( 0.07982360342473591996, 1.709180471932028711, 0.000000000000000000 ) ) ;
#19559 = ORIENTED_EDGE ( 'NONE', *, *, #3877, .F. ) ;
#19560 = VECTOR ( 'NONE', #30646, 39.37007874015748143 ) ;
#19561 = PLANE ( 'NONE',  #13056 ) ;
#19562 = VERTEX_POINT ( 'NONE', #26674 ) ;
#19563 = ORIENTED_EDGE ( 'NONE', *, *, #50630, .T. ) ;
#19564 = CARTESIAN_POINT ( 'NONE',  ( 0.9360721529196784907, 0.000000000000000000, 1.470771056236116481 ) ) ;
#19565 = LINE ( 'NONE', #25185, #9741 ) ;
#19566 = VERTEX_POINT ( 'NONE', #22812 ) ;
#19567 = CARTESIAN_POINT ( 'NONE',  ( -1.091055626815042645, 0.000000000000000000, -0.8267716535433052849 ) ) ;
#19568 = ORIENTED_EDGE ( 'NONE', *, *, #815, .F. ) ;
#19569 = CARTESIAN_POINT ( 'NONE',  ( 0.000000000000000000, 1.574803149606302854, 0.000000000000000000 ) ) ;
#19570 = DIRECTION ( 'NONE',  ( 0.000000000000000000, -1.000000000000000000, 0.000000000000000000 ) ) ;
#19571 = VECTOR ( 'NONE', #3741, 39.37007874015748143 ) ;
#19572 = VECTOR ( 'NONE', #4689, 39.37007874015748854 ) ;
#19573 = CARTESIAN_POINT ( 'NONE',  ( -1.461363083917493588, 1.574803149606302854, 1.597866488315563327 ) ) ;
#19574 = EDGE_LOOP ( 'NONE', ( #5002, #16017, #31114, #49856 ) ) ;
#19575 = ORIENTED_EDGE ( 'NONE', *, *, #23462, .F. ) ;
#19576 = DIRECTION ( 'NONE',  ( -1.000000000000000000, 0.000000000000000000, 1.734723475976806848E-16 ) ) ;
#19577 = CARTESIAN_POINT ( 'NONE',  ( 1.091055626815042423, 3.346456692913386100, -1.259842519685035134 ) ) ;
#19578 = CARTESIAN_POINT ( 'NONE',  ( -0.7322040776173250887, 1.028380827711104617, -2.468097745819289646 ) ) ;
#19579 = VECTOR ( 'NONE', #2, 39.37007874015748143 ) ;
#19580 = LINE ( 'NONE', #39214, #12826 ) ;
#19581 = CARTESIAN_POINT ( 'NONE',  ( 1.909347346926324684, 0.000000000000000000, -0.3543307086614178592 ) ) ;
#19582 = FACE_OUTER_BOUND ( 'NONE', #41558, .T. ) ;
#19583 = VERTEX_POINT ( 'NONE', #18936 ) ;
#19584 = CARTESIAN_POINT ( 'NONE',  ( 0.5455278134075216556, 3.267716535433071279, 1.692913385826762873 ) ) ;
#19585 = AXIS2_PLACEMENT_3D ( 'NONE', #38946, #14948, #7453 ) ;
#19586 = ADVANCED_FACE ( 'NONE', ( #26925 ), #42672, .F. ) ;
#19587 = EDGE_LOOP ( 'NONE', ( #17114, #3796, #34906, #21544 ) ) ;
#19588 = DIRECTION ( 'NONE',  ( -3.986037398843765983E-20, -1.000000000000000000, -1.160734090543304660E-16 ) ) ;
#19589 = EDGE_CURVE ( 'NONE', #39559, #46927, #28704, .T. ) ;
#19590 = VECTOR ( 'NONE', #3473, 39.37007874015748143 ) ;
#19591 = EDGE_LOOP ( 'NONE', ( #41178, #32573, #42674, #2348 ) ) ;
#19592 = EDGE_CURVE ( 'NONE', #23176, #40104, #16330, .T. ) ;
#19593 = DIRECTION ( 'NONE',  ( 0.000000000000000000, 0.7660444431189770143, 0.6427876096865403621 ) ) ;
#19594 = LINE ( 'NONE', #23472, #50846 ) ;
#19595 = VERTEX_POINT ( 'NONE', #39818 ) ;
#19596 = EDGE_CURVE ( 'NONE', #456, #26189, #32091, .T. ) ;
#19597 = CARTESIAN_POINT ( 'NONE',  ( 0.1968503937007870241, 0.000000000000000000, -1.889763779527552146 ) ) ;
#19598 = B_SPLINE_CURVE_WITH_KNOTS ( 'NONE', 3,
 ( #41764, #41509, #6401, #2525 ),
 .UNSPECIFIED., .F., .F.,
 ( 4, 4 ),
 ( 2.003042186605898400E-07, 0.01598066055596613841 ),
 .UNSPECIFIED. ) ;
#19599 = ORIENTED_EDGE ( 'NONE', *, *, #28356, .T. ) ;
#19600 = DIRECTION ( 'NONE',  ( -1.000000000000000000, 0.000000000000000000, 1.734723475976806848E-16 ) ) ;
#19601 = ORIENTED_EDGE ( 'NONE', *, *, #47470, .T. ) ;
#19602 = PLANE ( 'NONE',  #26054 ) ;
#19603 = CARTESIAN_POINT ( 'NONE',  ( 0.000000000000000000, 3.267716535433071279, -1.732283464566923170 ) ) ;
#19604 = EDGE_CURVE ( 'NONE', #21767, #15175, #35612, .T. ) ;
#19605 = VECTOR ( 'NONE', #47648, 39.37007874015748143 ) ;
#19606 = AXIS2_PLACEMENT_3D ( 'NONE', #29906, #30924, #27029 ) ;
#19607 = ORIENTED_EDGE ( 'NONE', *, *, #23745, .F. ) ;
#19608 = CARTESIAN_POINT ( 'NONE',  ( 0.1197526584096238467, 0.01986475091724364955, -1.879567902740797436 ) ) ;
#19609 = EDGE_LOOP ( 'NONE', ( #1392, #20449, #48228, #41883 ) ) ;
#19610 = ORIENTED_EDGE ( 'NONE', *, *, #29369, .T. ) ;
#19611 = ADVANCED_FACE ( 'NONE', ( #4454 ), #4962, .F. ) ;
#19612 = CARTESIAN_POINT ( 'NONE',  ( 0.000000000000000000, 3.346456692913386100, 0.000000000000000000 ) ) ;
#19613 = CARTESIAN_POINT ( 'NONE',  ( -1.712496953225537633, 3.346456692913386100, 1.417322834645662333 ) ) ;
#19614 = CARTESIAN_POINT ( 'NONE',  ( -0.3486774197067339376, 3.346456692913386100, 2.204724409448808764 ) ) ;
#19615 = VECTOR ( 'NONE', #25940, 39.37007874015748143 ) ;
#19616 = VERTEX_POINT ( 'NONE', #20189 ) ;
#19617 = VECTOR ( 'NONE', #50542, 39.37007874015748143 ) ;
#19618 = LINE ( 'NONE', #30750, #19579 ) ;
#19619 = CARTESIAN_POINT ( 'NONE',  ( -1.528548437409730454, 1.695430332713048882, 2.526376101461759838 ) ) ;
#19620 = ORIENTED_EDGE ( 'NONE', *, *, #4908, .F. ) ;
#19621 = VECTOR ( 'NONE', #26755, 39.37007874015748143 ) ;
#19622 = DIRECTION ( 'NONE',  ( -0.000000000000000000, 1.000000000000000000, -0.000000000000000000 ) ) ;
#19623 = ORIENTED_EDGE ( 'NONE', *, *, #29759, .F. ) ;
#19624 = ORIENTED_EDGE ( 'NONE', *, *, #29656, .F. ) ;
#19625 = AXIS2_PLACEMENT_3D ( 'NONE', #42884, #30777, #31287 ) ;
#19626 = EDGE_CURVE ( 'NONE', #37726, #11359, #8327, .T. ) ;
#19627 = EDGE_LOOP ( 'NONE', ( #1937, #32321, #48950 ) ) ;
#19628 = CARTESIAN_POINT ( 'NONE',  ( -0.5286458662987743029, 0.000000000000000000, 2.100489422084707680 ) ) ;
#19629 = DIRECTION ( 'NONE',  ( -0.8805955318567391110, -5.496845023002422681E-17, 0.4738686624729965269 ) ) ;
#19630 = CARTESIAN_POINT ( 'NONE',  ( 0.8182917201112819283, 0.000000000000000000, -0.3543307086614175816 ) ) ;
#19631 = DIRECTION ( 'NONE',  ( 0.000000000000000000, 0.000000000000000000, 1.000000000000000000 ) ) ;
#19632 = ORIENTED_EDGE ( 'NONE', *, *, #33029, .F. ) ;
#19633 = ORIENTED_EDGE ( 'NONE', *, *, #26298, .T. ) ;
#19634 = CARTESIAN_POINT ( 'NONE',  ( -1.536664496436148184E-16, 3.267716535433071279, -0.8267716535433052849 ) ) ;
#19635 = PLANE ( 'NONE',  #40800 ) ;
#19636 = ORIENTED_EDGE ( 'NONE', *, *, #19946, .F. ) ;
#19637 = DIRECTION ( 'NONE',  ( -0.000000000000000000, 1.000000000000000000, -0.000000000000000000 ) ) ;
#19638 = CARTESIAN_POINT ( 'NONE',  ( 0.000000000000000000, 3.267716535433071279, 1.732283464566921172 ) ) ;
#19639 = CARTESIAN_POINT ( 'NONE',  ( -1.556712866041156440, 1.596563264426776207, 2.509548638715847435 ) ) ;
#19640 = VECTOR ( 'NONE', #182, 39.37007874015748143 ) ;
#19641 = DIRECTION ( 'NONE',  ( 0.000000000000000000, -1.000000000000000000, 0.000000000000000000 ) ) ;
#19642 = PLANE ( 'NONE',  #8757 ) ;
#19643 = CARTESIAN_POINT ( 'NONE',  ( 0.07982360342473591996, 1.709180471932028711, 0.000000000000000000 ) ) ;
#19644 = ORIENTED_EDGE ( 'NONE', *, *, #11674, .T. ) ;
#19645 = FACE_OUTER_BOUND ( 'NONE', #17609, .T. ) ;
#19646 = LINE ( 'NONE', #35416, #32665 ) ;
#19647 = EDGE_CURVE ( 'NONE', #20944, #16575, #42999, .T. ) ;
#19648 = AXIS2_PLACEMENT_3D ( 'NONE', #40775, #1270, #48219 ) ;
#19649 = EDGE_LOOP ( 'NONE', ( #4946, #15693, #29560, #17786 ) ) ;
#19650 = EDGE_CURVE ( 'NONE', #6147, #33328, #24842, .T. ) ;
#19651 = ORIENTED_EDGE ( 'NONE', *, *, #1199, .F. ) ;
#19652 = CLOSED_SHELL ( 'NONE', ( #10713, #3166, #31550, #44419, #13980, #49978, #501, #42388, #36409, #42149, #42895, #23224, #12290, #17117, #18858, #46186, #5412, #25873, #3710, #21950, #6891, #8848, #37924, #28188, #21650, #17648, #11691, #19969, #16235 ) ) ;
#19653 = DIRECTION ( 'NONE',  ( -3.986037398843765983E-20, -1.000000000000000000, -1.160734090543304660E-16 ) ) ;
#19654 = FACE_OUTER_BOUND ( 'NONE', #27164, .T. ) ;
#19655 = DIRECTION ( 'NONE',  ( 0.000000000000000000, 0.000000000000000000, -1.000000000000000000 ) ) ;
#19656 = EDGE_CURVE ( 'NONE', #50585, #48785, #12451, .T. ) ;
#19657 = VERTEX_POINT ( 'NONE', #20706 ) ;
#19658 = EDGE_CURVE ( 'NONE', #358, #50651, #40078, .T. ) ;
#19659 = COLOUR_RGB ( '',0.7921568627450980005, 0.8196078431372548767, 0.9333333333333333481 ) ;
#19660 = ORIENTED_EDGE ( 'NONE', *, *, #28837, .T. ) ;
#19661 = FACE_OUTER_BOUND ( 'NONE', #2099, .T. ) ;
#19662 = ORIENTED_EDGE ( 'NONE', *, *, #44627, .T. ) ;
#19663 = AXIS2_PLACEMENT_3D ( 'NONE', #28814, #48647, #24442 ) ;
#19664 = DIRECTION ( 'NONE',  ( -1.000000000000000000, -0.000000000000000000, -0.000000000000000000 ) ) ;
#19665 = ORIENTED_EDGE ( 'NONE', *, *, #18960, .F. ) ;
#19666 = CARTESIAN_POINT ( 'NONE',  ( -1.022258465722730714, 1.597063495466063188, -2.236165044959671278 ) ) ;
#19667 = CARTESIAN_POINT ( 'NONE',  ( -2.823445274216743073, 1.675250974312822105, 0.8656477926280276014 ) ) ;
#19668 = CARTESIAN_POINT ( 'NONE',  ( 2.160407304981128984, 5.905511811023623991, -0.1462862061266579361 ) ) ;
#19669 = EDGE_CURVE ( 'NONE', #10859, #34607, #4714, .T. ) ;
#19670 = ORIENTED_EDGE ( 'NONE', *, *, #20108, .F. ) ;
#19671 = EDGE_LOOP ( 'NONE', ( #27535, #19015, #38058, #32747 ) ) ;
#19672 = ORIENTED_EDGE ( 'NONE', *, *, #30910, .F. ) ;
#19673 = LINE ( 'NONE', #9281, #19105 ) ;
#19674 = DIRECTION ( 'NONE',  ( -1.000000000000000000, 0.000000000000000000, 0.000000000000000000 ) ) ;
#19675 = ORIENTED_EDGE ( 'NONE', *, *, #18560, .F. ) ;
#19676 = EDGE_LOOP ( 'NONE', ( #13440, #33132, #46346, #44578 ) ) ;
#19677 = ADVANCED_FACE ( 'NONE', ( #1085 ), #35931, .T. ) ;
#19678 = DIRECTION ( 'NONE',  ( -1.000000000000000000, 0.000000000000000000, 1.734723475976806848E-16 ) ) ;
#19679 = CARTESIAN_POINT ( 'NONE',  ( 0.000000000000000000, 0.000000000000000000, 0.000000000000000000 ) ) ;
#19680 = LINE ( 'NONE', #27427, #48317 ) ;
#19681 = ORIENTED_EDGE ( 'NONE', *, *, #5565, .T. ) ;
#19682 = VERTEX_POINT ( 'NONE', #28191 ) ;
#19683 = CARTESIAN_POINT ( 'NONE',  ( 1.015142113812069091, 3.267716535433071279, -1.417322834645664331 ) ) ;
#19684 = CARTESIAN_POINT ( 'NONE',  ( 0.4788131938641112528, 1.726726173772622941, 2.914091152102192162 ) ) ;
#19685 = VECTOR ( 'NONE', #16653, 39.37007874015748143 ) ;
#19686 = EDGE_CURVE ( 'NONE', #13474, #2075, #43933, .T. ) ;
#19687 = CARTESIAN_POINT ( 'NONE',  ( 0.2727639067037604947, 0.000000000000000000, -0.4724409448818886470 ) ) ;
#19688 = VERTEX_POINT ( 'NONE', #5214 ) ;
#19689 =( NAMED_UNIT ( * ) PLANE_ANGLE_UNIT ( ) SI_UNIT ( $, .RADIAN. ) );
#19690 = LINE ( 'NONE', #35454, #40101 ) ;
#19691 = VERTEX_POINT ( 'NONE', #25097 ) ;
#19692 = CARTESIAN_POINT ( 'NONE',  ( 2.950518648759406393, 1.666751258392789259, -0.1160872037100129095 ) ) ;
#19693 = ORIENTED_EDGE ( 'NONE', *, *, #47232, .F. ) ;
#19694 = VERTEX_POINT ( 'NONE', #36212 ) ;
#19695 = CARTESIAN_POINT ( 'NONE',  ( 0.8182917201112819283, 3.346456692913386100, -0.1574803149606301411 ) ) ;
#19696 = DIRECTION ( 'NONE',  ( 0.000000000000000000, -1.000000000000000000, 0.000000000000000000 ) ) ;
#19697 = EDGE_CURVE ( 'NONE', #49795, #20976, #28192, .T. ) ;
#19698 = VECTOR ( 'NONE', #21806, 39.37007874015748143 ) ;
#19699 = VECTOR ( 'NONE', #33390, 39.37007874015748143 ) ;
#19700 = FACE_OUTER_BOUND ( 'NONE', #45630, .T. ) ;
#19701 = LINE ( 'NONE', #27701, #22852 ) ;
#19703 = CARTESIAN_POINT ( 'NONE',  ( 0.7423782071083087075, 3.346456692913386100, -0.3149606299212593941 ) ) ;
#19702 = AXIS2_PLACEMENT_3D ( 'NONE', #6767, #49830, #26632 ) ;
#19704 = ORIENTED_EDGE ( 'NONE', *, *, #3933, .F. ) ;
#19705 = ORIENTED_EDGE ( 'NONE', *, *, #47490, .F. ) ;
#19706 = EDGE_CURVE ( 'NONE', #6435, #20003, #20968, .T. ) ;
#19707 = AXIS2_PLACEMENT_3D ( 'NONE', #22033, #29258, #2413 ) ;
#19708 = ORIENTED_EDGE ( 'NONE', *, *, #17551, .T. ) ;
#19709 = LINE ( 'NONE', #35721, #46684 ) ;
#19710 = CARTESIAN_POINT ( 'NONE',  ( 0.1968503937007872462, 3.346456692913386100, -1.771653543307081025 ) ) ;
#19711 = EDGE_CURVE ( 'NONE', #42971, #6865, #50685, .T. ) ;
#19712 = LINE ( 'NONE', #43196, #21964 ) ;
#19713 = DIRECTION ( 'NONE',  ( 1.734723475976806848E-16, -0.000000000000000000, 1.000000000000000000 ) ) ;
#19714 = ORIENTED_EDGE ( 'NONE', *, *, #50437, .T. ) ;
#19715 = CARTESIAN_POINT ( 'NONE',  ( 0.7423782071083087075, 0.000000000000000000, 0.9448818897637746295 ) ) ;
#19716 = CARTESIAN_POINT ( 'NONE',  ( -0.3486774197067339376, 0.000000000000000000, 2.204724409448808764 ) ) ;
#19717 = EDGE_CURVE ( 'NONE', #39129, #25030, #320, .T. ) ;
#19718 = EDGE_LOOP ( 'NONE', ( #33993, #31060, #49789, #6639 ) ) ;
#19719 = CARTESIAN_POINT ( 'NONE',  ( 0.000000000000000000, 6.692913385826772199, 0.000000000000000000 ) ) ;
#19720 = LINE ( 'NONE', #36254, #10500 ) ;
#19721 = DIRECTION ( 'NONE',  ( -0.9998717552508121775, -0.01601477604151182316, 0.000000000000000000 ) ) ;
#19722 = VECTOR ( 'NONE', #18620, 39.37007874015748143 ) ;
#19723 = ORIENTED_EDGE ( 'NONE', *, *, #41500, .T. ) ;
#19724 = CARTESIAN_POINT ( 'NONE',  ( 1.363819533518803473, 3.267716535433071279, -2.365849761790805980E-16 ) ) ;
#19725 = FACE_OUTER_BOUND ( 'NONE', #43447, .T. ) ;
#19726 = EDGE_CURVE ( 'NONE', #5813, #49431, #14495, .T. ) ;
#19727 = LINE ( 'NONE', #43977, #43168 ) ;
#19728 = ORIENTED_EDGE ( 'NONE', *, *, #2705, .T. ) ;
#19729 = LINE ( 'NONE', #15855, #34574 ) ;
#19730 = ORIENTED_EDGE ( 'NONE', *, *, #2340, .F. ) ;
#19731 = DIRECTION ( 'NONE',  ( -1.000000000000000000, 0.000000000000000000, 1.734723475976806848E-16 ) ) ;
#19732 = AXIS2_PLACEMENT_3D ( 'NONE', #14253, #30261, #37256 ) ;
#19733 = DIRECTION ( 'NONE',  ( 1.000000000000000000, 0.000000000000000000, 0.000000000000000000 ) ) ;
#19734 = DIRECTION ( 'NONE',  ( -0.01601477604151182663, 0.9998717552508123996, -0.000000000000000000 ) ) ;
#19735 = DIRECTION ( 'NONE',  ( -0.000000000000000000, 0.000000000000000000, 1.000000000000000000 ) ) ;
#19736 = ORIENTED_EDGE ( 'NONE', *, *, #8783, .F. ) ;
#19737 = ORIENTED_EDGE ( 'NONE', *, *, #48073, .F. ) ;
#19738 = LINE ( 'NONE', #40407, #36412 ) ;
#19739 = FACE_OUTER_BOUND ( 'NONE', #44730, .T. ) ;
#19740 = ORIENTED_EDGE ( 'NONE', *, *, #9702, .F. ) ;
#19741 = DIRECTION ( 'NONE',  ( -0.000000000000000000, 1.000000000000000000, -0.000000000000000000 ) ) ;
#19742 = LINE ( 'NONE', #30370, #30986 ) ;
#19743 = VECTOR ( 'NONE', #42539, 39.37007874015748143 ) ;
#19744 = CARTESIAN_POINT ( 'NONE',  ( 0.1968503937007878568, 3.267716535433071279, 2.156388021673882438 ) ) ;
#19745 = CARTESIAN_POINT ( 'NONE',  ( 1.556712866041120247, 1.645058926882370542, 2.509548638715870084 ) ) ;
#19746 = EDGE_LOOP ( 'NONE', ( #35291, #26851, #32639, #35826 ) ) ;
#19747 = ORIENTED_EDGE ( 'NONE', *, *, #14329, .T. ) ;
#19748 = DIRECTION ( 'NONE',  ( -0.9510565162951500895, 3.590656546124792943E-17, -0.3090169943749582204 ) ) ;
#19749 = EDGE_CURVE ( 'NONE', #31800, #8483, #6243, .T. ) ;
#19750 = DIRECTION ( 'NONE',  ( 1.734723475976806848E-16, -0.000000000000000000, 1.000000000000000000 ) ) ;
#19751 = ORIENTED_EDGE ( 'NONE', *, *, #2882, .F. ) ;
#19752 = CIRCLE ( 'NONE', #2311, 2.106299212598425008 ) ;
#19753 = CARTESIAN_POINT ( 'NONE',  ( 0.2156353639037333347, 0.03137346048107473445, -1.846898229409209558 ) ) ;
#19754 = VERTEX_POINT ( 'NONE', #1602 ) ;
#19755 = ORIENTED_EDGE ( 'NONE', *, *, #33370, .T. ) ;
#19756 = DIRECTION ( 'NONE',  ( 0.000000000000000000, 0.000000000000000000, -1.000000000000000000 ) ) ;
#19757 = EDGE_CURVE ( 'NONE', #32113, #2736, #9606, .T. ) ;
#19758 = EDGE_CURVE ( 'NONE', #50824, #40528, #10623, .T. ) ;
#19759 = VECTOR ( 'NONE', #34059, 39.37007874015748143 ) ;
#19760 = EDGE_CURVE ( 'NONE', #45138, #31969, #16504, .T. ) ;
#19761 = EDGE_LOOP ( 'NONE', ( #21113, #19448, #49463, #8129 ) ) ;
#19762 = ORIENTED_EDGE ( 'NONE', *, *, #31034, .F. ) ;
#19763 = CARTESIAN_POINT ( 'NONE',  ( 1.636583440222563635, 3.346456692913386100, -1.141732283464564013 ) ) ;
#19764 = VERTEX_POINT ( 'NONE', #37747 ) ;
#19765 = EDGE_CURVE ( 'NONE', #48962, #30043, #37236, .T. ) ;
#19766 = DIRECTION ( 'NONE',  ( 1.160706738777435820E-16, 1.000000000000000000, 5.589669052740852391E-17 ) ) ;
#19767 = DIRECTION ( 'NONE',  ( -0.000000000000000000, 0.000000000000000000, 1.000000000000000000 ) ) ;
#19768 = LINE ( 'NONE', #12809, #7758 ) ;
#19769 = VECTOR ( 'NONE', #33260, 39.37007874015748143 ) ;
#19770 = DIRECTION ( 'NONE',  ( 1.734723475976806848E-16, -0.000000000000000000, 1.000000000000000000 ) ) ;
#19771 = CARTESIAN_POINT ( 'NONE',  ( 0.08139965876239094178, 1.610780518492231694, 0.000000000000000000 ) ) ;
#19772 = CARTESIAN_POINT ( 'NONE',  ( 0.3880746611937324064, 0.02269246980704499317, 1.862854658644473638 ) ) ;
#19773 = ORIENTED_EDGE ( 'NONE', *, *, #42528, .T. ) ;
#19774 = DIRECTION ( 'NONE',  ( -0.000000000000000000, 1.000000000000000000, -0.000000000000000000 ) ) ;
#19775 = AXIS2_PLACEMENT_3D ( 'NONE', #30488, #21982, #10857 ) ;
#19776 = CARTESIAN_POINT ( 'NONE',  ( 0.7406773873160164001, 0.5226447100659409317, 2.113585110334742279 ) ) ;
#19777 = DIRECTION ( 'NONE',  ( 1.000000000000000000, 0.000000000000000000, -3.469446951953613696E-16 ) ) ;
#19778 = EDGE_CURVE ( 'NONE', #7505, #36292, #49558, .T. ) ;
#19779 = ORIENTED_EDGE ( 'NONE', *, *, #7759, .F. ) ;
#19780 = CARTESIAN_POINT ( 'NONE',  ( 0.4696143004045479352, 3.267716535433071279, 0.7874015748031454320 ) ) ;
#19781 = DIRECTION ( 'NONE',  ( 0.9959742939952384022, 0.000000000000000000, 0.08963930890344089242 ) ) ;
#19782 = EDGE_LOOP ( 'NONE', ( #15565, #18223, #8847, #13940 ) ) ;
#19783 = CARTESIAN_POINT ( 'NONE',  ( 0.5455278134075212115, 0.000000000000000000, -1.259842519685035134 ) ) ;
#19784 = CARTESIAN_POINT ( 'NONE',  ( -1.472219874544909768, 1.546549606962118517, 2.560030851058948898 ) ) ;
#19785 = ADVANCED_FACE ( 'NONE', ( #1856 ), #48797, .F. ) ;
#19786 = CARTESIAN_POINT ( 'NONE',  ( -0.5455278134075214336, 3.267716535433071279, 2.204724409448808764 ) ) ;
#19787 = DIRECTION ( 'NONE',  ( -3.986037398843765983E-20, -1.000000000000000000, -1.160734090543304660E-16 ) ) ;
#19788 = VERTEX_POINT ( 'NONE', #33117 ) ;
#19789 = LINE ( 'NONE', #39934, #15721 ) ;
#19790 = DIRECTION ( 'NONE',  ( -0.000000000000000000, 1.000000000000000000, -0.000000000000000000 ) ) ;
#19791 = DIRECTION ( 'NONE',  ( 1.000000000000000000, -0.000000000000000000, 0.000000000000000000 ) ) ;
#19792 = DIRECTION ( 'NONE',  ( 0.000000000000000000, 1.000000000000000000, 0.000000000000000000 ) ) ;
#19793 = ORIENTED_EDGE ( 'NONE', *, *, #8020, .F. ) ;
#19794 = ORIENTED_EDGE ( 'NONE', *, *, #33712, .F. ) ;
#19795 = ORIENTED_EDGE ( 'NONE', *, *, #6030, .F. ) ;
#19796 = LINE ( 'NONE', #23682, #32017 ) ;
#19797 = ORIENTED_EDGE ( 'NONE', *, *, #23166, .T. ) ;
#19798 = DIRECTION ( 'NONE',  ( 0.000000000000000000, -1.000000000000000000, 0.000000000000000000 ) ) ;
#19799 = DIRECTION ( 'NONE',  ( -0.000000000000000000, 1.000000000000000000, -0.000000000000000000 ) ) ;
#19800 = VERTEX_POINT ( 'NONE', #29217 ) ;
#19801 = AXIS2_PLACEMENT_3D ( 'NONE', #28802, #8932, #48383 ) ;
#19802 = DIRECTION ( 'NONE',  ( -0.000000000000000000, 0.000000000000000000, 1.000000000000000000 ) ) ;
#19803 = VECTOR ( 'NONE', #14005, 39.37007874015748143 ) ;
#19804 = ORIENTED_EDGE ( 'NONE', *, *, #18005, .F. ) ;
#19805 = LINE ( 'NONE', #15188, #14218 ) ;
#19806 = DIRECTION ( 'NONE',  ( 0.000000000000000000, 0.000000000000000000, 1.000000000000000000 ) ) ;
#19807 = ORIENTED_EDGE ( 'NONE', *, *, #15275, .T. ) ;
#19808 = ORIENTED_EDGE ( 'NONE', *, *, #21473, .T. ) ;
#19809 = CARTESIAN_POINT ( 'NONE',  ( 0.5455278134075211005, 3.267716535433071279, -9.463399047163218249E-17 ) ) ;
#19810 = VERTEX_POINT ( 'NONE', #18368 ) ;
#19811 = AXIS2_PLACEMENT_3D ( 'NONE', #11062, #29672, #41291 ) ;
#19812 = CARTESIAN_POINT ( 'NONE',  ( -1.091055626815042201, 0.000000000000000000, 1.259842519685033357 ) ) ;
#19813 = EDGE_CURVE ( 'NONE', #31004, #9761, #10113, .T. ) ;
#19814 = EDGE_CURVE ( 'NONE', #37232, #15390, #49810, .T. ) ;
#19815 = ORIENTED_EDGE ( 'NONE', *, *, #14796, .F. ) ;
#19816 = ORIENTED_EDGE ( 'NONE', *, *, #38582, .F. ) ;
#19817 = DIRECTION ( 'NONE',  ( 1.000000000000000000, 0.000000000000000000, 0.000000000000000000 ) ) ;
#19818 = ADVANCED_FACE ( 'NONE', ( #49052 ), #29731, .F. ) ;
#19819 = CARTESIAN_POINT ( 'NONE',  ( 0.000000000000000000, 3.267716535433071279, -2.401574803149598036 ) ) ;
#19820 = ORIENTED_EDGE ( 'NONE', *, *, #6024, .T. ) ;
#19821 = CARTESIAN_POINT ( 'NONE',  ( -0.3486774197067340486, 3.267716535433071279, 0.1181102362204703021 ) ) ;
#19822 = EDGE_LOOP ( 'NONE', ( #2656, #10805, #1936, #12608 ) ) ;
#19823 = CARTESIAN_POINT ( 'NONE',  ( 1.636583440222563857, 3.267716535433071279, -0.8267716535433055070 ) ) ;
#19824 = DIRECTION ( 'NONE',  ( -0.01601477604151182663, 0.9998717552508123996, -0.000000000000000000 ) ) ;
#19825 = DIRECTION ( 'NONE',  ( 1.000000000000000000, 0.000000000000000000, -3.469446951953613696E-16 ) ) ;
#19826 = VERTEX_POINT ( 'NONE', #17859 ) ;
#19827 = ORIENTED_EDGE ( 'NONE', *, *, #8184, .T. ) ;
#19828 = LINE ( 'NONE', #51023, #45084 ) ;
#19829 = DIRECTION ( 'NONE',  ( 0.000000000000000000, 0.000000000000000000, -1.000000000000000000 ) ) ;
#19830 = CARTESIAN_POINT ( 'NONE',  ( -0.8182917201112819283, 3.346456692913386100, -1.102362204724405492 ) ) ;
#19831 = ADVANCED_FACE ( 'NONE', ( #45449 ), #25855, .F. ) ;
#19832 = DIRECTION ( 'NONE',  ( -0.3090169943749582204, 0.000000000000000000, 0.9510565162951500895 ) ) ;
#19833 = LINE ( 'NONE', #40247, #34713 ) ;
#19834 = AXIS2_PLACEMENT_3D ( 'NONE', #47430, #31733, #36371 ) ;
#19835 = ADVANCED_FACE ( 'NONE', ( #9860 ), #18115, .F. ) ;
#19836 = VECTOR ( 'NONE', #3692, 39.37007874015748143 ) ;
#19837 = LINE ( 'NONE', #40500, #3719 ) ;
#19838 = ORIENTED_EDGE ( 'NONE', *, *, #25037, .F. ) ;
#19839 = DIRECTION ( 'NONE',  ( 0.000000000000000000, 0.000000000000000000, -1.000000000000000000 ) ) ;
#19840 = ADVANCED_FACE ( 'NONE', ( #33622 ), #41609, .F. ) ;
#19841 = ORIENTED_EDGE ( 'NONE', *, *, #13507, .F. ) ;
#19842 = PLANE ( 'NONE',  #16814 ) ;
#19843 = EDGE_CURVE ( 'NONE', #5918, #15669, #6501, .T. ) ;
#19844 = AXIS2_PLACEMENT_3D ( 'NONE', #33241, #711, #28063 ) ;
#19845 = VERTEX_POINT ( 'NONE', #2621 ) ;
#19846 = FACE_OUTER_BOUND ( 'NONE', #21550, .T. ) ;
#19847 = CARTESIAN_POINT ( 'NONE',  ( 0.7148041136150545816, 0.000000000000000000, -2.044646019095610168 ) ) ;
#19848 = ORIENTED_EDGE ( 'NONE', *, *, #18521, .F. ) ;
#19849 = DIRECTION ( 'NONE',  ( -3.469446951953613696E-16, 0.000000000000000000, -1.000000000000000000 ) ) ;
#19850 = ORIENTED_EDGE ( 'NONE', *, *, #3046, .F. ) ;
#19851 = LINE ( 'NONE', #35111, #733 ) ;
#19852 = EDGE_LOOP ( 'NONE', ( #46850, #44757, #43040, #18480, #49434, #8039, #39814, #48591 ) ) ;
#19853 = DIRECTION ( 'NONE',  ( 0.3226000110797114795, 0.000000000000000000, -0.9465353838348411486 ) ) ;
#19854 = CARTESIAN_POINT ( 'NONE',  ( 0.08119777152254364916, 1.623385212329073957, 0.000000000000000000 ) ) ;
#19855 = B_SPLINE_CURVE_WITH_KNOTS ( 'NONE', 3,
 ( #719, #32224, #16473, #32486 ),
 .UNSPECIFIED., .F., .F.,
 ( 4, 4 ),
 ( 2.102946222184170507E-07, 0.002500239313106578012 ),
 .UNSPECIFIED. ) ;
#19856 = ORIENTED_EDGE ( 'NONE', *, *, #45290, .F. ) ;
#19857 = CARTESIAN_POINT ( 'NONE',  ( 2.949782676795221992, 5.905511811023623991, -0.1324748927672368959 ) ) ;
#19858 = EDGE_LOOP ( 'NONE', ( #45662, #43688, #47050, #48639 ) ) ;
#19859 = VERTEX_POINT ( 'NONE', #43103 ) ;
#19860 = CARTESIAN_POINT ( 'NONE',  ( 1.560669927219590303, 3.346456692913386100, -1.299212598425193210 ) ) ;
#19861 = DIRECTION ( 'NONE',  ( 0.000000000000000000, -0.7071067811865479058, 0.7071067811865470176 ) ) ;
#19862 = CARTESIAN_POINT ( 'NONE',  ( -0.8182917201112819283, 3.267716535433071279, -0.1574803149606301411 ) ) ;
#19863 = AXIS2_PLACEMENT_3D ( 'NONE', #36612, #4595, #47668 ) ;
#19864 = VECTOR ( 'NONE', #37080, 39.37007874015748143 ) ;
#19865 = ORIENTED_EDGE ( 'NONE', *, *, #46384, .F. ) ;
#19866 = VECTOR ( 'NONE', #49689, 39.37007874015748143 ) ;
#19867 = PLANE ( 'NONE',  #49266 ) ;
#19868 = DIRECTION ( 'NONE',  ( 0.000000000000000000, 0.000000000000000000, 1.000000000000000000 ) ) ;
#19869 = ORIENTED_EDGE ( 'NONE', *, *, #44663, .T. ) ;
#19870 = LINE ( 'NONE', #33575, #40609 ) ;
#19871 = ADVANCED_FACE ( 'NONE', ( #42356 ), #34377, .F. ) ;
#19872 = EDGE_CURVE ( 'NONE', #26527, #40993, #17076, .T. ) ;
#19873 = ORIENTED_EDGE ( 'NONE', *, *, #4455, .F. ) ;
#19874 = ORIENTED_EDGE ( 'NONE', *, *, #49825, .T. ) ;
#19875 = VECTOR ( 'NONE', #23492, 39.37007874015748143 ) ;
#19876 = ITEM_DEFINED_TRANSFORMATION ( 'NONE', 'NONE', #22622,  #26741 ) ;
#19877 = ADVANCED_FACE ( 'NONE', ( #50806 ), #26858, .T. ) ;
#19878 = VERTEX_POINT ( 'NONE', #19112 ) ;
#19879 = DIRECTION ( 'NONE',  ( -1.000000000000000000, 0.000000000000000000, 0.000000000000000000 ) ) ;
#19880 = AXIS2_PLACEMENT_3D ( 'NONE', #44301, #8177, #47630 ) ;
#19881 = DIRECTION ( 'NONE',  ( -0.000000000000000000, 0.000000000000000000, 1.000000000000000000 ) ) ;
#19882 = CARTESIAN_POINT ( 'NONE',  ( -2.258024766633058622, 3.267716535433071279, 7.834097144030835427E-16 ) ) ;
#19883 = LINE ( 'NONE', #271, #18130 ) ;
#19884 = VERTEX_POINT ( 'NONE', #19614 ) ;
#19885 = VERTEX_POINT ( 'NONE', #23241 ) ;
#19886 = CARTESIAN_POINT ( 'NONE',  ( 2.378961647330872786, 0.000000000000000000, -0.3149606299212596716 ) ) ;
#19887 = ORIENTED_EDGE ( 'NONE', *, *, #22215, .F. ) ;
#19888 = LINE ( 'NONE', #20151, #30916 ) ;
#19889 = CARTESIAN_POINT ( 'NONE',  ( -0.2727639067037602727, 0.000000000000000000, 1.535433070866133898 ) ) ;
#19890 = EDGE_CURVE ( 'NONE', #14486, #27199, #31504, .T. ) ;
#19891 = LINE ( 'NONE', #31027, #34138 ) ;
#19892 = DIRECTION ( 'NONE',  ( 0.000000000000000000, 0.000000000000000000, -1.000000000000000000 ) ) ;
#19893 = FACE_OUTER_BOUND ( 'NONE', #10473, .T. ) ;
#19894 = VERTEX_POINT ( 'NONE', #30747 ) ;
#19895 = CARTESIAN_POINT ( 'NONE',  ( 2.161044708975088380, 5.905511811023623991, 0.1463148319730650238 ) ) ;
#19896 = FILL_AREA_STYLE ('',( #24043 ) ) ;
#19897 = EDGE_CURVE ( 'NONE', #514, #39701, #15503, .T. ) ;
#19898 = ORIENTED_EDGE ( 'NONE', *, *, #5690, .T. ) ;
#19899 = VECTOR ( 'NONE', #43203, 39.37007874015748143 ) ;
#19900 = ORIENTED_EDGE ( 'NONE', *, *, #49175, .F. ) ;
#19901 = CARTESIAN_POINT ( 'NONE',  ( -1.166969139818015977, 3.267716535433071279, -0.4724409448818886470 ) ) ;
#19902 = VECTOR ( 'NONE', #14570, 39.37007874015748143 ) ;
#19903 = CARTESIAN_POINT ( 'NONE',  ( 0.3734705886643994721, 2.755905511811024056, -0.02018660888377523527 ) ) ;
#19904 = DIRECTION ( 'NONE',  ( -1.000000000000000000, 0.000000000000000000, 1.734723475976806848E-16 ) ) ;
#19905 = ORIENTED_EDGE ( 'NONE', *, *, #47048, .T. ) ;
#19906 = VECTOR ( 'NONE', #34244, 39.37007874015748143 ) ;
#19907 = ORIENTED_EDGE ( 'NONE', *, *, #20637, .T. ) ;
#19908 = LINE ( 'NONE', #39802, #13893 ) ;
#19909 = AXIS2_PLACEMENT_3D ( 'NONE', #12853, #48422, #32482 ) ;
#19910 = ORIENTED_EDGE ( 'NONE', *, *, #23626, .F. ) ;
#19911 = FACE_OUTER_BOUND ( 'NONE', #20527, .T. ) ;
#19912 = VERTEX_POINT ( 'NONE', #47204 ) ;
#19913 = AXIS2_PLACEMENT_3D ( 'NONE', #26151, #25894, #49597 ) ;
#19914 = LINE ( 'NONE', #16578, #2911 ) ;
#19915 = CARTESIAN_POINT ( 'NONE',  ( 0.8182917201112817063, 3.346456692913386100, -1.417322834645664331 ) ) ;
#19916 = CARTESIAN_POINT ( 'NONE',  ( 0.2727639067037610499, 3.346456692913386100, 1.102362204724404160 ) ) ;
#19917 = ORIENTED_EDGE ( 'NONE', *, *, #33238, .F. ) ;
#19918 = ORIENTED_EDGE ( 'NONE', *, *, #4555, .F. ) ;
#19919 = EDGE_LOOP ( 'NONE', ( #16537, #26664, #16661, #7831 ) ) ;
#19920 = DIRECTION ( 'NONE',  ( -1.045785279492541006E-16, -1.000000000000000000, -5.036236473261559574E-17 ) ) ;
#19921 = CARTESIAN_POINT ( 'NONE',  ( -1.334208625815133553, 3.267716535433071279, 2.047244094488179567 ) ) ;
#19922 = ORIENTED_EDGE ( 'NONE', *, *, #31221, .T. ) ;
#19923 = ORIENTED_EDGE ( 'NONE', *, *, #19749, .T. ) ;
#19924 = DIRECTION ( 'NONE',  ( -3.469446951953613696E-16, 0.000000000000000000, -1.000000000000000000 ) ) ;
#19925 = CARTESIAN_POINT ( 'NONE',  ( 0.4696143004045479352, 0.000000000000000000, -0.4724409448818886470 ) ) ;
#19926 = FACE_OUTER_BOUND ( 'NONE', #238, .T. ) ;
#19927 = B_SPLINE_CURVE_WITH_KNOTS ( 'NONE', 3,
 ( #14347, #33479, #45307, #9716 ),
 .UNSPECIFIED., .F., .F.,
 ( 4, 4 ),
 ( 0.0001130144768271833412, 0.05016325964078766769 ),
 .UNSPECIFIED. ) ;
#19928 = EDGE_LOOP ( 'NONE', ( #22129, #38232, #17682, #36627 ) ) ;
#19929 = CARTESIAN_POINT ( 'NONE',  ( -1.536664496436148184E-16, 3.346456692913386100, 0.4330708661417287386 ) ) ;
#19930 = CARTESIAN_POINT ( 'NONE',  ( -1.166969139818015533, 3.346456692913386100, 0.4724409448818871482 ) ) ;
#19931 = CARTESIAN_POINT ( 'NONE',  ( 1.485598995959308333, 6.692913385826772199, 1.625606721701627011 ) ) ;
#19932 = ORIENTED_EDGE ( 'NONE', *, *, #32079, .T. ) ;
#19933 = CARTESIAN_POINT ( 'NONE',  ( -1.330011864698828816, 1.686599376747761614, -1.746878811320646152 ) ) ;
#19934 = CARTESIAN_POINT ( 'NONE',  ( -1.363819533518803029, 0.000000000000000000, 1.102362204724404160 ) ) ;
#19935 = ADVANCED_FACE ( 'NONE', ( #27113 ), #26612, .T. ) ;
#19936 = ORIENTED_EDGE ( 'NONE', *, *, #29880, .T. ) ;
#19937 = EDGE_CURVE ( 'NONE', #43573, #4193, #34622, .T. ) ;
#19938 = DIRECTION ( 'NONE',  ( 0.000000000000000000, -1.000000000000000000, 0.000000000000000000 ) ) ;
#19939 = ORIENTED_EDGE ( 'NONE', *, *, #34707, .T. ) ;
#19940 = ORIENTED_EDGE ( 'NONE', *, *, #19658, .F. ) ;
#19941 = DIRECTION ( 'NONE',  ( 0.8584487936018728726, 1.288287287306305283E-16, -0.5128992774058949156 ) ) ;
#19942 = EDGE_CURVE ( 'NONE', #22594, #25844, #31257, .T. ) ;
#19943 = PRODUCT_RELATED_PRODUCT_CATEGORY ( 'part', '', ( #28122 ) ) ;
#19945 = VECTOR ( 'NONE', #3892, 39.37007874015748143 ) ;
#19944 = DIRECTION ( 'NONE',  ( 1.734723475976806848E-16, -0.000000000000000000, 1.000000000000000000 ) ) ;
#19946 = EDGE_CURVE ( 'NONE', #30890, #30042, #38992, .T. ) ;
#19947 = LINE ( 'NONE', #3968, #29450 ) ;
#19948 = ADVANCED_FACE ( 'NONE', ( #7749 ), #3628, .F. ) ;
#19949 = CARTESIAN_POINT ( 'NONE',  ( 1.558105373646058389, 3.346456692913386100, -1.417322834645665441 ) ) ;
#19950 = EDGE_LOOP ( 'NONE', ( #39441, #6431, #42001, #13714 ) ) ;
#19951 = EDGE_LOOP ( 'NONE', ( #42280, #25607, #24255, #10144, #50384, #36888, #43140, #1549, #12270, #33039, #38088, #50670, #526, #27953, #1592, #35388, #32013, #37423, #21984, #11407, #23881, #23699, #14747, #46100, #39651, #47548, #17517, #18269, #26085, #895, #2028, #31259, #7662, #13990, #19467, #34441, #11940, #25833, #109, #49436, #25186, #24966, #28445, #48169, #7002, #41732, #26059, #48732, #48794, #46685, #23725, #36261, #45320, #6331, #29164, #3069, #44078, #46765, #492, #29794, #37065, #7839, #29017, #31541, #15831, #26985, #47550, #30127, #5210, #5872, #10154, #19133, #20499, #35331, #31395, #7560, #1940, #47154, #10891, #49307, #30236, #31251, #32734, #38608, #22201, #33265, #3011, #30743, #16972, #20333, #40785, #28583, #20891, #32239, #9942, #32947, #9053, #27314, #12148, #43022, #35834, #14352, #20554, #28150, #14596, #46628, #30791, #11255, #37173, #11316, #37925, #18606, #41320, #16308, #3730, #23773, #48315, #33234, #29461, #38957, #11205, #3615, #38360, #21931, #18698, #3490, #45270, #17059, #31705, #24582, #9309, #45584, #28599, #44177, #28939, #41206, #14768, #41651, #19161, #2638 ) ) ;
#19952 = AXIS2_PLACEMENT_3D ( 'NONE', #13667, #41043, #21666 ) ;
#19953 = VECTOR ( 'NONE', #2949, 39.37007874015748143 ) ;
#19954 = ORIENTED_EDGE ( 'NONE', *, *, #32175, .T. ) ;
#19955 = DIRECTION ( 'NONE',  ( 1.734723475976806848E-16, 0.000000000000000000, 1.000000000000000000 ) ) ;
#19956 = CARTESIAN_POINT ( 'NONE',  ( 1.058660938151061659, 0.000000000000000000, 1.740053772717023328 ) ) ;
#19957 = VECTOR ( 'NONE', #35298, 39.37007874015748143 ) ;
#19958 = ADVANCED_FACE ( 'NONE', ( #3121 ), #39244, .F. ) ;
#19959 = CARTESIAN_POINT ( 'NONE',  ( 0.000000000000000000, 0.000000000000000000, 0.000000000000000000 ) ) ;
#19960 = DIRECTION ( 'NONE',  ( -0.7530714660036196273, -7.633917315840922073E-17, 0.6579387259397027066 ) ) ;
#19961 = ORIENTED_EDGE ( 'NONE', *, *, #2597, .F. ) ;
#19962 = DIRECTION ( 'NONE',  ( 0.01601477604151182663, -0.9998717552508123996, 0.000000000000000000 ) ) ;
#19963 = EDGE_CURVE ( 'NONE', #39256, #19298, #22496, .T. ) ;
#19964 = CARTESIAN_POINT ( 'NONE',  ( -0.07591351300297333182, 0.000000000000000000, 2.362204724409437961 ) ) ;
#19965 = ORIENTED_EDGE ( 'NONE', *, *, #37937, .T. ) ;
#19966 = DIRECTION ( 'NONE',  ( -3.986037398843765983E-20, -1.000000000000000000, -1.160734090543304660E-16 ) ) ;
#19967 = DIRECTION ( 'NONE',  ( -0.000000000000000000, 1.000000000000000000, -0.000000000000000000 ) ) ;
#19968 = DIRECTION ( 'NONE',  ( 0.000000000000000000, 0.000000000000000000, -1.000000000000000000 ) ) ;
#19969 = ADVANCED_FACE ( 'NONE', ( #35128 ), #50306, .F. ) ;
#19970 = ORIENTED_EDGE ( 'NONE', *, *, #3561, .F. ) ;
#19971 = DIRECTION ( 'NONE',  ( 1.000000000000000000, 0.000000000000000000, 0.000000000000000000 ) ) ;
#19972 = LINE ( 'NONE', #9135, #34100 ) ;
#19973 = CARTESIAN_POINT ( 'NONE',  ( -2.950847925457031007, 1.574821451496988933, -0.08326053095501942392 ) ) ;
#19974 = VERTEX_POINT ( 'NONE', #51053 ) ;
#19975 = CARTESIAN_POINT ( 'NONE',  ( 1.091055626815042645, 0.000000000000000000, 0.1181102362204704270 ) ) ;
#19976 = CARTESIAN_POINT ( 'NONE',  ( -1.195183497228115035E-16, 0.000000000000000000, -0.9448818897637765168 ) ) ;
#19977 = ORIENTED_EDGE ( 'NONE', *, *, #36542, .F. ) ;
#19978 = DIRECTION ( 'NONE',  ( -0.000000000000000000, 1.000000000000000000, -0.000000000000000000 ) ) ;
#19979 = EDGE_CURVE ( 'NONE', #5697, #39853, #42525, .T. ) ;
#19980 = AXIS2_PLACEMENT_3D ( 'NONE', #6447, #5422, #18069 ) ;
#19981 = DIRECTION ( 'NONE',  ( 1.734723475976806848E-16, 0.000000000000000000, 1.000000000000000000 ) ) ;
#19982 = FACE_OUTER_BOUND ( 'NONE', #13974, .T. ) ;
#19983 = CARTESIAN_POINT ( 'NONE',  ( 1.542217245295272932, 0.05262109711011796892, 1.166931937029544564 ) ) ;
#19984 = VECTOR ( 'NONE', #16980, 39.37007874015748143 ) ;
#19985 = VERTEX_POINT ( 'NONE', #15001 ) ;
#19986 = VERTEX_POINT ( 'NONE', #31000 ) ;
#19987 = CARTESIAN_POINT ( 'NONE',  ( 1.015142113812069313, 3.267716535433071279, -3.521981712565032882E-16 ) ) ;
#19988 = DIRECTION ( 'NONE',  ( -0.01601477604151182663, 0.9998717552508123996, -0.000000000000000000 ) ) ;
#19989 = VERTEX_POINT ( 'NONE', #46706 ) ;
#19990 = AXIS2_PLACEMENT_3D ( 'NONE', #2630, #25612, #1612 ) ;
#19991 = CARTESIAN_POINT ( 'NONE',  ( 1.363819533518803251, 0.000000000000000000, 0.7874015748031454320 ) ) ;
#19992 = DIRECTION ( 'NONE',  ( 1.734723475976806848E-16, 0.000000000000000000, 1.000000000000000000 ) ) ;
#19993 = DIRECTION ( 'NONE',  ( -3.469446951953613696E-16, 0.000000000000000000, -1.000000000000000000 ) ) ;
#19994 = CARTESIAN_POINT ( 'NONE',  ( -1.712991727494380223, 1.205361022782829114E-17, -0.3405009913947248945 ) ) ;
#19995 = VECTOR ( 'NONE', #29441, 39.37007874015748143 ) ;
#19996 = EDGE_LOOP ( 'NONE', ( #1687, #43370, #41335, #16008 ) ) ;
#19997 = VERTEX_POINT ( 'NONE', #16007 ) ;
#19998 = DIRECTION ( 'NONE',  ( -0.000000000000000000, -1.000000000000000000, -0.000000000000000000 ) ) ;
#19999 = CARTESIAN_POINT ( 'NONE',  ( 2.932638728931774352, 2.755905511811027164, 0.3475908556738226962 ) ) ;
#20000 = LINE ( 'NONE', #24148, #17313 ) ;
#20001 = PLANE ( 'NONE',  #2608 ) ;
#20002 = FACE_BOUND ( 'NONE', #11363, .T. ) ;
#20003 = VERTEX_POINT ( 'NONE', #28384 ) ;
#20004 = CARTESIAN_POINT ( 'NONE',  ( 0.000000000000000000, 3.267716535433071279, 0.4330708661417290162 ) ) ;
#20005 = ORIENTED_EDGE ( 'NONE', *, *, #45974, .T. ) ;
#20006 = ORIENTED_EDGE ( 'NONE', *, *, #10533, .T. ) ;
#20007 = CARTESIAN_POINT ( 'NONE',  ( 2.464291103507799008, 0.000000000000000000, -1.626664315311302733 ) ) ;
#20008 = ADVANCED_FACE ( 'NONE', ( #4139 ), #20121, .F. ) ;
#20009 = EDGE_CURVE ( 'NONE', #25170, #33806, #4390, .T. ) ;
#20010 = ORIENTED_EDGE ( 'NONE', *, *, #39006, .F. ) ;
#20011 = ORIENTED_EDGE ( 'NONE', *, *, #17818, .F. ) ;
#20012 = CARTESIAN_POINT ( 'NONE',  ( 0.000000000000000000, 3.267716535433071279, 1.377952755905504256 ) ) ;
#20013 = ADVANCED_FACE ( 'NONE', ( #8520 ), #252, .F. ) ;
#20014 = ORIENTED_EDGE ( 'NONE', *, *, #37763, .T. ) ;
#20015 = DIRECTION ( 'NONE',  ( -0.7660444431189771253, 0.6427876096865404731, 0.000000000000000000 ) ) ;
#20016 = DIRECTION ( 'NONE',  ( 0.7526474967735860000, -0.000000000000000000, -0.6584236824419781309 ) ) ;
#20017 = FACE_OUTER_BOUND ( 'NONE', #44386, .T. ) ;
#20018 = CARTESIAN_POINT ( 'NONE',  ( -0.8182917201112814842, 3.346456692913386100, 0.9055118110236167750 ) ) ;
#20019 = CIRCLE ( 'NONE', #48852, 2.165354330708661568 ) ;
#20020 = DIRECTION ( 'NONE',  ( -0.9998717552508122886, -0.01601477604151185785, 0.000000000000000000 ) ) ;
#20021 = CARTESIAN_POINT ( 'NONE',  ( 0.000000000000000000, 3.267716535433071279, 0.9055118110236164419 ) ) ;
#20022 = ORIENTED_EDGE ( 'NONE', *, *, #20316, .T. ) ;
#20023 = DIRECTION ( 'NONE',  ( 1.734723475976806848E-16, -0.000000000000000000, 1.000000000000000000 ) ) ;
#20024 = PLANE ( 'NONE',  #39195 ) ;
#20025 = DIRECTION ( 'NONE',  ( -1.000000000000000000, 0.000000000000000000, 0.000000000000000000 ) ) ;
#20026 = AXIS2_PLACEMENT_3D ( 'NONE', #50570, #19881, #7517 ) ;
#20027 = B_SPLINE_CURVE_WITH_KNOTS ( 'NONE', 3,
 ( #46955, #19619, #43367, #35387 ),
 .UNSPECIFIED., .F., .F.,
 ( 4, 4 ),
 ( 2.329984094937993841E-07, 0.002500456841312296598 ),
 .UNSPECIFIED. ) ;
#20028 = AXIS2_PLACEMENT_3D ( 'NONE', #18083, #46175, #26576 ) ;
#20029 = VERTEX_POINT ( 'NONE', #8002 ) ;
#20030 = CARTESIAN_POINT ( 'NONE',  ( 1.247448100859587239, 0.000000000000000000, -1.633239539486209591 ) ) ;
#20031 = PLANE ( 'NONE',  #7978 ) ;
#20032 = ORIENTED_EDGE ( 'NONE', *, *, #43294, .F. ) ;
#20033 = FACE_OUTER_BOUND ( 'NONE', #42586, .T. ) ;
#20034 = EDGE_CURVE ( 'NONE', #36015, #38547, #31807, .T. ) ;
#20035 = CARTESIAN_POINT ( 'NONE',  ( -0.1692531782225912829, 2.755905511811024056, 0.3335283217915853138 ) ) ;
#20036 = CARTESIAN_POINT ( 'NONE',  ( 1.833433833923351353, 3.346456692913386100, 1.259842519685033135 ) ) ;
#20037 = VECTOR ( 'NONE', #20023, 39.37007874015748143 ) ;
#20038 = CARTESIAN_POINT ( 'NONE',  ( 2.079445128081511829, 0.01975100886603133044, -0.04412578619987858608 ) ) ;
#20039 = ORIENTED_EDGE ( 'NONE', *, *, #42981, .F. ) ;
#20040 = CARTESIAN_POINT ( 'NONE',  ( -0.2493966119946618154, 1.605482210820551758, -2.222016418551142181 ) ) ;
#20041 = EDGE_CURVE ( 'NONE', #33786, #43157, #44132, .T. ) ;
#20042 = CARTESIAN_POINT ( 'NONE',  ( 2.021817418930639931, 3.346456692913386100, 0.5905511811023582691 ) ) ;
#20043 = CARTESIAN_POINT ( 'NONE',  ( -0.3486774197067339376, 3.267716535433071279, -1.574803149606293529 ) ) ;
#20044 = CARTESIAN_POINT ( 'NONE',  ( 1.662150612087327728, 1.049866565067837820, -1.156143393094004601 ) ) ;
#20045 = VERTEX_POINT ( 'NONE', #19862 ) ;
#20046 = EDGE_CURVE ( 'NONE', #25164, #25916, #16970, .T. ) ;
#20047 = ORIENTED_EDGE ( 'NONE', *, *, #19757, .T. ) ;
#20048 = ORIENTED_EDGE ( 'NONE', *, *, #29758, .F. ) ;
#20049 = LINE ( 'NONE', #28314, #20470 ) ;
#20050 = VERTEX_POINT ( 'NONE', #35633 ) ;
#20051 = EDGE_CURVE ( 'NONE', #33474, #13670, #8776, .T. ) ;
#20052 = DIRECTION ( 'NONE',  ( -1.000000000000000000, 0.000000000000000000, 1.734723475976806848E-16 ) ) ;
#20053 = EDGE_LOOP ( 'NONE', ( #41286, #24145, #47027, #42706 ) ) ;
#20054 = EDGE_CURVE ( 'NONE', #850, #5596, #44390, .T. ) ;
#20055 = FACE_OUTER_BOUND ( 'NONE', #35895, .T. ) ;
#20056 = ORIENTED_EDGE ( 'NONE', *, *, #21304, .F. ) ;
#20057 = CARTESIAN_POINT ( 'NONE',  ( -0.5455278134075208785, 3.267716535433071279, 0.6299212598425164567 ) ) ;
#20058 = VECTOR ( 'NONE', #13424, 39.37007874015748143 ) ;
#20059 = PLANE ( 'NONE',  #39682 ) ;
#20060 = ORIENTED_EDGE ( 'NONE', *, *, #38036, .F. ) ;
#20061 = CARTESIAN_POINT ( 'NONE',  ( -1.909347346926324906, 0.000000000000000000, 1.417322834645662333 ) ) ;
#20062 = CIRCLE ( 'NONE', #6886, 2.165354330708661568 ) ;
#20063 = EDGE_LOOP ( 'NONE', ( #50837, #36993, #23936, #3433 ) ) ;
#20064 = B_SPLINE_CURVE_WITH_KNOTS ( 'NONE', 3,
 ( #36114, #221, #746, #36625 ),
 .UNSPECIFIED., .F., .F.,
 ( 4, 4 ),
 ( 2.051433891274529492E-07, 0.01996805375819276154 ),
 .UNSPECIFIED. ) ;
#20065 = VECTOR ( 'NONE', #20079, 39.37007874015748143 ) ;
#20066 = EDGE_CURVE ( 'NONE', #26908, #19026, #1285, .T. ) ;
#20067 = VECTOR ( 'NONE', #26511, 39.37007874015748143 ) ;
#20068 = CARTESIAN_POINT ( 'NONE',  ( -0.07591351300297333182, 3.346456692913386100, 0.1574803149606283648 ) ) ;
#20069 = VERTEX_POINT ( 'NONE', #8264 ) ;
#20070 = ORIENTED_EDGE ( 'NONE', *, *, #32074, .T. ) ;
#20071 = ADVANCED_FACE ( 'NONE', ( #4903, #48483, #13171, #35889, #4652, #39757, #36402, #12390, #16263, #32024, #28125, #16788, #778, #518, #47715, #16527, #32279, #24527, #20647, #1028, #32541, #48232, #12915, #9034, #40532, #5155, #20907, #9289, #21934, #21171, #9546, #13676, #33057, #40789, #37693, #36920, #17799, #48735, #41050, #1794, #1544, #13418, #5415, #2306, #17297, #33566, #29157, #5673, #17545, #25035, #22187, #44634, #13933, #18307, #45644, #41549, #49251, #34063, #37433, #18059, #14175, #2563, #49500, #45141, #33309, #26052, #5920, #45393, #29679, #10055, #44890, #25797, #41805, #33819, #6181, #25540, #37942, #29928, #48994, #29420, #9803, #10308, #25293, #6438, #21423, #41300, #37177, #21676, #49752, #14435, #2054, #34322, #6691, #23893, #26804, #656, #30183, #43497, #45900, #8151, #22439, #38197, #50254, #14941, #38695, #30688, #24150, #50009, #4529, #4270, #42299, #46401, #18818, #16149, #7201, #46653, #46155, #39639, #36032, #39895, #20002, #14690, #2817, #18568, #20269, #30944, #34567, #3315, #35768, #27755, #31909, #11071, #10563, #34813, #42054, #42556, #43749, #395, #50497, #47600, #19057, #12278, #28014, #30441, #8404, #15193, #26307, #10809, #26553, #6944, #12018, #22688, #22940, #38446, #3068, #29292, #44274, #36288, #24409, #4786, #5803, #44773, #8654, #40668, #20533, #12791, #24668, #47856, #45030, #16411, #36798, #41184, #17424, #13303, #5293, #21552, #9168, #40926, #37056, #16671, #9681, #16921, #40422, #48870, #28785, #25417, #8913, #28265, #40162, #5040, #1677, #28523, #36545, #909, #20786, #33189, #32944, #17175, #1421, #21046, #37313, #9426, #32420, #1164, #48111, #32683, #48621, #44524, #32163, #24918, #29034, #48365, #12527, #25172, #13052, #5550, #21302, #13557, #44010, #14309, #46283, #30063, #2691, #41934, #18442, #1932, #22320, #50135, #26433, #38072, #33943, #17935, #30316, #34447, #49384, #45522, #26684, #14822 ), #21811, .T. ) ;
#20072 = DIRECTION ( 'NONE',  ( 0.000000000000000000, 1.000000000000000000, -0.000000000000000000 ) ) ;
#20073 = VECTOR ( 'NONE', #29765, 39.37007874015748143 ) ;
#20074 = DIRECTION ( 'NONE',  ( -3.469446951953613696E-16, 0.000000000000000000, -1.000000000000000000 ) ) ;
#20075 = ORIENTED_EDGE ( 'NONE', *, *, #42731, .T. ) ;
#20076 = FACE_OUTER_BOUND ( 'NONE', #42901, .T. ) ;
#20077 = EDGE_LOOP ( 'NONE', ( #34291, #16094, #21458 ) ) ;
#20078 = DIRECTION ( 'NONE',  ( 0.01601477604151182663, -0.9998717552508123996, 0.000000000000000000 ) ) ;
#20079 = DIRECTION ( 'NONE',  ( 1.734723475976806848E-16, -0.000000000000000000, 1.000000000000000000 ) ) ;
#20080 = PLANE ( 'NONE',  #9060 ) ;
#20081 = VERTEX_POINT ( 'NONE', #10945 ) ;
#20082 = ORIENTED_EDGE ( 'NONE', *, *, #42965, .T. ) ;
#20083 = DIRECTION ( 'NONE',  ( -3.469446951953613696E-16, 0.000000000000000000, -1.000000000000000000 ) ) ;
#20084 = PLANE ( 'NONE',  #41840 ) ;
#20085 = CARTESIAN_POINT ( 'NONE',  ( -1.636583440222563635, 0.000000000000000000, 0.1181102362204704270 ) ) ;
#20086 = B_SPLINE_CURVE_WITH_KNOTS ( 'NONE', 3,
 ( #19172, #11439, #11188, #47267 ),
 .UNSPECIFIED., .F., .F.,
 ( 4, 4 ),
 ( 0.01401300212335106037, 0.03074580230677671083 ),
 .UNSPECIFIED. ) ;
#20087 = CARTESIAN_POINT ( 'NONE',  ( -1.439733046521777027, 3.267716535433071279, 1.377952755905504256 ) ) ;
#20088 = LINE ( 'NONE', #35857, #13265 ) ;
#20089 = CARTESIAN_POINT ( 'NONE',  ( 1.531154912952773284, 5.905511811023623991, 1.532020527533857424 ) ) ;
#20090 = VERTEX_POINT ( 'NONE', #37821 ) ;
#20091 = ADVANCED_FACE ( 'NONE', ( #49131 ), #22821, .F. ) ;
#20092 = CARTESIAN_POINT ( 'NONE',  ( -2.121605289024800722, 3.346456692913386100, 0.4330708661417290162 ) ) ;
#20093 = AXIS2_PLACEMENT_3D ( 'NONE', #43184, #11704, #3963 ) ;
#20094 = ORIENTED_EDGE ( 'NONE', *, *, #38998, .T. ) ;
#20095 = CARTESIAN_POINT ( 'NONE',  ( -0.8942052331142549271, 3.267716535433071279, 3.102397620449222481E-16 ) ) ;
#20096 = VECTOR ( 'NONE', #21953, 39.37007874015748143 ) ;
#20097 = VECTOR ( 'NONE', #15728, 39.37007874015748143 ) ;
#20098 = VERTEX_POINT ( 'NONE', #6576 ) ;
#20099 = EDGE_CURVE ( 'NONE', #22312, #21069, #21091, .T. ) ;
#20100 = VECTOR ( 'NONE', #33433, 39.37007874015748143 ) ;
#20102 = VECTOR ( 'NONE', #39476, 39.37007874015748143 ) ;
#20101 = FACE_OUTER_BOUND ( 'NONE', #15582, .T. ) ;
#20103 = DIRECTION ( 'NONE',  ( 1.000000000000000000, 0.000000000000000000, 0.000000000000000000 ) ) ;
#20104 = EDGE_CURVE ( 'NONE', #4657, #48594, #49881, .T. ) ;
#20105 = FACE_OUTER_BOUND ( 'NONE', #35988, .T. ) ;
#20106 = VERTEX_POINT ( 'NONE', #13812 ) ;
#20107 = EDGE_CURVE ( 'NONE', #38209, #19566, #30570, .T. ) ;
#20108 = EDGE_CURVE ( 'NONE', #39410, #23414, #10697, .T. ) ;
#20109 = CONICAL_SURFACE ( 'NONE', #6939, 1.850107469027523210, 0.6386652850508578450 ) ;
#20110 = DIRECTION ( 'NONE',  ( -1.000000000000000000, 0.000000000000000000, 0.000000000000000000 ) ) ;
#20111 = ORIENTED_EDGE ( 'NONE', *, *, #23976, .F. ) ;
#20112 = DIRECTION ( 'NONE',  ( -0.9989930665413151445, -5.167793568183051143E-18, 0.04486483035050446017 ) ) ;
#20113 = ORIENTED_EDGE ( 'NONE', *, *, #18960, .T. ) ;
#20114 = FACE_OUTER_BOUND ( 'NONE', #28776, .T. ) ;
#20115 = CARTESIAN_POINT ( 'NONE',  ( 0.08119777152254364916, 1.623385212329073957, 0.000000000000000000 ) ) ;
#20116 = CARTESIAN_POINT ( 'NONE',  ( 0.1224067236346046000, 0.009932954893344222297, -1.909056982598775765 ) ) ;
#20117 = ORIENTED_EDGE ( 'NONE', *, *, #11761, .T. ) ;
#20118 = ORIENTED_EDGE ( 'NONE', *, *, #36759, .T. ) ;
#20119 = CARTESIAN_POINT ( 'NONE',  ( 1.312623452344845232, 5.905511811023623991, 1.722945714930923744 ) ) ;
#20120 = LINE ( 'NONE', #42852, #926 ) ;
#20121 = PLANE ( 'NONE',  #3763 ) ;
#20122 = B_SPLINE_CURVE_WITH_KNOTS ( 'NONE', 3,
 ( #48146, #5071, #47633, #20300 ),
 .UNSPECIFIED., .F., .F.,
 ( 4, 4 ),
 ( 2.018431748241431644E-07, 0.002500215118228798356 ),
 .UNSPECIFIED. ) ;
#20123 = EDGE_CURVE ( 'NONE', #50597, #35404, #10443, .T. ) ;
#20124 = B_SPLINE_CURVE_WITH_KNOTS ( 'NONE', 3,
 ( #4586, #1475, #16724, #48170 ),
 .UNSPECIFIED., .F., .F.,
 ( 4, 4 ),
 ( 0.001799345260683910160, 0.004299357162589153257 ),
 .UNSPECIFIED. ) ;
#20125 = ORIENTED_EDGE ( 'NONE', *, *, #8893, .F. ) ;
#20126 = EDGE_CURVE ( 'NONE', #8254, #5726, #9552, .T. ) ;
#20127 = CARTESIAN_POINT ( 'NONE',  ( 0.2727639067037609943, 0.000000000000000000, 1.850393700787392293 ) ) ;
#20128 = CARTESIAN_POINT ( 'NONE',  ( -1.439733046521776583, 3.346456692913386100, 1.537421584259135443 ) ) ;
#20129 = VERTEX_POINT ( 'NONE', #9937 ) ;
#20130 = ADVANCED_FACE ( 'NONE', ( #22564 ), #7086, .T. ) ;
#20131 = CARTESIAN_POINT ( 'NONE',  ( -0.5455278134075214336, 0.000000000000000000, 2.007874015748021268 ) ) ;
#20132 = EDGE_CURVE ( 'NONE', #19764, #4018, #14059, .T. ) ;
#20133 = ORIENTED_EDGE ( 'NONE', *, *, #34847, .T. ) ;
#20134 = VECTOR ( 'NONE', #14611, 39.37007874015748143 ) ;
#20135 = ORIENTED_EDGE ( 'NONE', *, *, #21083, .F. ) ;
#20136 = SHAPE_DEFINITION_REPRESENTATION ( #46625, #15265 ) ;
#20137 = AXIS2_PLACEMENT_3D ( 'NONE', #2286, #33544, #22420 ) ;
#20138 = ORIENTED_EDGE ( 'NONE', *, *, #43309, .F. ) ;
#20139 = CARTESIAN_POINT ( 'NONE',  ( -0.2156685157583831947, 1.617455082123532062, -2.945280361644576850 ) ) ;
#20140 = VECTOR ( 'NONE', #4823, 39.37007874015748143 ) ;
#20141 = PLANE ( 'NONE',  #28294 ) ;
#20142 = DIRECTION ( 'NONE',  ( -1.000000000000000000, -0.000000000000000000, -0.000000000000000000 ) ) ;
#20143 = DIRECTION ( 'NONE',  ( 1.000000000000000000, -0.000000000000000000, 0.000000000000000000 ) ) ;
#20144 = ORIENTED_EDGE ( 'NONE', *, *, #34418, .F. ) ;
#20145 = ORIENTED_EDGE ( 'NONE', *, *, #10696, .F. ) ;
#20146 = AXIS2_PLACEMENT_3D ( 'NONE', #364, #32387, #40390 ) ;
#20147 = CARTESIAN_POINT ( 'NONE',  ( -1.522953965282238586, 0.003526770554233742919, 0.8754220627670087351 ) ) ;
#20148 = CARTESIAN_POINT ( 'NONE',  ( -1.712496953225537633, 0.000000000000000000, -1.102362204724405492 ) ) ;
#20149 = CARTESIAN_POINT ( 'NONE',  ( 2.296360773918335152, 1.711873972321264814, 0.3607252540896742632 ) ) ;
#20150 = VERTEX_POINT ( 'NONE', #2190 ) ;
#20151 = CARTESIAN_POINT ( 'NONE',  ( -1.909347346926325129, 3.346456692913386100, -0.8893194486674343979 ) ) ;
#20152 = LINE ( 'NONE', #27899, #29733 ) ;
#20153 = CARTESIAN_POINT ( 'NONE',  ( 0.7190704387038853174, 0.000000000000000000, 1.869489989794381080 ) ) ;
#20154 = CARTESIAN_POINT ( 'NONE',  ( -1.636583440222564301, 0.000000000000000000, -1.141732283464563791 ) ) ;
#20155 = CARTESIAN_POINT ( 'NONE',  ( 0.7423782071083085965, 0.000000000000000000, -1.456692913385822630 ) ) ;
#20156 = ORIENTED_EDGE ( 'NONE', *, *, #6922, .T. ) ;
#20157 = PLANE ( 'NONE',  #15152 ) ;
#20158 = ORIENTED_EDGE ( 'NONE', *, *, #20841, .T. ) ;
#20159 = EDGE_LOOP ( 'NONE', ( #11248, #1998, #10312, #8160 ) ) ;
#20160 = CARTESIAN_POINT ( 'NONE',  ( -1.985260859929297572, 3.346456692913386100, 0.3149606299212578953 ) ) ;
#20161 = LINE ( 'NONE', #16305, #19572 ) ;
#20162 = CARTESIAN_POINT ( 'NONE',  ( -0.8942052331142548161, 3.267716535433071279, 3.102397620449221988E-16 ) ) ;
#20163 = EDGE_CURVE ( 'NONE', #16898, #12857, #41681, .T. ) ;
#20164 = ORIENTED_EDGE ( 'NONE', *, *, #8153, .T. ) ;
#20165 = EDGE_CURVE ( 'NONE', #21513, #2854, #6319, .T. ) ;
#20166 = CIRCLE ( 'NONE', #25981, 2.165354330708661568 ) ;
#20167 = EDGE_CURVE ( 'NONE', #10246, #31232, #31840, .T. ) ;
#20168 = VERTEX_POINT ( 'NONE', #8336 ) ;
#20169 = VECTOR ( 'NONE', #49783, 39.37007874015748143 ) ;
#20170 = DIRECTION ( 'NONE',  ( -1.000000000000000000, 0.000000000000000000, -0.000000000000000000 ) ) ;
#20171 = VERTEX_POINT ( 'NONE', #43177 ) ;
#20172 = FACE_OUTER_BOUND ( 'NONE', #14172, .T. ) ;
#20173 = ADVANCED_FACE ( 'NONE', ( #3957 ), #31075, .F. ) ;
#20174 = VECTOR ( 'NONE', #25720, 39.37007874015748143 ) ;
#20175 = VERTEX_POINT ( 'NONE', #39069 ) ;
#20176 = LINE ( 'NONE', #24574, #36750 ) ;
#20177 = DIRECTION ( 'NONE',  ( -0.000000000000000000, 1.000000000000000000, -0.000000000000000000 ) ) ;
#20178 = CARTESIAN_POINT ( 'NONE',  ( -1.358040552251954969, 1.036177007133961769, 2.177027195213288913 ) ) ;
#20179 = EDGE_LOOP ( 'NONE', ( #3650, #8895, #41863, #43078 ) ) ;
#20180 = EDGE_LOOP ( 'NONE', ( #6765, #35168, #44548, #34432 ) ) ;
#20181 = ORIENTED_EDGE ( 'NONE', *, *, #46423, .F. ) ;
#20182 = CARTESIAN_POINT ( 'NONE',  ( -1.712991727494380223, 1.205361022782829114E-17, -0.3405009913947248945 ) ) ;
#20183 = VECTOR ( 'NONE', #12149, 39.37007874015748143 ) ;
#20184 = PLANE ( 'NONE',  #37889 ) ;
#20185 = ORIENTED_EDGE ( 'NONE', *, *, #2198, .T. ) ;
#20186 = ORIENTED_EDGE ( 'NONE', *, *, #2784, .T. ) ;
#20187 = CARTESIAN_POINT ( 'NONE',  ( -1.494044303739022972, 0.003989811691878806209, -0.9272426299426647089 ) ) ;
#20188 = CARTESIAN_POINT ( 'NONE',  ( 1.287906020515830585, 3.267716535433071279, 1.574803149606291974 ) ) ;
#20189 = CARTESIAN_POINT ( 'NONE',  ( -1.363819533518803473, 3.346456692913386100, -1.732283464566922726 ) ) ;
#20190 = B_SPLINE_CURVE_WITH_KNOTS ( 'NONE', 3,
 ( #26692, #14067, #14319, #42441 ),
 .UNSPECIFIED., .F., .F.,
 ( 4, 4 ),
 ( 9.735347569733346160E-07, 6.298333608436676246E-06 ),
 .UNSPECIFIED. ) ;
#20191 = EDGE_CURVE ( 'NONE', #43265, #29231, #19690, .T. ) ;
#20192 = VERTEX_POINT ( 'NONE', #34948 ) ;
#20193 = EDGE_CURVE ( 'NONE', #3832, #12397, #26906, .T. ) ;
#20194 = PLANE ( 'NONE',  #22987 ) ;
#20195 = DIRECTION ( 'NONE',  ( 1.734723475976806848E-16, -0.000000000000000000, 1.000000000000000000 ) ) ;
#20196 = DIRECTION ( 'NONE',  ( 0.08963930890344089242, 1.156025585781303350E-16, -0.9959742939952384022 ) ) ;
#20197 = VERTEX_POINT ( 'NONE', #4207 ) ;
#20198 = CARTESIAN_POINT ( 'NONE',  ( -2.399080495885657083, 1.575253574022198455, 0.3746395858504699694 ) ) ;
#20199 = CARTESIAN_POINT ( 'NONE',  ( -2.793030215715272213, 1.205361022782829114E-17, 0.9592557174602285297 ) ) ;
#20200 = ORIENTED_EDGE ( 'NONE', *, *, #30975, .T. ) ;
#20201 = EDGE_CURVE ( 'NONE', #49607, #28604, #3703, .T. ) ;
#20202 = CARTESIAN_POINT ( 'NONE',  ( 1.833433833923351353, 3.346456692913386100, -0.6299212598425181220 ) ) ;
#20203 = ORIENTED_EDGE ( 'NONE', *, *, #43277, .F. ) ;
#20204 = VERTEX_POINT ( 'NONE', #71 ) ;
#20205 = CARTESIAN_POINT ( 'NONE',  ( 1.287906020515829919, 0.000000000000000000, -1.574803149606294417 ) ) ;
#20206 = CYLINDRICAL_SURFACE ( 'NONE', #25899, 2.854330708661417138 ) ;
#20207 = ADVANCED_FACE ( 'NONE', ( #15819 ), #47280, .F. ) ;
#20208 = CARTESIAN_POINT ( 'NONE',  ( -1.091055626815042201, 0.000000000000000000, 1.259842519685033357 ) ) ;
#20209 = DIRECTION ( 'NONE',  ( 1.734723475976806848E-16, -0.000000000000000000, 1.000000000000000000 ) ) ;
#20210 = DIRECTION ( 'NONE',  ( -0.9998717552508121775, -0.01601477604151182663, 0.000000000000000000 ) ) ;
#20211 = ORIENTED_EDGE ( 'NONE', *, *, #28042, .T. ) ;
#20212 = ORIENTED_EDGE ( 'NONE', *, *, #3669, .F. ) ;
#20213 = VECTOR ( 'NONE', #14904, 39.37007874015748143 ) ;
#20214 = VECTOR ( 'NONE', #44046, 39.37007874015748143 ) ;
#20215 = VECTOR ( 'NONE', #31994, 39.37007874015748143 ) ;
#20216 = ORIENTED_EDGE ( 'NONE', *, *, #17911, .T. ) ;
#20217 = LINE ( 'NONE', #4220, #21155 ) ;
#20218 = CARTESIAN_POINT ( 'NONE',  ( 0.1968503937007873017, 3.346456692913386100, -0.9448818897637765168 ) ) ;
#20219 = VECTOR ( 'NONE', #822, 39.37007874015748143 ) ;
#20220 = DIRECTION ( 'NONE',  ( -1.000000000000000000, 0.000000000000000000, 1.734723475976806848E-16 ) ) ;
#20221 = CARTESIAN_POINT ( 'NONE',  ( 2.919426793319799707, 1.764751637901927905, 0.4451252810446822417 ) ) ;
#20222 = FACE_OUTER_BOUND ( 'NONE', #37211, .T. ) ;
#20223 = CIRCLE ( 'NONE', #42493, 2.106299212598425008 ) ;
#20224 = ORIENTED_EDGE ( 'NONE', *, *, #13706, .T. ) ;
#20225 = FACE_OUTER_BOUND ( 'NONE', #7220, .T. ) ;
#20226 = DIRECTION ( 'NONE',  ( 1.734723475976806848E-16, 0.000000000000000000, 1.000000000000000000 ) ) ;
#20227 = ORIENTED_EDGE ( 'NONE', *, *, #24296, .F. ) ;
#20228 = DIRECTION ( 'NONE',  ( 0.000000000000000000, 1.160734090543304660E-16, -1.000000000000000000 ) ) ;
#20229 = CARTESIAN_POINT ( 'NONE',  ( -1.531154912952794378, 0.000000000000000000, 1.532020527533835441 ) ) ;
#20230 =( BOUNDED_CURVE ( )  B_SPLINE_CURVE ( 3, ( #2697, #48876, #2456, #21309 ),
 .UNSPECIFIED., .F., .F. ) 
 B_SPLINE_CURVE_WITH_KNOTS ( ( 4, 4 ),
 ( 3.808740206672671214, 3.859579113281694340 ),
 .UNSPECIFIED. ) 
 CURVE ( )  GEOMETRIC_REPRESENTATION_ITEM ( )  RATIONAL_B_SPLINE_CURVE ( ( 1.000000000000000000, 0.9997846287284284372, 0.9997846287284284372, 1.000000000000000000 ) ) 
 REPRESENTATION_ITEM ( '' )  );
#20231 = CARTESIAN_POINT ( 'NONE',  ( -0.6214413264104945434, 3.267716535433071279, 2.156057715732901026E-16 ) ) ;
#20232 = ORIENTED_EDGE ( 'NONE', *, *, #21446, .F. ) ;
#20233 = CARTESIAN_POINT ( 'NONE',  ( -0.8942052331142547050, 3.346456692913386100, 1.259842519685033357 ) ) ;
#20234 = DIRECTION ( 'NONE',  ( -3.469446951953613696E-16, 0.000000000000000000, -1.000000000000000000 ) ) ;
#20235 = CARTESIAN_POINT ( 'NONE',  ( 0.08139965876239094178, 1.610780518492231694, 0.000000000000000000 ) ) ;
#20236 = EDGE_CURVE ( 'NONE', #35848, #31200, #46778, .T. ) ;
#20237 = EDGE_CURVE ( 'NONE', #47091, #48366, #30822, .T. ) ;
#20238 = ORIENTED_EDGE ( 'NONE', *, *, #36893, .F. ) ;
#20239 = FACE_BOUND ( 'NONE', #15416, .T. ) ;
#20240 = LINE ( 'NONE', #49606, #6008 ) ;
#20241 = ORIENTED_EDGE ( 'NONE', *, *, #15867, .T. ) ;
#20242 = DIRECTION ( 'NONE',  ( -0.6579387259397136978, 0.000000000000000000, 0.7530714660036097463 ) ) ;
#20243 = EDGE_CURVE ( 'NONE', #26089, #40673, #20301, .T. ) ;
#20244 = CARTESIAN_POINT ( 'NONE',  ( 0.9237497747831215911, 0.5249316497054298258, 1.642046528974287378 ) ) ;
#20245 = CARTESIAN_POINT ( 'NONE',  ( 1.287906020515829919, 3.267716535433071279, -1.889763779527552368 ) ) ;
#20246 = LINE ( 'NONE', #31891, #11976 ) ;
#20247 = ADVANCED_FACE ( 'NONE', ( #12210 ), #42926, .F. ) ;
#20248 = EDGE_LOOP ( 'NONE', ( #8162, #827, #33319, #46083 ) ) ;
#20249 = EDGE_LOOP ( 'NONE', ( #35579, #50392, #6305, #7232 ) ) ;
#20250 = CARTESIAN_POINT ( 'NONE',  ( -2.823445274216743073, 1.573787237234608005, 0.8656477926280277124 ) ) ;
#20251 = VECTOR ( 'NONE', #36438, 39.37007874015748143 ) ;
#20252 = CARTESIAN_POINT ( 'NONE',  ( 1.287906020515830141, 3.346456692913386100, 0.3149606299212578953 ) ) ;
#20253 = AXIS2_PLACEMENT_3D ( 'NONE', #45407, #13947, #26068 ) ;
#20254 = ORIENTED_EDGE ( 'NONE', *, *, #20431, .T. ) ;
#20255 = DIRECTION ( 'NONE',  ( 1.000000000000000000, 0.000000000000000000, 0.000000000000000000 ) ) ;
#20256 = CARTESIAN_POINT ( 'NONE',  ( -1.363819533518803473, 0.000000000000000000, -1.102362204724405270 ) ) ;
#20257 = FACE_OUTER_BOUND ( 'NONE', #37614, .T. ) ;
#20258 = AXIS2_PLACEMENT_3D ( 'NONE', #9026, #36912, #28636 ) ;
#20259 = CARTESIAN_POINT ( 'NONE',  ( 0.000000000000000000, 3.267716535433071279, 0.000000000000000000 ) ) ;
#20260 = VERTEX_POINT ( 'NONE', #15578 ) ;
#20261 = ORIENTED_EDGE ( 'NONE', *, *, #39564, .T. ) ;
#20262 = ADVANCED_FACE ( 'NONE', ( #50381 ), #23826, .F. ) ;
#20263 = EDGE_CURVE ( 'NONE', #33586, #13738, #11450, .T. ) ;
#20264 = LINE ( 'NONE', #32159, #34502 ) ;
#20265 = CARTESIAN_POINT ( 'NONE',  ( -1.732283464566932052, 3.267716535433071279, -1.299212598425193210 ) ) ;
#20266 = AXIS2_PLACEMENT_3D ( 'NONE', #24271, #12137, #36146 ) ;
#20267 = CARTESIAN_POINT ( 'NONE',  ( -0.8182917201112814842, 3.346456692913386100, 0.4724409448818872592 ) ) ;
#20268 = PLANE ( 'NONE',  #36405 ) ;
#20270 = VECTOR ( 'NONE', #35433, 39.37007874015748143 ) ;
#20269 = FACE_BOUND ( 'NONE', #47857, .T. ) ;
#20271 = ORIENTED_EDGE ( 'NONE', *, *, #29869, .T. ) ;
#20272 = EDGE_CURVE ( 'NONE', #48050, #20926, #38574, .T. ) ;
#20273 = CARTESIAN_POINT ( 'NONE',  ( -2.122513613727505799, 1.575480814016643638, -0.4339716895473832436 ) ) ;
#20274 = EDGE_LOOP ( 'NONE', ( #37701, #585, #17691, #24962 ) ) ;
#20275 = VERTEX_POINT ( 'NONE', #34695 ) ;
#20276 = CARTESIAN_POINT ( 'NONE',  ( 2.491402175429654253, 1.659612532563349285, -1.585592796919505831 ) ) ;
#20277 = ORIENTED_EDGE ( 'NONE', *, *, #42920, .F. ) ;
#20278 = ORIENTED_EDGE ( 'NONE', *, *, #38504, .T. ) ;
#20279 = CARTESIAN_POINT ( 'NONE',  ( -0.07591351300297359550, 3.346456692913386100, -2.047244094488181343 ) ) ;
#20280 = EDGE_LOOP ( 'NONE', ( #7444, #21442, #21856, #8507 ) ) ;
#20281 = LINE ( 'NONE', #148, #29567 ) ;
#20282 = ADVANCED_FACE ( 'NONE', ( #47023 ), #11199, .F. ) ;
#20283 = LINE ( 'NONE', #24422, #23604 ) ;
#20284 = LINE ( 'NONE', #27772, #16842 ) ;
#20285 = CIRCLE ( 'NONE', #4631, 1.181102362204723200 ) ;
#20286 = CARTESIAN_POINT ( 'NONE',  ( 0.4696143004045484348, 3.267716535433071279, -1.629301903132388985E-16 ) ) ;
#20287 = FACE_OUTER_BOUND ( 'NONE', #42350, .T. ) ;
#20288 = CARTESIAN_POINT ( 'NONE',  ( 0.2727639067037602172, 0.000000000000000000, -2.244094488188969727 ) ) ;
#20289 = VECTOR ( 'NONE', #42753, 39.37007874015748143 ) ;
#20290 = ORIENTED_EDGE ( 'NONE', *, *, #49428, .F. ) ;
#20291 = CARTESIAN_POINT ( 'NONE',  ( -1.985260859929297572, 0.000000000000000000, 0.9448818897637749625 ) ) ;
#20292 = AXIS2_PLACEMENT_3D ( 'NONE', #22391, #31148, #38144 ) ;
#20293 = CARTESIAN_POINT ( 'NONE',  ( 0.1968503937007870241, 3.346456692913386100, -2.204724409448811429 ) ) ;
#20294 = VECTOR ( 'NONE', #44759, 39.37007874015748143 ) ;
#20295 = CARTESIAN_POINT ( 'NONE',  ( -1.181102362204724310, 0.4724409448818890911, -1.062992125984252079 ) ) ;
#20296 = ORIENTED_EDGE ( 'NONE', *, *, #15240, .T. ) ;
#20297 = PLANE ( 'NONE',  #27299 ) ;
#20298 = LINE ( 'NONE', #8684, #49988 ) ;
#20299 = VERTEX_POINT ( 'NONE', #38822 ) ;
#20300 = CARTESIAN_POINT ( 'NONE',  ( 2.932638728931774352, 1.447899366913586672, 0.3475908556738225297 ) ) ;
#20301 = CIRCLE ( 'NONE', #28519, 2.244934639244525076 ) ;
#20302 = FACE_OUTER_BOUND ( 'NONE', #15319, .T. ) ;
#20303 = DIRECTION ( 'NONE',  ( -0.6234898018587431423, 0.000000000000000000, 0.7818314824680221431 ) ) ;
#20304 = AXIS2_PLACEMENT_3D ( 'NONE', #46643, #12068, #11311 ) ;
#20305 = EDGE_CURVE ( 'NONE', #24856, #28374, #27437, .T. ) ;
#20306 = PRODUCT_DEFINITION_SHAPE ( 'NONE', 'NONE',  #51054 ) ;
#20307 = ORIENTED_EDGE ( 'NONE', *, *, #15432, .T. ) ;
#20308 = DIRECTION ( 'NONE',  ( 0.000000000000000000, 1.160734090543304660E-16, -1.000000000000000000 ) ) ;
#20309 = EDGE_LOOP ( 'NONE', ( #29912, #25378, #1934, #15798 ) ) ;
#20310 = DIRECTION ( 'NONE',  ( -0.000000000000000000, 1.000000000000000000, -0.000000000000000000 ) ) ;
#20311 = EDGE_CURVE ( 'NONE', #6610, #45728, #40601, .T. ) ;
#20312 = DIRECTION ( 'NONE',  ( 1.000000000000000000, -0.000000000000000000, 0.000000000000000000 ) ) ;
#20313 = PLANE ( 'NONE',  #45705 ) ;
#20315 = ADVANCED_FACE ( 'NONE', ( #9099 ), #4722, .F. ) ;
#20314 = CARTESIAN_POINT ( 'NONE',  ( -1.636583440222563635, 3.267716535433071279, 2.839019714148966584E-16 ) ) ;
#20316 = EDGE_CURVE ( 'NONE', #49974, #47433, #24082, .T. ) ;
#20317 = ORIENTED_EDGE ( 'NONE', *, *, #33657, .T. ) ;
#20318 = ORIENTED_EDGE ( 'NONE', *, *, #6929, .T. ) ;
#20319 = DIRECTION ( 'NONE',  ( -1.000000000000000000, 0.000000000000000000, -0.000000000000000000 ) ) ;
#20320 = VERTEX_POINT ( 'NONE', #8846 ) ;
#20321 = DIRECTION ( 'NONE',  ( -0.01601477604151182663, 0.9998717552508123996, -0.000000000000000000 ) ) ;
#20322 = ORIENTED_EDGE ( 'NONE', *, *, #26416, .T. ) ;
#20323 = CARTESIAN_POINT ( 'NONE',  ( -0.7381027496704849478, 5.905511811023623991, -2.859439394060923956 ) ) ;
#20324 = EDGE_CURVE ( 'NONE', #22357, #21187, #35519, .T. ) ;
#20325 = VERTEX_POINT ( 'NONE', #28714 ) ;
#20326 = DIRECTION ( 'NONE',  ( -0.000000000000000000, 1.000000000000000000, -0.000000000000000000 ) ) ;
#20327 = CARTESIAN_POINT ( 'NONE',  ( -1.602125192864240821, 3.267716535433071279, -1.456692913385822186 ) ) ;
#20328 = VECTOR ( 'NONE', #31988, 39.37007874015748143 ) ;
#20329 = VERTEX_POINT ( 'NONE', #20461 ) ;
#20330 = VECTOR ( 'NONE', #46303, 39.37007874015748143 ) ;
#20331 = EDGE_CURVE ( 'NONE', #20408, #22204, #24853, .T. ) ;
#20332 = LINE ( 'NONE', #19809, #12531 ) ;
#20333 = ORIENTED_EDGE ( 'NONE', *, *, #28361, .T. ) ;
#20334 = CARTESIAN_POINT ( 'NONE',  ( 0.2727639067037604392, 3.346456692913386100, -0.3543307086614173040 ) ) ;
#20335 = VECTOR ( 'NONE', #22329, 39.37007874015748854 ) ;
#20336 = EDGE_CURVE ( 'NONE', #33248, #44681, #22630, .T. ) ;
#20337 = VERTEX_POINT ( 'NONE', #28966 ) ;
#20338 = VERTEX_POINT ( 'NONE', #16342 ) ;
#20339 = DIRECTION ( 'NONE',  ( 0.3930250316539147803, 0.000000000000000000, 0.9195277725514544587 ) ) ;
#20340 = AXIS2_PLACEMENT_3D ( 'NONE', #41672, #2936, #33435 ) ;
#20341 = DIRECTION ( 'NONE',  ( -0.000000000000000000, 1.000000000000000000, -0.000000000000000000 ) ) ;
#20342 = ORIENTED_EDGE ( 'NONE', *, *, #43309, .T. ) ;
#20343 = DIRECTION ( 'NONE',  ( -0.8345732537212999791, 0.000000000000000000, -0.5508969814521065267 ) ) ;
#20344 = EDGE_CURVE ( 'NONE', #11074, #5663, #36223, .T. ) ;
#20345 = ORIENTED_EDGE ( 'NONE', *, *, #21026, .F. ) ;
#20346 = LINE ( 'NONE', #5109, #23567 ) ;
#20347 = CARTESIAN_POINT ( 'NONE',  ( 0.2727639067037604947, 3.346456692913386100, 0.7874015748031454320 ) ) ;
#20348 = DIRECTION ( 'NONE',  ( 0.08963930890344089242, 0.000000000000000000, -0.9959742939952384022 ) ) ;
#20349 = B_SPLINE_CURVE_WITH_KNOTS ( 'NONE', 3,
 ( #21270, #37026, #44998, #9652 ),
 .UNSPECIFIED., .F., .F.,
 ( 4, 4 ),
 ( 6.559598655537315290E-07, 0.004930659607264709435 ),
 .UNSPECIFIED. ) ;
#20350 = EDGE_LOOP ( 'NONE', ( #33957, #47205 ) ) ;
#20351 = ORIENTED_EDGE ( 'NONE', *, *, #15630, .F. ) ;
#20352 = APPLICATION_CONTEXT ( 'automotive_design' ) ;
#20353 = CARTESIAN_POINT ( 'NONE',  ( 1.598711713508005117, 1.574803149606302854, -1.460438370699377986 ) ) ;
#20354 = CARTESIAN_POINT ( 'NONE',  ( 1.895640394390794459, 0.03825063239866469816, 0.6676760893130100349 ) ) ;
#20355 = CARTESIAN_POINT ( 'NONE',  ( -1.363819533518803473, 3.267716535433071279, 2.365849761790805980E-16 ) ) ;
#20356 = EDGE_CURVE ( 'NONE', #11815, #8216, #33520, .T. ) ;
#20357 = CARTESIAN_POINT ( 'NONE',  ( 2.339241080213585899, 1.462148010760873307, 1.802537235681917815 ) ) ;
#20358 = EDGE_CURVE ( 'NONE', #45000, #33320, #32874, .T. ) ;
#20359 = CARTESIAN_POINT ( 'NONE',  ( 0.4517796511351843680, 1.715138028758778521, 2.213898087213642007 ) ) ;
#20360 = CARTESIAN_POINT ( 'NONE',  ( -1.377952755905513360, 0.000000000000000000, 2.165354330708661568 ) ) ;
#20361 = ORIENTED_EDGE ( 'NONE', *, *, #4278, .T. ) ;
#20362 = AXIS2_PLACEMENT_3D ( 'NONE', #45744, #13520, #29257 ) ;
#20363 = FACE_OUTER_BOUND ( 'NONE', #35875, .T. ) ;
#20364 = ORIENTED_EDGE ( 'NONE', *, *, #45524, .T. ) ;
#20365 = AXIS2_PLACEMENT_3D ( 'NONE', #17196, #25191, #37075 ) ;
#20366 = DIRECTION ( 'NONE',  ( 1.734723475976806848E-16, -0.000000000000000000, 1.000000000000000000 ) ) ;
#20367 = ORIENTED_EDGE ( 'NONE', *, *, #1683, .F. ) ;
#20368 = EDGE_CURVE ( 'NONE', #38168, #44408, #4464, .T. ) ;
#20369 = DIRECTION ( 'NONE',  ( -0.000000000000000000, 1.000000000000000000, -0.000000000000000000 ) ) ;
#20370 = LINE ( 'NONE', #11604, #31983 ) ;
#20371 = CARTESIAN_POINT ( 'NONE',  ( -0.7832715154832613491, 0.000000000000000000, 0.8840183951921659622 ) ) ;
#20372 = LINE ( 'NONE', #20629, #37611 ) ;
#20373 = ORIENTED_EDGE ( 'NONE', *, *, #32691, .F. ) ;
#20374 = ADVANCED_FACE ( 'NONE', ( #20978 ), #12459, .F. ) ;
#20375 = B_SPLINE_CURVE_WITH_KNOTS ( 'NONE', 3,
 ( #20591, #48927, #16729, #32745 ),
 .UNSPECIFIED., .F., .F.,
 ( 4, 4 ),
 ( 0.04354068846991995811, 0.06157816714894258359 ),
 .UNSPECIFIED. ) ;
#20376 = CARTESIAN_POINT ( 'NONE',  ( -1.410501566226150638, 6.692913385826772199, 1.689247093817288548 ) ) ;
#20377 = FACE_BOUND ( 'NONE', #21107, .T. ) ;
#20378 = ORIENTED_EDGE ( 'NONE', *, *, #5404, .F. ) ;
#20379 = DIRECTION ( 'NONE',  ( -1.000000000000000000, -0.000000000000000000, -0.000000000000000000 ) ) ;
#20380 = AXIS2_PLACEMENT_3D ( 'NONE', #13887, #18523, #29636 ) ;
#20381 = ORIENTED_EDGE ( 'NONE', *, *, #5556, .F. ) ;
#20382 = CARTESIAN_POINT ( 'NONE',  ( -0.07591351300297333182, 3.267716535433071279, 2.362204724409437961 ) ) ;
#20383 = CARTESIAN_POINT ( 'NONE',  ( 2.803168581537432758, 1.762931689648581157, 0.9280530358755010312 ) ) ;
#20384 = CARTESIAN_POINT ( 'NONE',  ( -0.5272349255865267370, 0.000000000000000000, 2.905303903342410621 ) ) ;
#20385 = VERTEX_POINT ( 'NONE', #40857 ) ;
#20386 = ORIENTED_EDGE ( 'NONE', *, *, #6783, .F. ) ;
#20387 = CARTESIAN_POINT ( 'NONE',  ( 1.015142113812069313, 0.000000000000000000, -1.102362204724405714 ) ) ;
#20388 = CARTESIAN_POINT ( 'NONE',  ( 1.287906020515830363, 3.267716535433071279, -4.468321617281356063E-16 ) ) ;
#20389 = DIRECTION ( 'NONE',  ( -0.000000000000000000, -1.000000000000000000, -0.000000000000000000 ) ) ;
#20390 = FACE_OUTER_BOUND ( 'NONE', #15521, .T. ) ;
#20391 = CARTESIAN_POINT ( 'NONE',  ( -0.8182917201112814842, 0.000000000000000000, 0.4724409448818872592 ) ) ;
#20392 = VECTOR ( 'NONE', #33940, 39.37007874015748143 ) ;
#20393 = VECTOR ( 'NONE', #5958, 39.37007874015748143 ) ;
#20394 = EDGE_CURVE ( 'NONE', #41467, #39512, #36989, .T. ) ;
#20395 = ORIENTED_EDGE ( 'NONE', *, *, #27830, .F. ) ;
#20396 = DIRECTION ( 'NONE',  ( -1.000000000000000000, 0.000000000000000000, 0.000000000000000000 ) ) ;
#20397 = ORIENTED_EDGE ( 'NONE', *, *, #42782, .T. ) ;
#20398 = EDGE_LOOP ( 'NONE', ( #21465, #37372, #26837, #21136 ) ) ;
#20399 = PRODUCT_CONTEXT ( 'NONE', #40795, 'mechanical' ) ;
#20400 = EDGE_CURVE ( 'NONE', #45906, #22792, #36476, .T. ) ;
#20401 = VERTEX_POINT ( 'NONE', #48804 ) ;
#20402 = CARTESIAN_POINT ( 'NONE',  ( 0.7423782071083084855, 3.346456692913386100, -1.971134437475891454 ) ) ;
#20403 = DIRECTION ( 'NONE',  ( -1.000000000000000000, 0.000000000000000000, 1.734723475976806848E-16 ) ) ;
#20404 = EDGE_CURVE ( 'NONE', #1425, #18884, #40088, .T. ) ;
#20405 = ADVANCED_FACE ( 'NONE', ( #12722 ), #32351, .F. ) ;
#20406 = PLANE ( 'NONE',  #6352 ) ;
#20407 = DIRECTION ( 'NONE',  ( 0.000000000000000000, 0.000000000000000000, -1.000000000000000000 ) ) ;
#20408 = VERTEX_POINT ( 'NONE', #44204 ) ;
#20409 = ORIENTED_EDGE ( 'NONE', *, *, #41088, .F. ) ;
#20410 = LINE ( 'NONE', #32826, #8479 ) ;
#20411 = PLANE ( 'NONE',  #35376 ) ;
#20412 = FACE_OUTER_BOUND ( 'NONE', #15269, .T. ) ;
#20413 = AXIS2_PLACEMENT_3D ( 'NONE', #21577, #40947, #37333 ) ;
#20414 = DIRECTION ( 'NONE',  ( -0.9998717552508122886, -0.01601477604151182316, 0.000000000000000000 ) ) ;
#20415 = CARTESIAN_POINT ( 'NONE',  ( 0.5905511811023621549, 0.000000000000000000, -4.133858267716536083 ) ) ;
#20416 = CARTESIAN_POINT ( 'NONE',  ( -2.952069331832154919, 5.118110236220475784, -1.181102362204724310 ) ) ;
#20417 = ADVANCED_FACE ( 'NONE', ( #12982 ), #38009, .T. ) ;
#20418 = DIRECTION ( 'NONE',  ( 0.000000000000000000, 0.000000000000000000, -1.000000000000000000 ) ) ;
#20419 = DIRECTION ( 'NONE',  ( 0.000000000000000000, 1.000000000000000000, 0.000000000000000000 ) ) ;
#20420 = ORIENTED_EDGE ( 'NONE', *, *, #369, .F. ) ;
#20421 = CARTESIAN_POINT ( 'NONE',  ( -0.1692531782225912829, -0.6299212598425202314, 0.3335283217915853138 ) ) ;
#20422 = ORIENTED_EDGE ( 'NONE', *, *, #27106, .F. ) ;
#20424 = ORIENTED_EDGE ( 'NONE', *, *, #40647, .F. ) ;
#20423 = EDGE_CURVE ( 'NONE', #50372, #34255, #49321, .T. ) ;
#20425 = DIRECTION ( 'NONE',  ( -1.000000000000000000, 0.000000000000000000, 1.734723475976806848E-16 ) ) ;
#20426 = CARTESIAN_POINT ( 'NONE',  ( 0.000000000000000000, 3.267716535433071279, 0.2755905511810994302 ) ) ;
#20427 = DIRECTION ( 'NONE',  ( 0.000000000000000000, 0.000000000000000000, 1.000000000000000000 ) ) ;
#20428 = AXIS2_PLACEMENT_3D ( 'NONE', #32394, #29783, #41659 ) ;
#20429 = EDGE_LOOP ( 'NONE', ( #13365, #43927, #45089, #5718 ) ) ;
#20430 = AXIS2_PLACEMENT_3D ( 'NONE', #34298, #30418, #42277 ) ;
#20431 = EDGE_CURVE ( 'NONE', #46441, #919, #5740, .T. ) ;
#20432 = ADVANCED_FACE ( 'NONE', ( #41872 ), #23576, .T. ) ;
#20433 = EDGE_CURVE ( 'NONE', #26916, #2822, #37502, .T. ) ;
#20434 = ORIENTED_EDGE ( 'NONE', *, *, #27123, .F. ) ;
#20435 = FACE_OUTER_BOUND ( 'NONE', #32158, .T. ) ;
#20436 = VECTOR ( 'NONE', #33822, 39.37007874015748143 ) ;
#20437 = ORIENTED_EDGE ( 'NONE', *, *, #30970, .F. ) ;
#20438 = CARTESIAN_POINT ( 'NONE',  ( 0.000000000000000000, 3.267716535433071279, 0.000000000000000000 ) ) ;
#20439 = ORIENTED_EDGE ( 'NONE', *, *, #49081, .T. ) ;
#20440 = VECTOR ( 'NONE', #15295, 39.37007874015748143 ) ;
#20441 = CYLINDRICAL_SURFACE ( 'NONE', #24360, 2.165354330708661568 ) ;
#20442 = DIRECTION ( 'NONE',  ( 0.6234898018587431423, 1.288287287306305283E-16, -0.7818314824680221431 ) ) ;
#20443 = DIRECTION ( 'NONE',  ( 0.000000000000000000, 0.000000000000000000, -1.000000000000000000 ) ) ;
#20444 = VECTOR ( 'NONE', #39457, 39.37007874015748143 ) ;
#20445 = ORIENTED_EDGE ( 'NONE', *, *, #49691, .F. ) ;
#20446 = EDGE_LOOP ( 'NONE', ( #32002, #19254, #6189, #31594 ) ) ;
#20447 = ORIENTED_EDGE ( 'NONE', *, *, #17152, .F. ) ;
#20448 = DIRECTION ( 'NONE',  ( -1.000000000000000000, -0.000000000000000000, -0.000000000000000000 ) ) ;
#20449 = ORIENTED_EDGE ( 'NONE', *, *, #47475, .T. ) ;
#20450 = ORIENTED_EDGE ( 'NONE', *, *, #20656, .T. ) ;
#20451 = LINE ( 'NONE', #32089, #7506 ) ;
#20452 = DIRECTION ( 'NONE',  ( 1.000000000000000000, -0.000000000000000000, 0.000000000000000000 ) ) ;
#20453 = CARTESIAN_POINT ( 'NONE',  ( 0.6363476328836782381, 3.346456692913386100, 2.007874015748021268 ) ) ;
#20454 = AXIS2_PLACEMENT_3D ( 'NONE', #25126, #41894, #6535 ) ;
#20455 = EDGE_LOOP ( 'NONE', ( #39134, #44887, #32234, #38601 ) ) ;
#20456 = DIRECTION ( 'NONE',  ( -0.000000000000000000, 1.000000000000000000, -0.000000000000000000 ) ) ;
#20457 = DIRECTION ( 'NONE',  ( -0.000000000000000000, 1.000000000000000000, -0.000000000000000000 ) ) ;
#20458 = CARTESIAN_POINT ( 'NONE',  ( -0.2727639067037602172, 0.000000000000000000, 1.732283464566921172 ) ) ;
#20459 = ORIENTED_EDGE ( 'NONE', *, *, #27851, .T. ) ;
#20460 = CARTESIAN_POINT ( 'NONE',  ( -2.919165122154194769, 1.575328909575085090, 0.4450898352768660748 ) ) ;
#20461 = CARTESIAN_POINT ( 'NONE',  ( 2.823445274216730638, 2.755905511811027164, 0.8656477926280683466 ) ) ;
#20462 = EDGE_LOOP ( 'NONE', ( #13189, #27916 ) ) ;
#20463 = LINE ( 'NONE', #12212, #12598 ) ;
#20464 = VERTEX_POINT ( 'NONE', #18124 ) ;
#20465 = VERTEX_POINT ( 'NONE', #25609 ) ;
#20466 = DIRECTION ( 'NONE',  ( 0.2660368455666687892, -1.119010597708915320E-16, 0.9639628606958549062 ) ) ;
#20467 = DIRECTION ( 'NONE',  ( 0.000000000000000000, 0.000000000000000000, 1.000000000000000000 ) ) ;
#20468 = DIRECTION ( 'NONE',  ( 1.734723475976806848E-16, 0.000000000000000000, 1.000000000000000000 ) ) ;
#20469 = EDGE_CURVE ( 'NONE', #7160, #42304, #1863, .T. ) ;
#20470 = VECTOR ( 'NONE', #16716, 39.37007874015748143 ) ;
#20471 = EDGE_CURVE ( 'NONE', #30246, #50120, #37247, .T. ) ;
#20472 = DIRECTION ( 'NONE',  ( 1.734723475976806848E-16, -0.000000000000000000, 1.000000000000000000 ) ) ;
#20473 = CARTESIAN_POINT ( 'NONE',  ( 2.813306935135764242, 1.664615162603113818, 0.8968503919118566703 ) ) ;
#20474 = ORIENTED_EDGE ( 'NONE', *, *, #18867, .F. ) ;
#20476 = EDGE_CURVE ( 'NONE', #25478, #9639, #21488, .T. ) ;
#20475 = ORIENTED_EDGE ( 'NONE', *, *, #25611, .F. ) ;
#20477 = DIRECTION ( 'NONE',  ( 1.000000000000000000, 0.000000000000000000, 0.000000000000000000 ) ) ;
#20478 = VECTOR ( 'NONE', #40224, 39.37007874015748143 ) ;
#20479 = ORIENTED_EDGE ( 'NONE', *, *, #2140, .F. ) ;
#20480 = LINE ( 'NONE', #16616, #16210 ) ;
#20481 = CARTESIAN_POINT ( 'NONE',  ( 2.378961647330872786, 0.000000000000000000, -0.1968503937007886062 ) ) ;
#20482 = ADVANCED_FACE ( 'NONE', ( #41365 ), #5989, .F. ) ;
#20483 = AXIS2_PLACEMENT_3D ( 'NONE', #1416, #29028, #8398 ) ;
#20484 = VECTOR ( 'NONE', #50599, 39.37007874015748143 ) ;
#20485 = VECTOR ( 'NONE', #33769, 39.37007874015748143 ) ;
#20486 = DIRECTION ( 'NONE',  ( -0.000000000000000000, 1.000000000000000000, -0.000000000000000000 ) ) ;
#20487 = CARTESIAN_POINT ( 'NONE',  ( 0.2727639067037604947, 3.346456692913386100, 0.4724409448818868706 ) ) ;
#20488 = DIRECTION ( 'NONE',  ( -0.000000000000000000, 1.000000000000000000, -0.000000000000000000 ) ) ;
#20489 = VERTEX_POINT ( 'NONE', #41619 ) ;
#20490 = FACE_OUTER_BOUND ( 'NONE', #7737, .T. ) ;
#20491 = ADVANCED_FACE ( 'NONE', ( #33381 ), #49060, .F. ) ;
#20492 = VECTOR ( 'NONE', #8181, 39.37007874015748143 ) ;
#20493 = DIRECTION ( 'NONE',  ( -0.000000000000000000, -1.000000000000000000, -0.000000000000000000 ) ) ;
#20494 = ORIENTED_EDGE ( 'NONE', *, *, #42509, .F. ) ;
#20495 = LINE ( 'NONE', #3989, #23212 ) ;
#20496 = EDGE_CURVE ( 'NONE', #46412, #3654, #10121, .T. ) ;
#20497 = DIRECTION ( 'NONE',  ( 0.6910626489868580968, -1.160734090543304660E-16, 0.7227948638273978821 ) ) ;
#20498 = CARTESIAN_POINT ( 'NONE',  ( -0.4098391621113791072, 1.049866565877818347, 1.982786943858533268 ) ) ;
#20499 = ORIENTED_EDGE ( 'NONE', *, *, #27587, .T. ) ;
#20500 = DIRECTION ( 'NONE',  ( -0.000000000000000000, -1.000000000000000000, 0.000000000000000000 ) ) ;
#20501 = LINE ( 'NONE', #37280, #25021 ) ;
#20502 = EDGE_CURVE ( 'NONE', #30196, #39803, #34129, .T. ) ;
#20503 = CARTESIAN_POINT ( 'NONE',  ( -0.7381027496704855029, 1.707760278544290689, -2.859439394060923512 ) ) ;
#20504 = EDGE_CURVE ( 'NONE', #22686, #6017, #44733, .T. ) ;
#20505 = ORIENTED_EDGE ( 'NONE', *, *, #34511, .F. ) ;
#20506 = LINE ( 'NONE', #24379, #50178 ) ;
#20507 = FACE_OUTER_BOUND ( 'NONE', #9674, .T. ) ;
#20508 = ORIENTED_EDGE ( 'NONE', *, *, #47497, .T. ) ;
#20509 = EDGE_CURVE ( 'NONE', #11981, #18410, #45458, .T. ) ;
#20510 = DIRECTION ( 'NONE',  ( 0.7071067811865483499, -0.000000000000000000, -0.7071067811865466846 ) ) ;
#20511 = CARTESIAN_POINT ( 'NONE',  ( 1.015142113812069091, 3.346456692913386100, -2.047244094488181343 ) ) ;
#20512 = LINE ( 'NONE', #24127, #5754 ) ;
#20513 = CARTESIAN_POINT ( 'NONE',  ( 1.833433833923351353, 3.267716535433071279, -0.9448818897637765168 ) ) ;
#20514 = VECTOR ( 'NONE', #10234, 39.37007874015748143 ) ;
#20515 = B_SPLINE_CURVE_WITH_KNOTS ( 'NONE', 3,
 ( #7605, #49091, #44991, #44488 ),
 .UNSPECIFIED., .F., .F.,
 ( 4, 4 ),
 ( 2.472189648548164523E-07, 0.01923235726777020385 ),
 .UNSPECIFIED. ) ;
#20516 = ORIENTED_EDGE ( 'NONE', *, *, #44645, .F. ) ;
#20517 = ORIENTED_EDGE ( 'NONE', *, *, #10813, .F. ) ;
#20518 = FACE_OUTER_BOUND ( 'NONE', #39141, .T. ) ;
#20519 = DIRECTION ( 'NONE',  ( -0.000000000000000000, 1.000000000000000000, -0.000000000000000000 ) ) ;
#20520 = ORIENTED_EDGE ( 'NONE', *, *, #42560, .F. ) ;
#20521 = FACE_OUTER_BOUND ( 'NONE', #33526, .T. ) ;
#20522 = DIRECTION ( 'NONE',  ( -3.469446951953613696E-16, 0.000000000000000000, -1.000000000000000000 ) ) ;
#20523 = CARTESIAN_POINT ( 'NONE',  ( -1.909347346926324462, 3.267716535433071279, 0.4724409448818871482 ) ) ;
#20524 = FACE_OUTER_BOUND ( 'NONE', #43114, .T. ) ;
#20525 = AXIS2_PLACEMENT_3D ( 'NONE', #15065, #43430, #19425 ) ;
#20526 = VECTOR ( 'NONE', #23173, 39.37007874015748143 ) ;
#20527 = EDGE_LOOP ( 'NONE', ( #2509, #42270, #15174, #3881 ) ) ;
#20528 = ORIENTED_EDGE ( 'NONE', *, *, #16828, .T. ) ;
#20529 = CARTESIAN_POINT ( 'NONE',  ( 0.5455278134075211005, 3.346456692913386100, -0.8267716535433055070 ) ) ;
#20530 = CARTESIAN_POINT ( 'NONE',  ( 0.1067246931122726866, 0.02962905676920215767, 0.000000000000000000 ) ) ;
#20531 = CARTESIAN_POINT ( 'NONE',  ( 1.905060681038603265, 6.692913385826772199, 1.081042454612135773 ) ) ;
#20532 = FACE_OUTER_BOUND ( 'NONE', #49905, .T. ) ;
#20533 = FACE_BOUND ( 'NONE', #8457, .T. ) ;
#20534 = ORIENTED_EDGE ( 'NONE', *, *, #24129, .F. ) ;
#20535 = LINE ( 'NONE', #36548, #21634 ) ;
#20536 = ORIENTED_EDGE ( 'NONE', *, *, #49576, .T. ) ;
#20537 = ORIENTED_EDGE ( 'NONE', *, *, #29753, .T. ) ;
#20538 = VECTOR ( 'NONE', #7793, 39.37007874015748143 ) ;
#20539 = DIRECTION ( 'NONE',  ( -0.000000000000000000, 1.000000000000000000, -0.000000000000000000 ) ) ;
#20540 = ORIENTED_EDGE ( 'NONE', *, *, #45204, .F. ) ;
#20541 = ORIENTED_EDGE ( 'NONE', *, *, #7096, .F. ) ;
#20542 = LINE ( 'NONE', #28277, #47491 ) ;
#20543 = ORIENTED_EDGE ( 'NONE', *, *, #6588, .T. ) ;
#20544 = EDGE_CURVE ( 'NONE', #11143, #15306, #33884, .T. ) ;
#20545 = EDGE_CURVE ( 'NONE', #46587, #10178, #36386, .T. ) ;
#20546 = CARTESIAN_POINT ( 'NONE',  ( -2.165354330708661568, 1.673228346456695492, 0.08080958544675392874 ) ) ;
#20547 = CARTESIAN_POINT ( 'NONE',  ( 0.000000000000000000, 3.267716535433071279, 1.259842519685033357 ) ) ;
#20548 = EDGE_CURVE ( 'NONE', #13314, #11136, #33038, .T. ) ;
#20549 = DIRECTION ( 'NONE',  ( -1.000000000000000000, 0.000000000000000000, 0.000000000000000000 ) ) ;
#20550 = VECTOR ( 'NONE', #38060, 39.37007874015748143 ) ;
#20551 = FACE_OUTER_BOUND ( 'NONE', #18304, .T. ) ;
#20552 = CARTESIAN_POINT ( 'NONE',  ( -0.6214413264104939882, 3.267716535433071279, 0.4724409448818872592 ) ) ;
#20553 = DIRECTION ( 'NONE',  ( -8.021399753802077430E-17, -1.000000000000000000, -8.389726389140663754E-17 ) ) ;
#20554 = ORIENTED_EDGE ( 'NONE', *, *, #14244, .F. ) ;
#20555 = CARTESIAN_POINT ( 'NONE',  ( -0.2727639067037608278, 3.346456692913386100, -0.9842519685039344823 ) ) ;
#20556 = CARTESIAN_POINT ( 'NONE',  ( 1.025452293874513421, 0.3889243959228481651, -1.097585813245683717 ) ) ;
#20557 = CARTESIAN_POINT ( 'NONE',  ( 2.074049943651431693, 1.574803149606302854, 0.6221544894624233546 ) ) ;
#20558 = VECTOR ( 'NONE', #20726, 39.37007874015748143 ) ;
#20559 = ORIENTED_EDGE ( 'NONE', *, *, #31812, .F. ) ;
#20560 = CARTESIAN_POINT ( 'NONE',  ( -0.04921259842519688094, 0.02713143566191717967, 1.843522435433914142 ) ) ;
#20561 = EDGE_CURVE ( 'NONE', #17428, #728, #1524, .T. ) ;
#20562 = DIRECTION ( 'NONE',  ( -0.000000000000000000, 1.000000000000000000, -0.000000000000000000 ) ) ;
#20563 = ORIENTED_EDGE ( 'NONE', *, *, #8781, .F. ) ;
#20564 = FACE_OUTER_BOUND ( 'NONE', #22185, .T. ) ;
#20565 = CARTESIAN_POINT ( 'NONE',  ( 0.000000000000000000, 3.267716535433071279, -0.6692913385826760875 ) ) ;
#20566 = VECTOR ( 'NONE', #20755, 39.37007874015748143 ) ;
#20567 = CARTESIAN_POINT ( 'NONE',  ( 0.1968503937007877735, 3.267716535433071279, -6.829619984160670372E-17 ) ) ;
#20568 = EDGE_CURVE ( 'NONE', #18896, #695, #26284, .T. ) ;
#20569 = EDGE_CURVE ( 'NONE', #32131, #50834, #45123, .T. ) ;
#20570 = ORIENTED_EDGE ( 'NONE', *, *, #38884, .F. ) ;
#20571 = CARTESIAN_POINT ( 'NONE',  ( 0.000000000000000000, 3.267716535433071279, -2.443628662382284489 ) ) ;
#20572 = VECTOR ( 'NONE', #7181, 39.37007874015748143 ) ;
#20573 = EDGE_LOOP ( 'NONE', ( #23284, #49991, #29950, #6259 ) ) ;
#20574 = FACE_BOUND ( 'NONE', #44047, .T. ) ;
#20575 = FACE_OUTER_BOUND ( 'NONE', #33151, .T. ) ;
#20576 = LINE ( 'NONE', #28567, #25099 ) ;
#20577 = FACE_OUTER_BOUND ( 'NONE', #14618, .T. ) ;
#20578 = B_SPLINE_CURVE_WITH_KNOTS ( 'NONE', 3,
 ( #12329, #12846, #4843, #36338 ),
 .UNSPECIFIED., .F., .F.,
 ( 4, 4 ),
 ( 0.001272230606304385449, 0.04687302674643420430 ),
 .UNSPECIFIED. ) ;
#20579 = ORIENTED_EDGE ( 'NONE', *, *, #39029, .T. ) ;
#20580 = VERTEX_POINT ( 'NONE', #28369 ) ;
#20581 = CARTESIAN_POINT ( 'NONE',  ( 1.287906020515830141, 0.000000000000000000, 1.259842519685033357 ) ) ;
#20582 = VERTEX_POINT ( 'NONE', #48465 ) ;
#20583 = DIRECTION ( 'NONE',  ( 3.986037398843765983E-20, 1.000000000000000000, 1.160734090543304660E-16 ) ) ;
#20584 = ORIENTED_EDGE ( 'NONE', *, *, #8959, .F. ) ;
#20585 = LINE ( 'NONE', #39953, #7479 ) ;
#20586 = VECTOR ( 'NONE', #34868, 39.37007874015748143 ) ;
#20587 = VERTEX_POINT ( 'NONE', #36645 ) ;
#20588 = LINE ( 'NONE', #968, #26591 ) ;
#20589 = DIRECTION ( 'NONE',  ( -0.5877852522924684742, 0.000000000000000000, -0.8090169943749506709 ) ) ;
#20590 = EDGE_LOOP ( 'NONE', ( #28326, #25739, #6122, #37279 ) ) ;
#20591 = CARTESIAN_POINT ( 'NONE',  ( -0.04921259842519708216, 1.608688524157807498, 2.242709805336809303 ) ) ;
#20592 = VERTEX_POINT ( 'NONE', #9785 ) ;
#20593 = AXIS2_PLACEMENT_3D ( 'NONE', #49516, #1814, #29173 ) ;
#20594 = LINE ( 'NONE', #19812, #41897 ) ;
#20595 = ORIENTED_EDGE ( 'NONE', *, *, #11278, .F. ) ;
#20596 = ORIENTED_EDGE ( 'NONE', *, *, #45356, .F. ) ;
#20597 = DIRECTION ( 'NONE',  ( 0.000000000000000000, 1.000000000000000000, 0.000000000000000000 ) ) ;
#20598 = EDGE_CURVE ( 'NONE', #3086, #44277, #20372, .T. ) ;
#20599 = ORIENTED_EDGE ( 'NONE', *, *, #20994, .F. ) ;
#20600 = VECTOR ( 'NONE', #26661, 39.37007874015748143 ) ;
#20601 = CARTESIAN_POINT ( 'NONE',  ( 1.091055626815042867, 3.267716535433071279, -1.892679809432644882E-16 ) ) ;
#20602 = ORIENTED_EDGE ( 'NONE', *, *, #9181, .F. ) ;
#20603 = LINE ( 'NONE', #24227, #12897 ) ;
#20604 = EDGE_CURVE ( 'NONE', #17408, #36108, #25098, .T. ) ;
#20605 = CARTESIAN_POINT ( 'NONE',  ( 0.1067246931122726866, 0.02962905676920215767, 0.000000000000000000 ) ) ;
#20606 = EDGE_CURVE ( 'NONE', #24946, #18566, #16766, .T. ) ;
#20607 = B_SPLINE_CURVE_WITH_KNOTS ( 'NONE', 3,
 ( #33272, #6145, #5380, #37142 ),
 .UNSPECIFIED., .F., .F.,
 ( 4, 4 ),
 ( 0.1211873102087489551, 0.1625992483279400380 ),
 .UNSPECIFIED. ) ;
#20608 = EDGE_CURVE ( 'NONE', #39964, #43653, #21123, .T. ) ;
#20609 = FACE_OUTER_BOUND ( 'NONE', #11743, .T. ) ;
#20610 = ORIENTED_EDGE ( 'NONE', *, *, #39354, .F. ) ;
#20611 = CARTESIAN_POINT ( 'NONE',  ( 2.339241080213585899, 1.755713673067765379, 1.802537235681918037 ) ) ;
#20612 = FACE_OUTER_BOUND ( 'NONE', #42597, .T. ) ;
#20613 = DIRECTION ( 'NONE',  ( -3.469446951953613696E-16, 0.000000000000000000, -1.000000000000000000 ) ) ;
#20614 = CARTESIAN_POINT ( 'NONE',  ( 0.5455278134075216556, 3.346456692913386100, 1.377952755905504256 ) ) ;
#20615 = DIRECTION ( 'NONE',  ( -0.000000000000000000, 1.000000000000000000, -0.000000000000000000 ) ) ;
#20616 = CARTESIAN_POINT ( 'NONE',  ( -0.8942052331142547050, 0.000000000000000000, 1.574803149606291974 ) ) ;
#20617 = DIRECTION ( 'NONE',  ( -0.000000000000000000, 1.000000000000000000, -0.000000000000000000 ) ) ;
#20618 = EDGE_CURVE ( 'NONE', #10297, #45101, #25523, .T. ) ;
#20619 = EDGE_LOOP ( 'NONE', ( #27606, #41554, #50237, #24041 ) ) ;
#20620 = CYLINDRICAL_SURFACE ( 'NONE', #20970, 2.165354330708661568 ) ;
#20621 = ORIENTED_EDGE ( 'NONE', *, *, #16413, .F. ) ;
#20622 = DIRECTION ( 'NONE',  ( 1.000000000000000000, -0.000000000000000000, 0.000000000000000000 ) ) ;
#20623 = EDGE_CURVE ( 'NONE', #17342, #44964, #33286, .T. ) ;
#20624 = ORIENTED_EDGE ( 'NONE', *, *, #47141, .T. ) ;
#20625 = PLANE ( 'NONE',  #5263 ) ;
#20626 = CARTESIAN_POINT ( 'NONE',  ( 0.000000000000000000, 3.346456692913386100, 0.000000000000000000 ) ) ;
#20627 = CONICAL_SURFACE ( 'NONE', #2512, 2.246510896728926010, 0.01601546068027819014 ) ;
#20628 = DIRECTION ( 'NONE',  ( -0.000000000000000000, 1.000000000000000000, -0.000000000000000000 ) ) ;
#20629 = CARTESIAN_POINT ( 'NONE',  ( 0.000000000000000000, 3.267716535433071279, -1.574803149606293529 ) ) ;
#20630 = ORIENTED_EDGE ( 'NONE', *, *, #18867, .T. ) ;
#20631 = EDGE_CURVE ( 'NONE', #6824, #30018, #49927, .T. ) ;
#20632 = LINE ( 'NONE', #14161, #18353 ) ;
#20633 = FACE_BOUND ( 'NONE', #29973, .T. ) ;
#20634 = EDGE_LOOP ( 'NONE', ( #10489, #9042, #50986, #16775 ) ) ;
#20635 = CARTESIAN_POINT ( 'NONE',  ( 1.461363083917469829, 1.574803149606302854, 1.597866488315584865 ) ) ;
#20636 = AXIS2_PLACEMENT_3D ( 'NONE', #44625, #32535, #25026 ) ;
#20637 = EDGE_CURVE ( 'NONE', #17906, #47500, #44873, .T. ) ;
#20638 = ORIENTED_EDGE ( 'NONE', *, *, #40897, .F. ) ;
#20639 = CARTESIAN_POINT ( 'NONE',  ( -0.8182917201112819283, 0.000000000000000000, -0.6692913385826760875 ) ) ;
#20640 = LINE ( 'NONE', #1018, #48641 ) ;
#20641 = CARTESIAN_POINT ( 'NONE',  ( 0.000000000000000000, 1.574803149606302854, 0.000000000000000000 ) ) ;
#20642 = ORIENTED_EDGE ( 'NONE', *, *, #24420, .T. ) ;
#20643 = ORIENTED_EDGE ( 'NONE', *, *, #25995, .F. ) ;
#20644 = ADVANCED_FACE ( 'NONE', ( #9016 ), #48975, .F. ) ;
#20645 = DIRECTION ( 'NONE',  ( 0.000000000000000000, -1.000000000000000000, 0.000000000000000000 ) ) ;
#20646 = CARTESIAN_POINT ( 'NONE',  ( 1.091055626815042423, 3.346456692913386100, -1.574803149606294417 ) ) ;
#20647 = FACE_BOUND ( 'NONE', #29836, .T. ) ;
#20648 = CARTESIAN_POINT ( 'NONE',  ( 0.4696143004045484348, 3.346456692913386100, 0.9055118110236167750 ) ) ;
#20649 = CARTESIAN_POINT ( 'NONE',  ( -1.083598637574820334, 1.538470290252458739, 2.747180975113330259 ) ) ;
#20650 = ORIENTED_EDGE ( 'NONE', *, *, #8332, .F. ) ;
#20651 = LINE ( 'NONE', #1035, #198 ) ;
#20652 = EDGE_LOOP ( 'NONE', ( #10862, #4431, #22766, #44931 ) ) ;
#20653 = EDGE_LOOP ( 'NONE', ( #40123, #37628, #35953, #44188 ) ) ;
#20654 = ORIENTED_EDGE ( 'NONE', *, *, #39377, .T. ) ;
#20655 = DIRECTION ( 'NONE',  ( -0.000000000000000000, 1.000000000000000000, -0.000000000000000000 ) ) ;
#20656 = EDGE_CURVE ( 'NONE', #14441, #43305, #5138, .T. ) ;
#20657 = AXIS2_PLACEMENT_3D ( 'NONE', #35914, #20670, #1310 ) ;
#20658 = DIRECTION ( 'NONE',  ( 1.734723475976806848E-16, 0.000000000000000000, 1.000000000000000000 ) ) ;
#20659 = VECTOR ( 'NONE', #35301, 39.37007874015748143 ) ;
#20660 = FACE_OUTER_BOUND ( 'NONE', #22708, .T. ) ;
#20661 = EDGE_CURVE ( 'NONE', #48582, #17616, #8754, .T. ) ;
#20662 = CARTESIAN_POINT ( 'NONE',  ( 2.505429192702631536, 1.652952030840073805, 0.3890454956553852650 ) ) ;
#20663 = VERTEX_POINT ( 'NONE', #24510 ) ;
#20664 = VERTEX_POINT ( 'NONE', #40261 ) ;
#20665 = FACE_OUTER_BOUND ( 'NONE', #28358, .T. ) ;
#20666 = PLANE ( 'NONE',  #18068 ) ;
#20667 = DIRECTION ( 'NONE',  ( 0.000000000000000000, 0.000000000000000000, 1.000000000000000000 ) ) ;
#20668 = AXIS2_PLACEMENT_3D ( 'NONE', #34748, #27238, #46832 ) ;
#20669 = CARTESIAN_POINT ( 'NONE',  ( 1.287906020515829919, 3.249608194809333384, -2.086614173228340086 ) ) ;
#20670 = DIRECTION ( 'NONE',  ( -1.000000000000000000, 0.000000000000000000, 1.734723475976806848E-16 ) ) ;
#20671 = CARTESIAN_POINT ( 'NONE',  ( 1.909347346926324684, 0.000000000000000000, 0.4724409448818868706 ) ) ;
#20672 = CARTESIAN_POINT ( 'NONE',  ( -1.363819533518803473, 0.000000000000000000, 1.535433070866133232 ) ) ;
#20673 = CARTESIAN_POINT ( 'NONE',  ( -0.2727639067037610499, 3.346456692913386100, -2.047244094488181343 ) ) ;
#20674 = ORIENTED_EDGE ( 'NONE', *, *, #28016, .T. ) ;
#20675 = CARTESIAN_POINT ( 'NONE',  ( 1.287906020515830141, 0.000000000000000000, -0.5118110236220471121 ) ) ;
#20676 = LINE ( 'NONE', #32575, #47444 ) ;
#20677 = VERTEX_POINT ( 'NONE', #20884 ) ;
#20678 = ORIENTED_EDGE ( 'NONE', *, *, #16363, .F. ) ;
#20679 = PLANE ( 'NONE',  #18323 ) ;
#20680 = LINE ( 'NONE', #11916, #47555 ) ;
#20681 = CARTESIAN_POINT ( 'NONE',  ( 0.04921259842519689481, 1.205361022782829114E-17, 2.952755905511811108 ) ) ;
#20682 = EDGE_LOOP ( 'NONE', ( #5338, #36659, #19062 ) ) ;
#20683 = EDGE_CURVE ( 'NONE', #49793, #10381, #30439, .T. ) ;
#20684 = ORIENTED_EDGE ( 'NONE', *, *, #14847, .T. ) ;
#20685 = DIRECTION ( 'NONE',  ( 0.000000000000000000, 1.160734090543304660E-16, -1.000000000000000000 ) ) ;
#20686 = VERTEX_POINT ( 'NONE', #4886 ) ;
#20687 = ADVANCED_FACE ( 'NONE', ( #37412 ), #18288, .F. ) ;
#20688 = ORIENTED_EDGE ( 'NONE', *, *, #18618, .T. ) ;
#20689 = VECTOR ( 'NONE', #32768, 39.37007874015748143 ) ;
#20690 = DIRECTION ( 'NONE',  ( -0.000000000000000000, 0.000000000000000000, 1.000000000000000000 ) ) ;
#20691 = DIRECTION ( 'NONE',  ( 1.000000000000000000, 0.000000000000000000, 0.000000000000000000 ) ) ;
#20692 = PLANE ( 'NONE',  #18619 ) ;
#20693 = VECTOR ( 'NONE', #25229, 39.37007874015748143 ) ;
#20694 = EDGE_CURVE ( 'NONE', #40166, #43305, #18797, .T. ) ;
#20695 = EDGE_CURVE ( 'NONE', #36994, #21756, #2036, .T. ) ;
#20696 = ORIENTED_EDGE ( 'NONE', *, *, #47787, .T. ) ;
#20697 = ORIENTED_EDGE ( 'NONE', *, *, #39185, .F. ) ;
#20698 = ORIENTED_EDGE ( 'NONE', *, *, #14793, .T. ) ;
#20699 = CARTESIAN_POINT ( 'NONE',  ( -2.793030215715272213, 1.675725205278408403, 0.9592557174602281966 ) ) ;
#20700 = EDGE_LOOP ( 'NONE', ( #44944, #48515, #5680, #12387 ) ) ;
#20701 = ORIENTED_EDGE ( 'NONE', *, *, #36290, .F. ) ;
#20702 = ADVANCED_FACE ( 'NONE', ( #22169 ), #10543, .F. ) ;
#20703 = DIRECTION ( 'NONE',  ( 1.000000000000000000, 0.000000000000000000, -3.469446951953613696E-16 ) ) ;
#20704 = PLANE ( 'NONE',  #4638 ) ;
#20705 = AXIS2_PLACEMENT_3D ( 'NONE', #21038, #12518, #9159 ) ;
#20706 = CARTESIAN_POINT ( 'NONE',  ( 1.833433833923351353, 3.346456692913386100, -1.259842519685035800 ) ) ;
#20707 = EDGE_CURVE ( 'NONE', #45906, #4245, #41783, .T. ) ;
#20708 = AXIS2_PLACEMENT_3D ( 'NONE', #9195, #21841, #37593 ) ;
#20709 = ORIENTED_EDGE ( 'NONE', *, *, #10988, .F. ) ;
#20710 = CARTESIAN_POINT ( 'NONE',  ( 2.138597145901430352, 6.692913385826772199, 0.3393547186367261159 ) ) ;
#20711 = LINE ( 'NONE', #32608, #43086 ) ;
#20712 = DIRECTION ( 'NONE',  ( -1.000000000000000000, 0.000000000000000000, 0.000000000000000000 ) ) ;
#20713 = EDGE_LOOP ( 'NONE', ( #35074, #49414, #16815, #28076 ) ) ;
#20714 = DIRECTION ( 'NONE',  ( -0.000000000000000000, 1.000000000000000000, -0.000000000000000000 ) ) ;
#20715 = CARTESIAN_POINT ( 'NONE',  ( -0.7447559422295143561, 0.01073262845819722075, -1.659925117323180599 ) ) ;
#20716 = CARTESIAN_POINT ( 'NONE',  ( 0.000000000000000000, 0.4235180831842794702, -1.062992125984252301 ) ) ;
#20717 = EDGE_LOOP ( 'NONE', ( #22782, #17806, #20445, #43484 ) ) ;
#20718 = VERTEX_POINT ( 'NONE', #29908 ) ;
#20719 = CARTESIAN_POINT ( 'NONE',  ( 1.287906020515830141, 3.267716535433071279, 0.7480314960629872445 ) ) ;
#20720 = CARTESIAN_POINT ( 'NONE',  ( -0.8241443283111672402, 1.596276574288824301, 2.055867440327626916 ) ) ;
#20721 = B_SPLINE_CURVE_WITH_KNOTS ( 'NONE', 3,
 ( #22463, #37967, #42080, #41576 ),
 .UNSPECIFIED., .F., .F.,
 ( 4, 4 ),
 ( 2.074912098696191126E-07, 0.01852445910376516319 ),
 .UNSPECIFIED. ) ;
#20722 = ADVANCED_FACE ( 'NONE', ( #6420 ), #42279, .F. ) ;
#20723 = CARTESIAN_POINT ( 'NONE',  ( 1.363819533518803251, 0.000000000000000000, -0.4724409448818889246 ) ) ;
#20724 = CARTESIAN_POINT ( 'NONE',  ( 0.1968503937007878568, 0.000000000000000000, 2.204724409448808764 ) ) ;
#20725 = ADVANCED_FACE ( 'NONE', ( #29658, #34046 ), #2544, .F. ) ;
#20726 = DIRECTION ( 'NONE',  ( 1.734723475976806848E-16, -0.000000000000000000, 1.000000000000000000 ) ) ;
#20727 = EDGE_LOOP ( 'NONE', ( #34329, #37618, #7324, #18879 ) ) ;
#20728 = ORIENTED_EDGE ( 'NONE', *, *, #14022, .T. ) ;
#20729 = EDGE_CURVE ( 'NONE', #35776, #41844, #45376, .T. ) ;
#20730 = CARTESIAN_POINT ( 'NONE',  ( -0.8182917201112819283, 0.000000000000000000, -2.047244094488181343 ) ) ;
#20731 = PRODUCT_DEFINITION_SHAPE ( 'NONE', 'NONE',  #4815 ) ;
#20732 = ORIENTED_EDGE ( 'NONE', *, *, #43415, .T. ) ;
#20733 = CARTESIAN_POINT ( 'NONE',  ( 2.295325967725798222, 1.744665796922353351, 0.3605850800666594580 ) ) ;
#20734 = CARTESIAN_POINT ( 'NONE',  ( -1.062992125984252079, 0.000000000000000000, -1.014069264286642014 ) ) ;
#20735 = CIRCLE ( 'NONE', #11658, 2.165354330708661568 ) ;
#20736 = VECTOR ( 'NONE', #19243, 39.37007874015748143 ) ;
#20737 = CARTESIAN_POINT ( 'NONE',  ( 2.951990591674675368, 1.666783180044518087, -0.08331184815398359755 ) ) ;
#20738 = CARTESIAN_POINT ( 'NONE',  ( 2.165460538733997353, 0.000000000000000000, 0.04798874274655835076 ) ) ;
#20740 = DIRECTION ( 'NONE',  ( -3.469446951953613696E-16, 0.000000000000000000, -1.000000000000000000 ) ) ;
#20739 = VECTOR ( 'NONE', #6301, 39.37007874015748143 ) ;
#20741 = VERTEX_POINT ( 'NONE', #45879 ) ;
#20742 = CARTESIAN_POINT ( 'NONE',  ( -2.043634885149970160, 6.692913385826772199, 0.7157624142945935297 ) ) ;
#20743 = AXIS2_PLACEMENT_3D ( 'NONE', #49499, #3314, #10307 ) ;
#20744 = CARTESIAN_POINT ( 'NONE',  ( 1.905671854841463952, 5.905511811023623991, 2.256015092822682089 ) ) ;
#20745 = ORIENTED_EDGE ( 'NONE', *, *, #32740, .F. ) ;
#20746 = AXIS2_PLACEMENT_3D ( 'NONE', #26896, #18910, #38784 ) ;
#20747 = CARTESIAN_POINT ( 'NONE',  ( 1.091055626815042645, 3.346456692913386100, 0.6299212598425161236 ) ) ;
#20748 = CARTESIAN_POINT ( 'NONE',  ( 1.083598637574782142, 1.637691314537677023, 2.747180975113346246 ) ) ;
#20749 = CARTESIAN_POINT ( 'NONE',  ( -1.909347346926324462, 3.346456692913386100, 1.102362204724404160 ) ) ;
#20750 = VERTEX_POINT ( 'NONE', #14416 ) ;
#20751 = CARTESIAN_POINT ( 'NONE',  ( -1.735354274664482110, 1.614490279294756192, 1.320953578359251424 ) ) ;
#20752 = LINE ( 'NONE', #8627, #48893 ) ;
#20753 = CARTESIAN_POINT ( 'NONE',  ( -1.238969615956150738, 0.5248216437167342319, -1.789020852678176121 ) ) ;
#20754 = ORIENTED_EDGE ( 'NONE', *, *, #40290, .T. ) ;
#20755 = DIRECTION ( 'NONE',  ( -3.469446951953613696E-16, 0.000000000000000000, -1.000000000000000000 ) ) ;
#20756 = DIRECTION ( 'NONE',  ( -0.000000000000000000, 1.000000000000000000, -0.000000000000000000 ) ) ;
#20757 = VERTEX_POINT ( 'NONE', #18546 ) ;
#20758 = LINE ( 'NONE', #32914, #33646 ) ;
#20759 = CARTESIAN_POINT ( 'NONE',  ( 0.000000000000000000, 3.267716535433071279, -1.299212598425193210 ) ) ;
#20760 = CARTESIAN_POINT ( 'NONE',  ( -0.5455278134075211005, 3.267716535433071279, 9.463399047163219482E-17 ) ) ;
#20761 = LINE ( 'NONE', #36521, #47389 ) ;
#20762 = EDGE_CURVE ( 'NONE', #1205, #48217, #21654, .T. ) ;
#20763 = B_SPLINE_CURVE_WITH_KNOTS ( 'NONE', 3,
 ( #16799, #20662, #47480, #44149 ),
 .UNSPECIFIED., .F., .F.,
 ( 4, 4 ),
 ( 0.01482598341399509086, 0.03075144114903187453 ),
 .UNSPECIFIED. ) ;
#20764 = EDGE_CURVE ( 'NONE', #26292, #41090, #2727, .T. ) ;
#20765 = EDGE_CURVE ( 'NONE', #50597, #2602, #33799, .T. ) ;
#20766 = CARTESIAN_POINT ( 'NONE',  ( 0.8182917201112817063, 3.267716535433071279, -1.929133858267711110 ) ) ;
#20767 = EDGE_LOOP ( 'NONE', ( #19074, #41760, #33213, #32983 ) ) ;
#20768 = ORIENTED_EDGE ( 'NONE', *, *, #16779, .T. ) ;
#20769 = DIRECTION ( 'NONE',  ( -3.469446951953613696E-16, 0.000000000000000000, -1.000000000000000000 ) ) ;
#20770 = FACE_OUTER_BOUND ( 'NONE', #48586, .T. ) ;
#20771 = ORIENTED_EDGE ( 'NONE', *, *, #50395, .F. ) ;
#20772 = LINE ( 'NONE', #13036, #34102 ) ;
#20773 = CARTESIAN_POINT ( 'NONE',  ( 4.268512490100411402E-16, 3.346456692913386100, 2.204724409448808764 ) ) ;
#20774 = DIRECTION ( 'NONE',  ( -0.000000000000000000, 1.000000000000000000, -0.000000000000000000 ) ) ;
#20775 = VECTOR ( 'NONE', #355, 39.37007874015748143 ) ;
#20776 = LINE ( 'NONE', #14494, #5053 ) ;
#20777 = ORIENTED_EDGE ( 'NONE', *, *, #16668, .F. ) ;
#20778 = AXIS2_PLACEMENT_3D ( 'NONE', #22001, #45714, #14241 ) ;
#20779 = ORIENTED_EDGE ( 'NONE', *, *, #43835, .T. ) ;
#20780 = LINE ( 'NONE', #44268, #39461 ) ;
#20781 = DIRECTION ( 'NONE',  ( -0.000000000000000000, 1.000000000000000000, -0.000000000000000000 ) ) ;
#20782 = CARTESIAN_POINT ( 'NONE',  ( -0.04921259842519689481, 0.01808868210717232833, 1.870356923343539979 ) ) ;
#20783 = ORIENTED_EDGE ( 'NONE', *, *, #3391, .T. ) ;
#20784 = DIRECTION ( 'NONE',  ( -0.000000000000000000, 1.000000000000000000, -0.000000000000000000 ) ) ;
#20785 = VECTOR ( 'NONE', #18681, 39.37007874015748143 ) ;
#20786 = FACE_BOUND ( 'NONE', #12196, .T. ) ;
#20787 = ORIENTED_EDGE ( 'NONE', *, *, #27004, .F. ) ;
#20788 = CARTESIAN_POINT ( 'NONE',  ( 0.7423782071083092626, 0.000000000000000000, 2.204724409448808764 ) ) ;
#20789 = ORIENTED_EDGE ( 'NONE', *, *, #27278, .T. ) ;
#20790 = AXIS2_PLACEMENT_3D ( 'NONE', #34512, #50194, #3010 ) ;
#20791 = ORIENTED_EDGE ( 'NONE', *, *, #41315, .F. ) ;
#20792 = B_SPLINE_CURVE_WITH_KNOTS ( 'NONE', 3,
 ( #40503, #44859, #21137, #48204 ),
 .UNSPECIFIED., .F., .F.,
 ( 4, 4 ),
 ( 0.1211873102087489551, 0.1625992483279400380 ),
 .UNSPECIFIED. ) ;
#20793 = EDGE_CURVE ( 'NONE', #13815, #38409, #25777, .T. ) ;
#20794 = CARTESIAN_POINT ( 'NONE',  ( -1.091055626815042645, 3.267716535433071279, -2.086614173228339641 ) ) ;
#20795 = AXIS2_PLACEMENT_3D ( 'NONE', #44048, #48398, #170 ) ;
#20796 = ADVANCED_FACE ( 'NONE', ( #49986 ), #41281, .F. ) ;
#20797 = ORIENTED_EDGE ( 'NONE', *, *, #34828, .F. ) ;
#20798 = VERTEX_POINT ( 'NONE', #14670 ) ;
#20799 = CARTESIAN_POINT ( 'NONE',  ( -0.8182917201112819283, 3.346456692913386100, -0.7874015748031467643 ) ) ;
#20800 = EDGE_CURVE ( 'NONE', #4205, #28641, #30421, .T. ) ;
#20801 = ORIENTED_EDGE ( 'NONE', *, *, #46451, .T. ) ;
#20802 = EDGE_CURVE ( 'NONE', #36182, #22163, #26533, .T. ) ;
#20803 = CARTESIAN_POINT ( 'NONE',  ( 0.1968503937007872462, 0.000000000000000000, -1.456692913385822630 ) ) ;
#20804 = DIRECTION ( 'NONE',  ( 0.6910626489868580968, -8.392480990704469866E-17, 0.7227948638273978821 ) ) ;
#20805 = PLANE ( 'NONE',  #15176 ) ;
#20806 = FACE_OUTER_BOUND ( 'NONE', #31466, .T. ) ;
#20807 = B_SPLINE_CURVE_WITH_KNOTS ( 'NONE', 3,
 ( #43411, #43664, #35941, #32076 ),
 .UNSPECIFIED., .F., .F.,
 ( 4, 4 ),
 ( 3.882109077968705590E-07, 0.04390313747348802836 ),
 .UNSPECIFIED. ) ;
#20808 = DIRECTION ( 'NONE',  ( -4.561975526775602830E-17, -1.000000000000000000, -1.067327232801823148E-16 ) ) ;
#20809 = CARTESIAN_POINT ( 'NONE',  ( -0.9302092402134520821, 3.346456692913386100, -1.889763779527552146 ) ) ;
#20810 = VERTEX_POINT ( 'NONE', #5903 ) ;
#20811 = CARTESIAN_POINT ( 'NONE',  ( -2.182111253630085734, 0.000000000000000000, -0.6299212598425177889 ) ) ;
#20812 = CARTESIAN_POINT ( 'NONE',  ( -0.5455278134075214336, 3.346456692913386100, 2.034427629037600660 ) ) ;
#20813 = ORIENTED_EDGE ( 'NONE', *, *, #12975, .F. ) ;
#20814 = AXIS2_PLACEMENT_3D ( 'NONE', #4395, #35639, #24276 ) ;
#20815 = DIRECTION ( 'NONE',  ( 0.000000000000000000, 0.000000000000000000, -1.000000000000000000 ) ) ;
#20816 = FACE_OUTER_BOUND ( 'NONE', #24823, .T. ) ;
#20817 = ORIENTED_EDGE ( 'NONE', *, *, #12572, .T. ) ;
#20818 = CARTESIAN_POINT ( 'NONE',  ( 2.808237744965994320, 0.000000000000000000, 0.9124517550441679781 ) ) ;
#20819 = DIRECTION ( 'NONE',  ( 0.9510565162951545304, 0.000000000000000000, -0.3090169943749447867 ) ) ;
#20820 = CARTESIAN_POINT ( 'NONE',  ( 2.378961647330872786, 3.346456692913386100, 0.1181102362204698858 ) ) ;
#20821 = CIRCLE ( 'NONE', #19144, 2.106299212598425008 ) ;
#20822 = EDGE_LOOP ( 'NONE', ( #44179, #3197, #10602, #32414 ) ) ;
#20823 = AXIS2_PLACEMENT_3D ( 'NONE', #3705, #38576, #34697 ) ;
#20824 = LINE ( 'NONE', #36324, #41437 ) ;
#20825 = VERTEX_POINT ( 'NONE', #44020 ) ;
#20826 = FACE_BOUND ( 'NONE', #39558, .T. ) ;
#20827 = DIRECTION ( 'NONE',  ( 1.734723475976806848E-16, 0.000000000000000000, 1.000000000000000000 ) ) ;
#20828 = VECTOR ( 'NONE', #25626, 39.37007874015748143 ) ;
#20829 = VECTOR ( 'NONE', #28406, 39.37007874015748143 ) ;
#20830 = DIRECTION ( 'NONE',  ( -1.156482317317871478E-16, 0.000000000000000000, -1.000000000000000000 ) ) ;
#20831 = DIRECTION ( 'NONE',  ( 1.000000000000000000, 0.000000000000000000, 0.000000000000000000 ) ) ;
#20832 = B_SPLINE_CURVE_WITH_KNOTS ( 'NONE', 3,
 ( #43470, #48086, #48593, #4760 ),
 .UNSPECIFIED., .F., .F.,
 ( 4, 4 ),
 ( 0.1211775127643062444, 0.1625894504277921315 ),
 .UNSPECIFIED. ) ;
#20833 = ADVANCED_FACE ( 'NONE', ( #36041 ), #5050, .F. ) ;
#20834 = ORIENTED_EDGE ( 'NONE', *, *, #36592, .T. ) ;
#20835 = VERTEX_POINT ( 'NONE', #28025 ) ;
#20836 = ADVANCED_FACE ( 'NONE', ( #31397 ), #15371, .T. ) ;
#20837 = PLANE ( 'NONE',  #37857 ) ;
#20838 = ORIENTED_EDGE ( 'NONE', *, *, #21574, .T. ) ;
#20839 = LINE ( 'NONE', #4841, #49928 ) ;
#20840 = VERTEX_POINT ( 'NONE', #24418 ) ;
#20841 = EDGE_CURVE ( 'NONE', #29961, #33629, #13753, .T. ) ;
#20842 = CARTESIAN_POINT ( 'NONE',  ( 0.08139965876239094178, 1.610780518492231694, 0.000000000000000000 ) ) ;
#20843 = EDGE_LOOP ( 'NONE', ( #16135, #43939, #16767, #37053 ) ) ;
#20844 = FACE_OUTER_BOUND ( 'NONE', #3281, .T. ) ;
#20845 = CARTESIAN_POINT ( 'NONE',  ( 0.5455278134075212115, 3.346456692913386100, 0.9448818897637746295 ) ) ;
#20846 = ORIENTED_EDGE ( 'NONE', *, *, #33596, .F. ) ;
#20847 = LINE ( 'NONE', #45087, #46301 ) ;
#20848 = VERTEX_POINT ( 'NONE', #24161 ) ;
#20849 = EDGE_CURVE ( 'NONE', #16745, #27664, #48122, .T. ) ;
#20850 =( BOUNDED_CURVE ( )  B_SPLINE_CURVE ( 3, ( #22531, #23531, #38786, #42648 ),
 .UNSPECIFIED., .F., .F. ) 
 B_SPLINE_CURVE_WITH_KNOTS ( ( 4, 4 ),
 ( 4.856797154144195439, 4.907729085828183457 ),
 .UNSPECIFIED. ) 
 CURVE ( )  GEOMETRIC_REPRESENTATION_ITEM ( )  RATIONAL_B_SPLINE_CURVE ( ( 1.000000000000000000, 0.9997838398768879031, 0.9997838398768879031, 1.000000000000000000 ) ) 
 REPRESENTATION_ITEM ( '' )  );
#20851 = VERTEX_POINT ( 'NONE', #16421 ) ;
#20852 = ORIENTED_EDGE ( 'NONE', *, *, #22253, .F. ) ;
#20853 = CARTESIAN_POINT ( 'NONE',  ( 0.000000000000000000, 3.267716535433071279, -0.3543307086614175816 ) ) ;
#20854 = CIRCLE ( 'NONE', #5185, 2.246510896728926010 ) ;
#20855 = ADVANCED_FACE ( 'NONE', ( #47351 ), #664, .F. ) ;
#20856 = VERTEX_POINT ( 'NONE', #23642 ) ;
#20857 = CARTESIAN_POINT ( 'NONE',  ( 0.2156685157584260770, 1.722625337188476546, -2.945280361644574185 ) ) ;
#20858 = EDGE_LOOP ( 'NONE', ( #27122, #5768, #6847, #31816 ) ) ;
#20859 = DIRECTION ( 'NONE',  ( 0.9998717552508121775, 0.01601477604151182663, 0.000000000000000000 ) ) ;
#20860 = VECTOR ( 'NONE', #25815, 39.37007874015748143 ) ;
#20861 = VECTOR ( 'NONE', #15471, 39.37007874015748143 ) ;
#20862 = B_SPLINE_CURVE_WITH_KNOTS ( 'NONE', 3,
 ( #20988, #16610, #47546, #1104 ),
 .UNSPECIFIED., .F., .F.,
 ( 4, 4 ),
 ( 6.340610770647737117E-07, 0.002830502821758625054 ),
 .UNSPECIFIED. ) ;
#20863 = DIRECTION ( 'NONE',  ( -1.000000000000000000, -0.000000000000000000, -0.000000000000000000 ) ) ;
#20864 = ORIENTED_EDGE ( 'NONE', *, *, #23578, .T. ) ;
#20865 = CARTESIAN_POINT ( 'NONE',  ( -1.166969139818016199, 3.346456692913386100, -0.3543307086614174151 ) ) ;
#20866 = CARTESIAN_POINT ( 'NONE',  ( 1.091055626815042645, 3.267716535433071279, 0.4330708661417287386 ) ) ;
#20867 = VECTOR ( 'NONE', #48696, 39.37007874015748854 ) ;
#20868 = CARTESIAN_POINT ( 'NONE',  ( 2.576863348864710801, 1.759415398959654819, 1.442554885838449819 ) ) ;
#20869 = PLANE ( 'NONE',  #16742 ) ;
#20870 = CARTESIAN_POINT ( 'NONE',  ( 0.8182917201112819283, 3.267716535433071279, -0.4724409448818889246 ) ) ;
#20871 = CARTESIAN_POINT ( 'NONE',  ( -1.427293369312925497, 0.000000000000000000, -1.001115484471666761 ) ) ;
#20872 = CARTESIAN_POINT ( 'NONE',  ( -1.483604961240789333, -2.043891966111581001E-16, 1.623324365321668239 ) ) ;
#20873 = VERTEX_POINT ( 'NONE', #4282 ) ;
#20874 = DIRECTION ( 'NONE',  ( 1.000000000000000000, 0.000000000000000000, -1.156482317317871478E-16 ) ) ;
#20875 = DIRECTION ( 'NONE',  ( -0.01601477604151182663, 0.9998717552508123996, -0.000000000000000000 ) ) ;
#20876 = DIMENSIONAL_EXPONENTS ( 1.000000000000000000, 0.000000000000000000, 0.000000000000000000, 0.000000000000000000, 0.000000000000000000, 0.000000000000000000, 0.000000000000000000 ) ;
#20877 = ORIENTED_EDGE ( 'NONE', *, *, #7042, .T. ) ;
#20878 = DIRECTION ( 'NONE',  ( -0.000000000000000000, -1.000000000000000000, 0.000000000000000000 ) ) ;
#20879 = ORIENTED_EDGE ( 'NONE', *, *, #20765, .F. ) ;
#20880 = CARTESIAN_POINT ( 'NONE',  ( 1.636583440222563635, 3.346456692913386100, -1.141732283464564013 ) ) ;
#20881 = FACE_OUTER_BOUND ( 'NONE', #336, .T. ) ;
#20882 = CARTESIAN_POINT ( 'NONE',  ( -1.930378847111418050, 1.590732546136234937, 2.234429243736988813 ) ) ;
#20883 = DIRECTION ( 'NONE',  ( 0.000000000000000000, 0.000000000000000000, 1.000000000000000000 ) ) ;
#20884 = CARTESIAN_POINT ( 'NONE',  ( 0.3664524127070866721, 2.755905511811024056, 0.07483588040983164824 ) ) ;
#20885 = ORIENTED_EDGE ( 'NONE', *, *, #45500, .T. ) ;
#20886 = CARTESIAN_POINT ( 'NONE',  ( 0.8067290215917978236, 6.692913385826772199, 2.009464521518182334 ) ) ;
#20887 = VECTOR ( 'NONE', #15006, 39.37007874015748143 ) ;
#20888 = EDGE_CURVE ( 'NONE', #30219, #47632, #39652, .T. ) ;
#20889 = FACE_BOUND ( 'NONE', #14845, .T. ) ;
#20890 = ADVANCED_FACE ( 'NONE', ( #16680 ), #11768, .F. ) ;
#20891 = ORIENTED_EDGE ( 'NONE', *, *, #14445, .T. ) ;
#20892 = LINE ( 'NONE', #44378, #36188 ) ;
#20893 = VECTOR ( 'NONE', #43466, 39.37007874015748143 ) ;
#20894 = ORIENTED_EDGE ( 'NONE', *, *, #1471, .F. ) ;
#20895 = EDGE_CURVE ( 'NONE', #21029, #24, #44284, .T. ) ;
#20896 = VECTOR ( 'NONE', #50428, 39.37007874015748143 ) ;
#20897 = VECTOR ( 'NONE', #4994, 39.37007874015748143 ) ;
#20898 = DIRECTION ( 'NONE',  ( -3.469446951953613696E-16, 0.000000000000000000, -1.000000000000000000 ) ) ;
#20899 = CARTESIAN_POINT ( 'NONE',  ( 0.5455278134075217666, 3.346456692913386100, 1.259842519685033357 ) ) ;
#20900 = EDGE_CURVE ( 'NONE', #8317, #7323, #39396, .T. ) ;
#20901 = VECTOR ( 'NONE', #38349, 39.37007874015748143 ) ;
#20902 = CARTESIAN_POINT ( 'NONE',  ( -1.453832412804729302, 0.000000000000000000, -1.018633753700964428 ) ) ;
#20903 = ORIENTED_EDGE ( 'NONE', *, *, #34991, .T. ) ;
#20904 = EDGE_LOOP ( 'NONE', ( #15009, #14758, #12528 ) ) ;
#20905 = DIRECTION ( 'NONE',  ( -0.01601477604151182663, 0.9998717552508123996, -0.000000000000000000 ) ) ;
#20906 = FACE_OUTER_BOUND ( 'NONE', #3104, .T. ) ;
#20907 = FACE_BOUND ( 'NONE', #48868, .T. ) ;
#20908 = EDGE_LOOP ( 'NONE', ( #20459, #50945, #111, #35139 ) ) ;
#20909 = CARTESIAN_POINT ( 'NONE',  ( -2.182111253630085734, 3.267716535433071279, -0.6299212598425177889 ) ) ;
#20910 = EDGE_CURVE ( 'NONE', #49043, #26202, #20542, .T. ) ;
#20911 = LINE ( 'NONE', #25296, #6113 ) ;
#20912 = ORIENTED_EDGE ( 'NONE', *, *, #12097, .T. ) ;
#20913 = DIRECTION ( 'NONE',  ( 1.000000000000000000, -0.000000000000000000, 0.000000000000000000 ) ) ;
#20914 = B_SPLINE_CURVE_WITH_KNOTS ( 'NONE', 3,
 ( #10743, #29858, #10236, #41477 ),
 .UNSPECIFIED., .F., .F.,
 ( 4, 4 ),
 ( 1.140376665250896911E-05, 0.05043874644244002864 ),
 .UNSPECIFIED. ) ;
#20915 = FACE_OUTER_BOUND ( 'NONE', #26327, .T. ) ;
#20916 = EDGE_CURVE ( 'NONE', #42699, #4909, #40430, .T. ) ;
#20917 = ORIENTED_EDGE ( 'NONE', *, *, #19119, .T. ) ;
#20918 = ORIENTED_EDGE ( 'NONE', *, *, #50532, .F. ) ;
#20919 = ORIENTED_EDGE ( 'NONE', *, *, #24815, .F. ) ;
#20920 = CARTESIAN_POINT ( 'NONE',  ( 0.5455278134075211005, 3.346456692913386100, 0.1181102362204701633 ) ) ;
#20921 = DIRECTION ( 'NONE',  ( 0.000000000000000000, 1.000000000000000000, 0.000000000000000000 ) ) ;
#20922 = DIRECTION ( 'NONE',  ( 1.000000000000000000, 0.000000000000000000, 0.000000000000000000 ) ) ;
#20923 = LINE ( 'NONE', #535, #50206 ) ;
#20924 = VERTEX_POINT ( 'NONE', #31918 ) ;
#20925 = B_SPLINE_CURVE_WITH_KNOTS ( 'NONE', 3,
 ( #45431, #18096, #1835, #21206 ),
 .UNSPECIFIED., .F., .F.,
 ( 4, 4 ),
 ( 2.103951164766250122E-07, 0.01609579516997627566 ),
 .UNSPECIFIED. ) ;
#20926 = VERTEX_POINT ( 'NONE', #4033 ) ;
#20927 = AXIS2_PLACEMENT_3D ( 'NONE', #49755, #47092, #42992 ) ;
#20928 = CARTESIAN_POINT ( 'NONE',  ( -1.909347346926324462, 0.000000000000000000, -0.1574803149606297248 ) ) ;
#20929 = DIRECTION ( 'NONE',  ( -1.776356839400250149E-14, 0.000000000000000000, 1.000000000000000000 ) ) ;
#20930 = LINE ( 'NONE', #32049, #17548 ) ;
#20931 = CONICAL_SURFACE ( 'NONE', #3604, 1.850107469027523210, 0.6386652850508578450 ) ;
#20932 = EDGE_CURVE ( 'NONE', #6769, #38240, #33558, .T. ) ;
#20933 = DIRECTION ( 'NONE',  ( 0.3930250316539278810, 0.000000000000000000, -0.9195277725514489076 ) ) ;
#20934 = VECTOR ( 'NONE', #24889, 39.37007874015748143 ) ;
#20935 = PLANE ( 'NONE',  #37969 ) ;
#20936 = AXIS2_PLACEMENT_3D ( 'NONE', #7723, #22969, #11846 ) ;
#20937 = DIRECTION ( 'NONE',  ( 0.000000000000000000, 0.000000000000000000, 1.000000000000000000 ) ) ;
#20938 = CARTESIAN_POINT ( 'NONE',  ( 1.929629134066521923, 1.574803149606302854, 0.9824921284572415425 ) ) ;
#20939 = VECTOR ( 'NONE', #36183, 39.37007874015748143 ) ;
#20940 = ORIENTED_EDGE ( 'NONE', *, *, #29651, .F. ) ;
#20941 = CARTESIAN_POINT ( 'NONE',  ( 0.1067246931122726866, 0.02962905676920215767, 0.000000000000000000 ) ) ;
#20942 = CARTESIAN_POINT ( 'NONE',  ( 0.000000000000000000, 3.346456692913386100, 0.000000000000000000 ) ) ;
#20943 = VERTEX_POINT ( 'NONE', #32430 ) ;
#20944 = VERTEX_POINT ( 'NONE', #145 ) ;
#20945 = CARTESIAN_POINT ( 'NONE',  ( 2.479883737258961940, 1.750989359453594130, -0.5155390881854031715 ) ) ;
#20946 = PLANE ( 'NONE',  #610 ) ;
#20947 = VERTEX_POINT ( 'NONE', #12804 ) ;
#20948 = EDGE_LOOP ( 'NONE', ( #10601, #34435, #11288, #41990 ) ) ;
#20949 = CARTESIAN_POINT ( 'NONE',  ( 2.151809081513405886, 1.574803149606302854, 0.2418202932658659043 ) ) ;
#20950 = ORIENTED_EDGE ( 'NONE', *, *, #21722, .T. ) ;
#20951 = ORIENTED_EDGE ( 'NONE', *, *, #441, .T. ) ;
#20952 = EDGE_CURVE ( 'NONE', #16283, #5399, #28534, .T. ) ;
#20953 = CARTESIAN_POINT ( 'NONE',  ( -0.9726748280992547624, 0.004179766354514788743, 1.532033615445409724 ) ) ;
#20954 = CARTESIAN_POINT ( 'NONE',  ( 0.8182917201112817063, 3.346456692913386100, -2.047244094488181343 ) ) ;
#20955 = EDGE_CURVE ( 'NONE', #31614, #18410, #35525, .T. ) ;
#20956 = B_SPLINE_CURVE_WITH_KNOTS ( 'NONE', 3,
 ( #22678, #17787, #45889, #26543 ),
 .UNSPECIFIED., .F., .F.,
 ( 4, 4 ),
 ( 6.477935607884877264E-07, 0.004084871717682403425 ),
 .UNSPECIFIED. ) ;
#20957 = EDGE_CURVE ( 'NONE', #40341, #46985, #34732, .T. ) ;
#20958 = ORIENTED_EDGE ( 'NONE', *, *, #16532, .T. ) ;
#20959 = VERTEX_POINT ( 'NONE', #27505 ) ;
#20960 = VERTEX_POINT ( 'NONE', #17435 ) ;
#20961 = DIRECTION ( 'NONE',  ( 0.000000000000000000, 0.000000000000000000, 1.000000000000000000 ) ) ;
#20962 = CIRCLE ( 'NONE', #28360, 2.106299212598425008 ) ;
#20963 = EDGE_LOOP ( 'NONE', ( #13561, #10356, #50609, #33815 ) ) ;
#20964 = ORIENTED_EDGE ( 'NONE', *, *, #11546, .T. ) ;
#20965 = CONICAL_SURFACE ( 'NONE', #41572, 3.483074324928249421, 1.244861948955335196 ) ;
#20966 = DIRECTION ( 'NONE',  ( -0.000000000000000000, 1.000000000000000000, -0.000000000000000000 ) ) ;
#20967 = DIRECTION ( 'NONE',  ( 1.734723475976806848E-16, 0.000000000000000000, 1.000000000000000000 ) ) ;
#20968 = LINE ( 'NONE', #48545, #475 ) ;
#20969 = CONICAL_SURFACE ( 'NONE', #15185, 2.246510896728926010, 0.01601546068027819014 ) ;
#20970 = AXIS2_PLACEMENT_3D ( 'NONE', #5129, #9007, #17269 ) ;
#20971 = ORIENTED_EDGE ( 'NONE', *, *, #30457, .F. ) ;
#20972 = B_SPLINE_CURVE_WITH_KNOTS ( 'NONE', 3,
 ( #15793, #35171, #12181, #8053 ),
 .UNSPECIFIED., .F., .F.,
 ( 4, 4 ),
 ( 0.01355629821058103486, 0.03074392676604455199 ),
 .UNSPECIFIED. ) ;
#20973 = CARTESIAN_POINT ( 'NONE',  ( -1.909347346926324906, 0.000000000000000000, 1.417322834645662333 ) ) ;
#20974 = DIRECTION ( 'NONE',  ( 0.000000000000000000, 0.000000000000000000, -1.000000000000000000 ) ) ;
#20975 = CARTESIAN_POINT ( 'NONE',  ( 1.698224779224786429, 1.735102128624146811, -1.555582603516539875 ) ) ;
#20976 = VERTEX_POINT ( 'NONE', #13822 ) ;
#20977 = LINE ( 'NONE', #40351, #18309 ) ;
#20978 = FACE_OUTER_BOUND ( 'NONE', #25644, .T. ) ;
#20979 = AXIS2_PLACEMENT_3D ( 'NONE', #2280, #26717, #14857 ) ;
#20980 = FACE_OUTER_BOUND ( 'NONE', #30138, .T. ) ;
#20981 = EDGE_LOOP ( 'NONE', ( #31298, #3855, #30633, #7463 ) ) ;
#20982 = ORIENTED_EDGE ( 'NONE', *, *, #11295, .T. ) ;
#20983 = LINE ( 'NONE', #24087, #22149 ) ;
#20984 = CARTESIAN_POINT ( 'NONE',  ( 0.000000000000000000, 0.000000000000000000, 0.000000000000000000 ) ) ;
#20985 = DIRECTION ( 'NONE',  ( -0.9998717552508121775, -0.01601477604151182663, 0.000000000000000000 ) ) ;
#20986 = ADVANCED_FACE ( 'NONE', ( #5561 ), #5301, .F. ) ;
#20987 = LINE ( 'NONE', #21495, #35195 ) ;
#20988 = CARTESIAN_POINT ( 'NONE',  ( 0.4787700707360283414, 1.205361022782829114E-17, -1.919768535593459724 ) ) ;
#20989 = ORIENTED_EDGE ( 'NONE', *, *, #1841, .T. ) ;
#20990 = ORIENTED_EDGE ( 'NONE', *, *, #39961, .F. ) ;
#20991 = DIRECTION ( 'NONE',  ( -0.01601477604151182663, 0.9998717552508123996, -0.000000000000000000 ) ) ;
#20992 = ORIENTED_EDGE ( 'NONE', *, *, #15710, .F. ) ;
#20993 = FACE_OUTER_BOUND ( 'NONE', #35725, .T. ) ;
#20994 = EDGE_CURVE ( 'NONE', #23689, #17781, #2200, .T. ) ;
#20995 = DIRECTION ( 'NONE',  ( 1.734723475976806848E-16, -0.000000000000000000, 1.000000000000000000 ) ) ;
#20996 = CARTESIAN_POINT ( 'NONE',  ( -1.546652493784001603, 0.000000000000000000, 0.8508756243308288614 ) ) ;
#20997 = FACE_OUTER_BOUND ( 'NONE', #48807, .T. ) ;
#20998 = FACE_OUTER_BOUND ( 'NONE', #45888, .T. ) ;
#20999 = ORIENTED_EDGE ( 'NONE', *, *, #11123, .F. ) ;
#21000 = VECTOR ( 'NONE', #8607, 39.37007874015748143 ) ;
#21001 = DIRECTION ( 'NONE',  ( -3.469446951953613696E-16, 0.000000000000000000, -1.000000000000000000 ) ) ;
#21002 = B_SPLINE_CURVE_WITH_KNOTS ( 'NONE', 3,
 ( #32180, #47870, #29573, #30080 ),
 .UNSPECIFIED., .F., .F.,
 ( 4, 4 ),
 ( 0.1211775127643062860, 0.1625894504277921315 ),
 .UNSPECIFIED. ) ;
#21003 = ADVANCED_FACE ( 'NONE', ( #17186 ), #29818, .F. ) ;
#21004 = VECTOR ( 'NONE', #41579, 39.37007874015748143 ) ;
#21005 = CARTESIAN_POINT ( 'NONE',  ( 1.560669927219590525, 0.000000000000000000, 0.9055118110236164419 ) ) ;
#21006 = VECTOR ( 'NONE', #26032, 39.37007874015748143 ) ;
#21007 = ADVANCED_FACE ( 'NONE', ( #13312 ), #25429, .T. ) ;
#21008 = VECTOR ( 'NONE', #41215, 39.37007874015748143 ) ;
#21009 = ORIENTED_EDGE ( 'NONE', *, *, #2070, .F. ) ;
#21010 = DIRECTION ( 'NONE',  ( 1.734723475976806848E-16, 0.000000000000000000, 1.000000000000000000 ) ) ;
#21011 = FACE_OUTER_BOUND ( 'NONE', #26622, .T. ) ;
#21012 = FACE_OUTER_BOUND ( 'NONE', #20280, .T. ) ;
#21013 = EDGE_LOOP ( 'NONE', ( #1067, #23202, #42375, #31001 ) ) ;
#21014 = CARTESIAN_POINT ( 'NONE',  ( -0.2627480064045953911, 0.000000000000000000, 1.723473835155032274 ) ) ;
#21015 = CARTESIAN_POINT ( 'NONE',  ( 1.833433833923351353, 3.346456692913386100, 0.7480314960629872445 ) ) ;
#21016 = VECTOR ( 'NONE', #9467, 39.37007874015748143 ) ;
#21017 = EDGE_LOOP ( 'NONE', ( #31310, #36921, #22510, #11437 ) ) ;
#21018 = DIRECTION ( 'NONE',  ( -3.469446951953613696E-16, 0.000000000000000000, -1.000000000000000000 ) ) ;
#21019 = PLANE ( 'NONE',  #50464 ) ;
#21020 = ORIENTED_EDGE ( 'NONE', *, *, #40902, .F. ) ;
#21021 = CARTESIAN_POINT ( 'NONE',  ( -0.2727639067037610499, 0.000000000000000000, -2.047244094488181343 ) ) ;
#21022 = ADVANCED_FACE ( 'NONE', ( #44781 ), #9946, .F. ) ;
#21023 = DIRECTION ( 'NONE',  ( -0.5128992774059071280, -9.962263361493005127E-17, 0.8584487936018655452 ) ) ;
#21024 = DIRECTION ( 'NONE',  ( -0.000000000000000000, 1.000000000000000000, -0.000000000000000000 ) ) ;
#21025 = CARTESIAN_POINT ( 'NONE',  ( -1.091055626815042201, 3.346456692913386100, 1.062992125984246083 ) ) ;
#21026 = EDGE_CURVE ( 'NONE', #10852, #11355, #21564, .T. ) ;
#21027 = EDGE_CURVE ( 'NONE', #11581, #39976, #40142, .T. ) ;
#21028 = CARTESIAN_POINT ( 'NONE',  ( 0.2727639067037604392, 0.000000000000000000, -1.299212598425193210 ) ) ;
#21029 = VERTEX_POINT ( 'NONE', #1173 ) ;
#21030 = ORIENTED_EDGE ( 'NONE', *, *, #48936, .F. ) ;
#21031 = CARTESIAN_POINT ( 'NONE',  ( -2.454875160333845674, 0.000000000000000000, -0.3543307086614173040 ) ) ;
#21032 = EDGE_CURVE ( 'NONE', #14557, #6504, #19482, .T. ) ;
#21033 = FACE_OUTER_BOUND ( 'NONE', #26572, .T. ) ;
#21034 = EDGE_LOOP ( 'NONE', ( #898, #27995, #33935, #42621 ) ) ;
#21035 = DIRECTION ( 'NONE',  ( -0.01601477604151182663, 0.9998717552508123996, -0.000000000000000000 ) ) ;
#21036 = CARTESIAN_POINT ( 'NONE',  ( 1.015142113812069313, 0.000000000000000000, 0.2755905511810994302 ) ) ;
#21037 = LINE ( 'NONE', #36786, #10444 ) ;
#21038 = CARTESIAN_POINT ( 'NONE',  ( 0.000000000000000000, 3.346456692913386100, 0.000000000000000000 ) ) ;
#21039 = ORIENTED_EDGE ( 'NONE', *, *, #28941, .T. ) ;
#21040 = ORIENTED_EDGE ( 'NONE', *, *, #24202, .T. ) ;
#21041 = LINE ( 'NONE', #16405, #27873 ) ;
#21042 = CARTESIAN_POINT ( 'NONE',  ( 0.5110944797606088441, 1.727220439156562204, 2.908232962414051492 ) ) ;
#21043 = CARTESIAN_POINT ( 'NONE',  ( -2.443991082961025185, 3.256070107886888554, 0.1574803149606286423 ) ) ;
#21044 = ORIENTED_EDGE ( 'NONE', *, *, #30060, .F. ) ;
#21045 = DIRECTION ( 'NONE',  ( -3.469446951953613696E-16, 0.000000000000000000, -1.000000000000000000 ) ) ;
#21046 = FACE_BOUND ( 'NONE', #19591, .T. ) ;
#21047 = VECTOR ( 'NONE', #43893, 39.37007874015748143 ) ;
#21048 = ORIENTED_EDGE ( 'NONE', *, *, #32115, .T. ) ;
#21049 = AXIS2_PLACEMENT_3D ( 'NONE', #13169, #20905, #25033 ) ;
#21050 = DIRECTION ( 'NONE',  ( 0.000000000000000000, 0.000000000000000000, 1.000000000000000000 ) ) ;
#21051 = VECTOR ( 'NONE', #45167, 39.37007874015748143 ) ;
#21052 = EDGE_LOOP ( 'NONE', ( #12263, #46516, #27671, #33673 ) ) ;
#21053 = ORIENTED_EDGE ( 'NONE', *, *, #49366, .T. ) ;
#21054 = CARTESIAN_POINT ( 'NONE',  ( -0.2042174104418111591, 0.000000000000000000, -0.3133417129078099328 ) ) ;
#21055 = VECTOR ( 'NONE', #17153, 39.37007874015748143 ) ;
#21057 = ORIENTED_EDGE ( 'NONE', *, *, #38469, .F. ) ;
#21056 = EDGE_CURVE ( 'NONE', #25743, #25170, #47025, .T. ) ;
#21058 = CARTESIAN_POINT ( 'NONE',  ( 0.000000000000000000, 3.267716535433071279, 0.000000000000000000 ) ) ;
#21059 = EDGE_LOOP ( 'NONE', ( #10783, #4667, #21780, #7204 ) ) ;
#21060 = DIRECTION ( 'NONE',  ( 1.000000000000000000, 0.000000000000000000, 0.000000000000000000 ) ) ;
#21061 = LINE ( 'NONE', #36813, #541 ) ;
#21062 = EDGE_CURVE ( 'NONE', #31055, #22725, #37325, .T. ) ;
#21063 = CARTESIAN_POINT ( 'NONE',  ( -0.2727639067037602172, 0.000000000000000000, 1.417322834645662777 ) ) ;
#21064 = EDGE_CURVE ( 'NONE', #25081, #41000, #17877, .T. ) ;
#21065 = EDGE_CURVE ( 'NONE', #23763, #29175, #48878, .T. ) ;
#21066 = DIRECTION ( 'NONE',  ( 1.000000000000000000, 0.000000000000000000, 0.000000000000000000 ) ) ;
#21067 = LINE ( 'NONE', #29578, #15433 ) ;
#21068 = CARTESIAN_POINT ( 'NONE',  ( -0.07591351300297288773, 3.267716535433071279, 2.633779063002553116E-17 ) ) ;
#21069 = VERTEX_POINT ( 'NONE', #17689 ) ;
#21070 = CARTESIAN_POINT ( 'NONE',  ( 2.695799277629594037, 1.453624836071520265, -1.205759334241453651 ) ) ;
#21071 = LINE ( 'NONE', #36825, #8356 ) ;
#21072 = VERTEX_POINT ( 'NONE', #22077 ) ;
#21073 = CARTESIAN_POINT ( 'NONE',  ( -0.8182917201112819283, 0.000000000000000000, -0.4724409448818886470 ) ) ;
#21074 = CARTESIAN_POINT ( 'NONE',  ( 1.950008968278537091, 6.692913385826772199, 0.9934589848971188131 ) ) ;
#21075 = ORIENTED_EDGE ( 'NONE', *, *, #13256, .T. ) ;
#21076 = DIRECTION ( 'NONE',  ( -0.3090169943749582204, 0.000000000000000000, 0.9510565162951500895 ) ) ;
#21077 = CARTESIAN_POINT ( 'NONE',  ( 1.363819533518803251, 3.267716535433071279, -2.365849761790805487E-16 ) ) ;
#21078 = CARTESIAN_POINT ( 'NONE',  ( 1.560669927219591191, 3.346456692913386100, 1.535433070866133898 ) ) ;
#21079 = VECTOR ( 'NONE', #12552, 39.37007874015748143 ) ;
#21080 = AXIS2_PLACEMENT_3D ( 'NONE', #10324, #13435, #29434 ) ;
#21081 = VERTEX_POINT ( 'NONE', #33457 ) ;
#21082 = CARTESIAN_POINT ( 'NONE',  ( -2.258024766633058622, 0.000000000000000000, 0.1574803149606286423 ) ) ;
#21083 = EDGE_CURVE ( 'NONE', #37126, #22293, #49142, .T. ) ;
#21084 = ORIENTED_EDGE ( 'NONE', *, *, #45981, .T. ) ;
#21085 = FACE_BOUND ( 'NONE', #33578, .T. ) ;
#21086 = VECTOR ( 'NONE', #17594, 39.37007874015748143 ) ;
#21087 = DIRECTION ( 'NONE',  ( -1.000000000000000000, 0.000000000000000000, 1.734723475976806848E-16 ) ) ;
#21088 = EDGE_CURVE ( 'NONE', #36015, #41720, #13155, .T. ) ;
#21089 = CARTESIAN_POINT ( 'NONE',  ( -1.636583440222563635, 3.267716535433071279, 1.062992125984246083 ) ) ;
#21090 = DIRECTION ( 'NONE',  ( 0.000000000000000000, 0.000000000000000000, -1.000000000000000000 ) ) ;
#21091 = CIRCLE ( 'NONE', #49893, 1.743387098533651480 ) ;
#21092 = EDGE_CURVE ( 'NONE', #48759, #15500, #29140, .T. ) ;
#21093 = EDGE_CURVE ( 'NONE', #7484, #10001, #49395, .T. ) ;
#21094 = VECTOR ( 'NONE', #41914, 39.37007874015748143 ) ;
#21095 = ORIENTED_EDGE ( 'NONE', *, *, #21056, .T. ) ;
#21096 = ORIENTED_EDGE ( 'NONE', *, *, #48301, .F. ) ;
#21097 = CARTESIAN_POINT ( 'NONE',  ( -0.8182917201112814842, 3.267716535433071279, 1.732283464566921172 ) ) ;
#21098 = ADVANCED_FACE ( 'NONE', ( #30579 ), #38830, .F. ) ;
#21099 = ORIENTED_EDGE ( 'NONE', *, *, #36428, .F. ) ;
#21100 = DIRECTION ( 'NONE',  ( -0.9972836025229415702, 0.000000000000000000, -0.07365742419378766559 ) ) ;
#21101 = ORIENTED_EDGE ( 'NONE', *, *, #48750, .F. ) ;
#21102 = LINE ( 'NONE', #16978, #9141 ) ;
#21103 = ORIENTED_EDGE ( 'NONE', *, *, #20910, .F. ) ;
#21104 = DIRECTION ( 'NONE',  ( -3.469446951953613696E-16, 0.000000000000000000, -1.000000000000000000 ) ) ;
#21105 = B_SPLINE_CURVE_WITH_KNOTS ( 'NONE', 3,
 ( #3844, #50021, #30459, #18831 ),
 .UNSPECIFIED., .F., .F.,
 ( 4, 4 ),
 ( 0.1211873102087489551, 0.1625992483279400380 ),
 .UNSPECIFIED. ) ;
#21106 = CARTESIAN_POINT ( 'NONE',  ( 0.000000000000000000, 3.267716535433071279, -1.929133858267710000 ) ) ;
#21107 = EDGE_LOOP ( 'NONE', ( #7760, #9295, #34785, #2428 ) ) ;
#21108 = LINE ( 'NONE', #36346, #39725 ) ;
#21109 = VERTEX_POINT ( 'NONE', #22574 ) ;
#21110 = ORIENTED_EDGE ( 'NONE', *, *, #33318, .T. ) ;
#21111 = AXIS2_PLACEMENT_3D ( 'NONE', #35473, #47557, #23848 ) ;
#21112 = VERTEX_POINT ( 'NONE', #14583 ) ;
#21113 = ORIENTED_EDGE ( 'NONE', *, *, #16467, .T. ) ;
#21114 = DIRECTION ( 'NONE',  ( -0.9998717552508121775, -0.01601477604151182663, 0.000000000000000000 ) ) ;
#21115 = PLANE ( 'NONE',  #4966 ) ;
#21116 = AXIS2_PLACEMENT_3D ( 'NONE', #13121, #35588, #473 ) ;
#21117 = VERTEX_POINT ( 'NONE', #18709 ) ;
#21118 = LINE ( 'NONE', #28854, #27880 ) ;
#21119 = AXIS2_PLACEMENT_3D ( 'NONE', #11252, #42734, #34499 ) ;
#21120 = VERTEX_POINT ( 'NONE', #38335 ) ;
#21121 = CARTESIAN_POINT ( 'NONE',  ( 0.000000000000000000, 0.4724409448818898127, 0.000000000000000000 ) ) ;
#21122 = EDGE_CURVE ( 'NONE', #31774, #16641, #32266, .T. ) ;
#21123 = CIRCLE ( 'NONE', #14524, 2.165354330708661568 ) ;
#21124 = LINE ( 'NONE', #36875, #9913 ) ;
#21125 = ORIENTED_EDGE ( 'NONE', *, *, #16636, .F. ) ;
#21126 = EDGE_CURVE ( 'NONE', #3114, #2304, #19197, .T. ) ;
#21127 = VECTOR ( 'NONE', #5852, 39.37007874015748143 ) ;
#21128 = CARTESIAN_POINT ( 'NONE',  ( -0.3500732549360408563, 1.603869690133923331, 2.204675616574417685 ) ) ;
#21129 = CARTESIAN_POINT ( 'NONE',  ( -0.6214413264104945434, 3.346456692913386100, -2.074263738136479240 ) ) ;
#21130 = ORIENTED_EDGE ( 'NONE', *, *, #23584, .F. ) ;
#21131 = LINE ( 'NONE', #35405, #46367 ) ;
#21132 = DIRECTION ( 'NONE',  ( -0.9998717552508122886, -0.01601477604151185785, 0.000000000000000000 ) ) ;
#21133 = LINE ( 'NONE', #9253, #26010 ) ;
#21134 = CARTESIAN_POINT ( 'NONE',  ( 0.000000000000000000, 3.346456692913386100, 0.000000000000000000 ) ) ;
#21135 = CARTESIAN_POINT ( 'NONE',  ( -1.427293369312925497, 0.000000000000000000, -1.001115484471666761 ) ) ;
#21136 = ORIENTED_EDGE ( 'NONE', *, *, #5343, .F. ) ;
#21137 = CARTESIAN_POINT ( 'NONE',  ( -0.8338860769296044806, 1.049866565877818125, -1.845005749107295756 ) ) ;
#21138 = DIRECTION ( 'NONE',  ( 0.000000000000000000, -1.000000000000000000, 0.000000000000000000 ) ) ;
#21139 = ORIENTED_EDGE ( 'NONE', *, *, #34847, .F. ) ;
#21140 = CARTESIAN_POINT ( 'NONE',  ( -1.536664496436148184E-16, 3.267716535433071279, 0.1181102362204701633 ) ) ;
#21141 = EDGE_CURVE ( 'NONE', #14945, #767, #37860, .T. ) ;
#21142 = ORIENTED_EDGE ( 'NONE', *, *, #39435, .F. ) ;
#21143 = DIRECTION ( 'NONE',  ( 1.000000000000000000, 0.000000000000000000, 0.000000000000000000 ) ) ;
#21144 = CARTESIAN_POINT ( 'NONE',  ( 2.161044708975088380, 1.205361022782829114E-17, 0.1463148319730657732 ) ) ;
#21145 = CARTESIAN_POINT ( 'NONE',  ( 1.091055626815043311, 3.267716535433071279, 1.889763779527550369 ) ) ;
#21146 = EDGE_CURVE ( 'NONE', #11424, #1319, #49643, .T. ) ;
#21147 = CARTESIAN_POINT ( 'NONE',  ( 0.000000000000000000, 3.267716535433071279, 0.000000000000000000 ) ) ;
#21148 = DIRECTION ( 'NONE',  ( 1.000000000000000000, -0.000000000000000000, 0.000000000000000000 ) ) ;
#21149 = EDGE_LOOP ( 'NONE', ( #41159, #1157, #1167, #33746 ) ) ;
#21150 = AXIS2_PLACEMENT_3D ( 'NONE', #10656, #6775, #38029 ) ;
#21151 = ADVANCED_FACE ( 'NONE', ( #26944 ), #34958, .F. ) ;
#21152 = CARTESIAN_POINT ( 'NONE',  ( 1.695772546416037363, 1.647224322255602891, -2.417756147381349141 ) ) ;
#21153 = VECTOR ( 'NONE', #3097, 39.37007874015748143 ) ;
#21154 = CARTESIAN_POINT ( 'NONE',  ( 1.015142113812069313, 3.346456692913386100, -0.9842519685039348154 ) ) ;
#21155 = VECTOR ( 'NONE', #47039, 39.37007874015748143 ) ;
#21156 = EDGE_CURVE ( 'NONE', #47474, #20582, #14322, .T. ) ;
#21157 = ORIENTED_EDGE ( 'NONE', *, *, #39764, .T. ) ;
#21158 = CARTESIAN_POINT ( 'NONE',  ( -1.497019770989685084, 1.049866565067838486, -1.363210918355331591 ) ) ;
#21159 = VECTOR ( 'NONE', #48289, 39.37007874015748143 ) ;
#21160 = ORIENTED_EDGE ( 'NONE', *, *, #17354, .F. ) ;
#21161 = CARTESIAN_POINT ( 'NONE',  ( 1.852263788401641076, 0.9949518933081566985, -1.839032047933712111 ) ) ;
#21162 = CARTESIAN_POINT ( 'NONE',  ( 0.8291286199751974895, 1.205361022782829114E-17, -1.835126787948130556 ) ) ;
#21163 = VECTOR ( 'NONE', #34458, 39.37007874015748143 ) ;
#21164 = CARTESIAN_POINT ( 'NONE',  ( -1.883550378546958060, 1.205361022782829114E-17, -1.069467267250448161 ) ) ;
#21165 = AXIS2_PLACEMENT_3D ( 'NONE', #25924, #26425, #14560 ) ;
#21166 = DIRECTION ( 'NONE',  ( -0.9998717552508122886, -0.01601477604151182316, 0.000000000000000000 ) ) ;
#21167 = ORIENTED_EDGE ( 'NONE', *, *, #49747, .F. ) ;
#21168 = ORIENTED_EDGE ( 'NONE', *, *, #50847, .T. ) ;
#21169 = FACE_OUTER_BOUND ( 'NONE', #16800, .T. ) ;
#21170 = DIRECTION ( 'NONE',  ( -3.469446951953613696E-16, 0.000000000000000000, -1.000000000000000000 ) ) ;
#21171 = FACE_BOUND ( 'NONE', #4330, .T. ) ;
#21172 = VERTEX_POINT ( 'NONE', #15084 ) ;
#21173 = CARTESIAN_POINT ( 'NONE',  ( 0.8182917201112819283, 3.267716535433071279, -1.419509857074483292E-16 ) ) ;
#21174 = DIRECTION ( 'NONE',  ( 1.000000000000000000, -0.000000000000000000, 0.000000000000000000 ) ) ;
#21175 = EDGE_LOOP ( 'NONE', ( #44062, #15384, #30194, #37469 ) ) ;
#21176 = DIRECTION ( 'NONE',  ( 1.000000000000000000, -0.000000000000000000, 0.000000000000000000 ) ) ;
#21177 = CARTESIAN_POINT ( 'NONE',  ( -2.168245791271168788, 1.205361022782829114E-17, -2.004968704497279486 ) ) ;
#21178 = EDGE_LOOP ( 'NONE', ( #33633, #34285, #39060, #1414 ) ) ;
#21179 = ORIENTED_EDGE ( 'NONE', *, *, #21542, .F. ) ;
#21180 = EDGE_LOOP ( 'NONE', ( #13847, #34323, #3549, #7802 ) ) ;
#21181 = CARTESIAN_POINT ( 'NONE',  ( -1.363819533518803251, 3.267716535433071279, 2.365849761790805487E-16 ) ) ;
#21182 = CARTESIAN_POINT ( 'NONE',  ( 0.2239970000120027616, 0.000000000000000000, -1.939803615689571048 ) ) ;
#21184 = LINE ( 'NONE', #16545, #2801 ) ;
#21183 = AXIS2_PLACEMENT_3D ( 'NONE', #423, #47631, #40450 ) ;
#21185 = DIRECTION ( 'NONE',  ( -1.000000000000000000, 0.000000000000000000, 0.000000000000000000 ) ) ;
#21186 = ORIENTED_EDGE ( 'NONE', *, *, #15816, .T. ) ;
#21187 = VERTEX_POINT ( 'NONE', #10453 ) ;
#21188 = EDGE_CURVE ( 'NONE', #17122, #11634, #40959, .T. ) ;
#21190 = VECTOR ( 'NONE', #9502, 39.37007874015748143 ) ;
#21189 = CARTESIAN_POINT ( 'NONE',  ( -2.576863348864732117, 1.568913320674888201, 1.442554885838411849 ) ) ;
#21191 = PLANE ( 'NONE',  #22991 ) ;
#21192 = EDGE_CURVE ( 'NONE', #3813, #29782, #15334, .T. ) ;
#21193 = CARTESIAN_POINT ( 'NONE',  ( -1.536664496436148184E-16, 3.346456692913386100, -0.5118110236220465570 ) ) ;
#21194 = DIRECTION ( 'NONE',  ( -0.000000000000000000, 1.000000000000000000, -0.000000000000000000 ) ) ;
#21195 = EDGE_CURVE ( 'NONE', #40833, #50445, #7342, .T. ) ;
#21196 = CARTESIAN_POINT ( 'NONE',  ( -1.985260859929297572, 3.267716535433071279, -0.3149606299212589500 ) ) ;
#21197 = LINE ( 'NONE', #6470, #25130 ) ;
#21198 = VECTOR ( 'NONE', #18133, 39.37007874015748143 ) ;
#21199 = CARTESIAN_POINT ( 'NONE',  ( -1.909347346926324462, 0.000000000000000000, -0.3543307086614171930 ) ) ;
#21200 = EDGE_LOOP ( 'NONE', ( #41262, #48539, #16115, #43381 ) ) ;
#21201 = FACE_OUTER_BOUND ( 'NONE', #569, .T. ) ;
#21202 = DIRECTION ( 'NONE',  ( -0.000000000000000000, -1.000000000000000000, -0.000000000000000000 ) ) ;
#21203 = ORIENTED_EDGE ( 'NONE', *, *, #21983, .T. ) ;
#21204 = ORIENTED_EDGE ( 'NONE', *, *, #32437, .F. ) ;
#21205 = LINE ( 'NONE', #40321, #29041 ) ;
#21206 = CARTESIAN_POINT ( 'NONE',  ( 2.190654571063535005, 1.742989292944022939, 0.7635320059819211691 ) ) ;
#21207 = ADVANCED_FACE ( 'NONE', ( #11212 ), #38485, .T. ) ;
#21208 = VERTEX_POINT ( 'NONE', #30073 ) ;
#21209 = EDGE_CURVE ( 'NONE', #35032, #25253, #50146, .T. ) ;
#21210 = ORIENTED_EDGE ( 'NONE', *, *, #22723, .T. ) ;
#21211 = DIRECTION ( 'NONE',  ( 1.000000000000000000, 0.000000000000000000, -3.469446951953613696E-16 ) ) ;
#21212 = ORIENTED_EDGE ( 'NONE', *, *, #35696, .T. ) ;
#21213 = B_SPLINE_CURVE_WITH_KNOTS ( 'NONE', 3,
 ( #41199, #37329, #29571, #48633 ),
 .UNSPECIFIED., .F., .F.,
 ( 4, 4 ),
 ( 2.136716580819921136E-07, 0.01722135198962225847 ),
 .UNSPECIFIED. ) ;
#21214 = FACE_OUTER_BOUND ( 'NONE', #12160, .T. ) ;
#21215 = DIRECTION ( 'NONE',  ( -0.000000000000000000, 1.000000000000000000, -0.000000000000000000 ) ) ;
#21216 = VECTOR ( 'NONE', #28875, 39.37007874015748143 ) ;
#21217 = VECTOR ( 'NONE', #14598, 39.37007874015748143 ) ;
#21218 = VERTEX_POINT ( 'NONE', #6831 ) ;
#21219 = EDGE_LOOP ( 'NONE', ( #12409, #43612, #51040, #11638 ) ) ;
#21220 = ORIENTED_EDGE ( 'NONE', *, *, #5243, .F. ) ;
#21221 = VECTOR ( 'NONE', #38840, 39.37007874015748143 ) ;
#21222 = CARTESIAN_POINT ( 'NONE',  ( -2.295861763883067841, 1.675315707476183080, 0.7977158951143258347 ) ) ;
#21223 = EDGE_LOOP ( 'NONE', ( #30329, #17556, #31566, #44019 ) ) ;
#21224 = ORIENTED_EDGE ( 'NONE', *, *, #21500, .T. ) ;
#21225 = DIRECTION ( 'NONE',  ( -3.469446951953613696E-16, 0.000000000000000000, -1.000000000000000000 ) ) ;
#21226 = DIRECTION ( 'NONE',  ( -1.000000000000000000, 0.000000000000000000, 1.734723475976806848E-16 ) ) ;
#21227 = CARTESIAN_POINT ( 'NONE',  ( 2.277873973731426194, 1.656288013650806912, 1.879489153247668076 ) ) ;
#21228 = EDGE_CURVE ( 'NONE', #22686, #15190, #6387, .T. ) ;
#21229 = ORIENTED_EDGE ( 'NONE', *, *, #12198, .T. ) ;
#21230 = CARTESIAN_POINT ( 'NONE',  ( 1.560669927219590747, 0.000000000000000000, -0.4724409448818889246 ) ) ;
#21231 = CARTESIAN_POINT ( 'NONE',  ( -0.2727639067037608278, 0.000000000000000000, -1.614173228346451605 ) ) ;
#21232 = CARTESIAN_POINT ( 'NONE',  ( 0.000000000000000000, 3.267716535433071279, 0.7480314960629872445 ) ) ;
#21233 = ORIENTED_EDGE ( 'NONE', *, *, #44421, .T. ) ;
#21234 = DIRECTION ( 'NONE',  ( -1.000000000000000000, 0.000000000000000000, 1.734723475976806848E-16 ) ) ;
#21235 = CARTESIAN_POINT ( 'NONE',  ( -0.04921259842519708910, 1.674305324545202867, 2.241718228789840950 ) ) ;
#21236 = DIRECTION ( 'NONE',  ( 0.000000000000000000, -1.000000000000000000, 0.000000000000000000 ) ) ;
#21237 = ORIENTED_EDGE ( 'NONE', *, *, #35425, .T. ) ;
#21238 = ORIENTED_EDGE ( 'NONE', *, *, #46539, .T. ) ;
#21239 = VECTOR ( 'NONE', #48069, 39.37007874015748143 ) ;
#21240 = CARTESIAN_POINT ( 'NONE',  ( 0.000000000000000000, 3.267716535433071279, 1.220472440944875281 ) ) ;
#21241 = CARTESIAN_POINT ( 'NONE',  ( 0.7423782071083091516, 3.346456692913386100, 2.034117492951036166 ) ) ;
#21242 = DIRECTION ( 'NONE',  ( 0.000000000000000000, 0.000000000000000000, -1.000000000000000000 ) ) ;
#21243 = ORIENTED_EDGE ( 'NONE', *, *, #47470, .F. ) ;
#21244 = EDGE_LOOP ( 'NONE', ( #23552, #28701, #40132, #27312 ) ) ;
#21245 = EDGE_CURVE ( 'NONE', #48594, #23441, #6587, .T. ) ;
#21246 = DIRECTION ( 'NONE',  ( 0.000000000000000000, -1.000000000000000000, 0.000000000000000000 ) ) ;
#21247 = ORIENTED_EDGE ( 'NONE', *, *, #26546, .T. ) ;
#21248 = DIRECTION ( 'NONE',  ( -3.469446951953613696E-16, 0.000000000000000000, -1.000000000000000000 ) ) ;
#21249 = CARTESIAN_POINT ( 'NONE',  ( 2.182111253630085290, 3.346456692913386100, -1.161035397307311917E-15 ) ) ;
#21250 = EDGE_CURVE ( 'NONE', #41945, #13922, #26442, .T. ) ;
#21251 = EDGE_CURVE ( 'NONE', #39570, #10700, #341, .T. ) ;
#21252 = VECTOR ( 'NONE', #9912, 39.37007874015748143 ) ;
#21253 = VECTOR ( 'NONE', #43341, 39.37007874015748143 ) ;
#21254 = ADVANCED_FACE ( 'NONE', ( #23577 ), #3062, .T. ) ;
#21255 = CARTESIAN_POINT ( 'NONE',  ( 1.287906020515829919, 3.346456692913386100, -1.740706023381844547 ) ) ;
#21256 = CARTESIAN_POINT ( 'NONE',  ( 1.287906020515830141, 3.267716535433071279, -0.1968503937007883287 ) ) ;
#21257 = DIRECTION ( 'NONE',  ( 1.000000000000000000, 0.000000000000000000, 0.000000000000000000 ) ) ;
#21258 = ORIENTED_EDGE ( 'NONE', *, *, #8526, .F. ) ;
#21259 = DIRECTION ( 'NONE',  ( -0.9998717552508122886, -0.01601477604151182316, 0.000000000000000000 ) ) ;
#21260 = AXIS2_PLACEMENT_3D ( 'NONE', #9036, #24273, #780 ) ;
#21261 = CARTESIAN_POINT ( 'NONE',  ( -0.07591351300297340121, 3.346456692913386100, -1.299212598425193210 ) ) ;
#21262 = VERTEX_POINT ( 'NONE', #4214 ) ;
#21263 = CARTESIAN_POINT ( 'NONE',  ( 1.833433833923351353, 0.000000000000000000, 1.259842519685033135 ) ) ;
#21264 = DIRECTION ( 'NONE',  ( 0.9998717552508121775, 0.01601477604151182663, 0.000000000000000000 ) ) ;
#21265 = EDGE_CURVE ( 'NONE', #32836, #24066, #19947, .T. ) ;
#21266 = CARTESIAN_POINT ( 'NONE',  ( 0.000000000000000000, 3.267716535433071279, 0.3149606299212578953 ) ) ;
#21267 = ORIENTED_EDGE ( 'NONE', *, *, #33374, .T. ) ;
#21268 = FACE_OUTER_BOUND ( 'NONE', #16715, .T. ) ;
#21269 = VECTOR ( 'NONE', #5562, 39.37007874015748143 ) ;
#21270 = CARTESIAN_POINT ( 'NONE',  ( 2.136190583516914820, 1.205361022782829114E-17, -0.1451986319116555235 ) ) ;
#21271 = EDGE_CURVE ( 'NONE', #22242, #40968, #19701, .T. ) ;
#21272 = ORIENTED_EDGE ( 'NONE', *, *, #49451, .T. ) ;
#21273 = LINE ( 'NONE', #1645, #49382 ) ;
#21274 = CARTESIAN_POINT ( 'NONE',  ( 0.000000000000000000, 2.755905511811022723, 0.000000000000000000 ) ) ;
#21275 = VERTEX_POINT ( 'NONE', #35463 ) ;
#21276 = CIRCLE ( 'NONE', #29531, 1.743387098533651480 ) ;
#21277 = B_SPLINE_CURVE_WITH_KNOTS ( 'NONE', 3,
 ( #20557, #40186, #44299, #32190 ),
 .UNSPECIFIED., .F., .F.,
 ( 4, 4 ),
 ( 0.1211775127643062444, 0.1625894504277921315 ),
 .UNSPECIFIED. ) ;
#21278 = CARTESIAN_POINT ( 'NONE',  ( 0.000000000000000000, 3.267716535433071279, -0.8267716535433052849 ) ) ;
#21279 = CARTESIAN_POINT ( 'NONE',  ( -2.182111253630085734, 0.000000000000000000, -0.9448818897637762948 ) ) ;
#21280 = DIRECTION ( 'NONE',  ( 0.000000000000000000, -0.000000000000000000, 1.000000000000000000 ) ) ;
#21281 = CARTESIAN_POINT ( 'NONE',  ( -1.439733046521777027, 3.346456692913386100, -1.771653543307080581 ) ) ;
#21282 = EDGE_CURVE ( 'NONE', #23253, #29154, #8599, .T. ) ;
#21283 = CARTESIAN_POINT ( 'NONE',  ( 0.000000000000000000, 6.692913385826772199, 0.000000000000000000 ) ) ;
#21284 = ORIENTED_EDGE ( 'NONE', *, *, #27108, .T. ) ;
#21285 = VERTEX_POINT ( 'NONE', #15829 ) ;
#21286 = DIRECTION ( 'NONE',  ( -3.469446951953613696E-16, 0.000000000000000000, -1.000000000000000000 ) ) ;
#21287 = FACE_OUTER_BOUND ( 'NONE', #20053, .T. ) ;
#21288 = ORIENTED_EDGE ( 'NONE', *, *, #19181, .T. ) ;
#21289 = FACE_OUTER_BOUND ( 'NONE', #22410, .T. ) ;
#21290 = CARTESIAN_POINT ( 'NONE',  ( 0.000000000000000000, 0.000000000000000000, 0.000000000000000000 ) ) ;
#21291 = FACE_OUTER_BOUND ( 'NONE', #12785, .T. ) ;
#21292 = EDGE_CURVE ( 'NONE', #17810, #18573, #31591, .T. ) ;
#21293 = DIRECTION ( 'NONE',  ( 0.5877852522924685852, 0.000000000000000000, 0.8090169943749507819 ) ) ;
#21294 = ORIENTED_EDGE ( 'NONE', *, *, #39827, .F. ) ;
#21295 = EDGE_LOOP ( 'NONE', ( #44518, #23902, #49508, #22050 ) ) ;
#21296 = CARTESIAN_POINT ( 'NONE',  ( 0.8182917201112824834, 3.346456692913386100, 2.047244094488179567 ) ) ;
#21297 = DIRECTION ( 'NONE',  ( 0.000000000000000000, 0.000000000000000000, -1.000000000000000000 ) ) ;
#21298 = VECTOR ( 'NONE', #31183, 39.37007874015748143 ) ;
#21299 = LINE ( 'NONE', #49128, #32171 ) ;
#21300 = ORIENTED_EDGE ( 'NONE', *, *, #45464, .F. ) ;
#21301 = LINE ( 'NONE', #33187, #44638 ) ;
#21302 = FACE_BOUND ( 'NONE', #34294, .T. ) ;
#21303 = VERTEX_POINT ( 'NONE', #16091 ) ;
#21304 = EDGE_CURVE ( 'NONE', #26089, #1230, #35910, .T. ) ;
#21305 = CARTESIAN_POINT ( 'NONE',  ( -2.122494303567052487, 1.641097921313502184, -0.4339672821292706595 ) ) ;
#21306 = ORIENTED_EDGE ( 'NONE', *, *, #9329, .T. ) ;
#21308 = ORIENTED_EDGE ( 'NONE', *, *, #13409, .T. ) ;
#21307 = VECTOR ( 'NONE', #338, 39.37007874015748143 ) ;
#21309 = CARTESIAN_POINT ( 'NONE',  ( -1.263630850544466666, 0.000000000000000000, -1.276241334172347530 ) ) ;
#21310 = EDGE_CURVE ( 'NONE', #1426, #34848, #27210, .T. ) ;
#21311 = AXIS2_PLACEMENT_3D ( 'NONE', #25843, #39489, #31752 ) ;
#21312 = ORIENTED_EDGE ( 'NONE', *, *, #33444, .T. ) ;
#21313 = CARTESIAN_POINT ( 'NONE',  ( -0.8182917201112819283, 0.000000000000000000, -1.732283464566922726 ) ) ;
#21315 = LINE ( 'NONE', #31974, #2329 ) ;
#21314 = VECTOR ( 'NONE', #33008, 39.37007874015748143 ) ;
#21316 = ORIENTED_EDGE ( 'NONE', *, *, #5616, .F. ) ;
#21318 =( CONVERSION_BASED_UNIT ( 'INCH', #44785 ) LENGTH_UNIT ( ) NAMED_UNIT ( #48537 ) );
#21317 = VECTOR ( 'NONE', #42773, 39.37007874015748143 ) ;
#21319 = DIRECTION ( 'NONE',  ( -3.469446951953613696E-16, 0.000000000000000000, -1.000000000000000000 ) ) ;
#21320 = CARTESIAN_POINT ( 'NONE',  ( -1.312442655063644770, 0.006898494447474761912, -1.186737126055851022 ) ) ;
#21321 = EDGE_CURVE ( 'NONE', #42907, #26436, #24211, .T. ) ;
#21322 = B_SPLINE_CURVE_WITH_KNOTS ( 'NONE', 3,
 ( #35029, #6893, #50452, #18520 ),
 .UNSPECIFIED., .F., .F.,
 ( 4, 4 ),
 ( 3.722988146457368422E-07, 0.04368291484730600638 ),
 .UNSPECIFIED. ) ;
#21323 = CARTESIAN_POINT ( 'NONE',  ( 2.225020958752729872, 1.645114536686943296, 0.6712079458291126954 ) ) ;
#21324 = EDGE_CURVE ( 'NONE', #47130, #10670, #12220, .T. ) ;
#21325 = DIRECTION ( 'NONE',  ( -1.000000000000000000, -0.000000000000000000, -0.000000000000000000 ) ) ;
#21326 = CARTESIAN_POINT ( 'NONE',  ( -1.312623452344869435, 5.905511811023623991, 1.722945714930905536 ) ) ;
#21327 = ORIENTED_EDGE ( 'NONE', *, *, #14249, .F. ) ;
#21328 = FACE_OUTER_BOUND ( 'NONE', #16057, .T. ) ;
#21329 = LINE ( 'NONE', #9961, #19864 ) ;
#21330 = ORIENTED_EDGE ( 'NONE', *, *, #39827, .T. ) ;
#21331 = CARTESIAN_POINT ( 'NONE',  ( -1.363819533518803473, 3.267716535433071279, -0.6692913385826760875 ) ) ;
#21332 = LINE ( 'NONE', #41458, #27798 ) ;
#21333 = EDGE_LOOP ( 'NONE', ( #48278, #4462, #2294, #38755 ) ) ;
#21334 = LINE ( 'NONE', #9199, #41950 ) ;
#21335 = VECTOR ( 'NONE', #22114, 39.37007874015748143 ) ;
#21336 = LINE ( 'NONE', #25454, #21008 ) ;
#21337 = CARTESIAN_POINT ( 'NONE',  ( 1.909347346926324684, 3.346456692913386100, 0.7874015748031456541 ) ) ;
#21338 = ORIENTED_EDGE ( 'NONE', *, *, #30133, .T. ) ;
#21339 = DIRECTION ( 'NONE',  ( -1.729310098865080642E-17, 1.000000000000000000, 1.276627980444840260E-16 ) ) ;
#21340 = ORIENTED_EDGE ( 'NONE', *, *, #9700, .F. ) ;
#21341 = FACE_BOUND ( 'NONE', #40213, .T. ) ;
#21342 = LINE ( 'NONE', #12833, #8617 ) ;
#21343 = B_SPLINE_CURVE_WITH_KNOTS ( 'NONE', 3,
 ( #35194, #49876, #50873, #3698 ),
 .UNSPECIFIED., .F., .F.,
 ( 4, 4 ),
 ( 2.034061690683489341E-07, 0.002500755411796015595 ),
 .UNSPECIFIED. ) ;
#21344 = VECTOR ( 'NONE', #45960, 39.37007874015748143 ) ;
#21345 = AXIS2_PLACEMENT_3D ( 'NONE', #32532, #8763, #25020 ) ;
#21346 = CARTESIAN_POINT ( 'NONE',  ( 0.4696143004045484348, 0.000000000000000000, 2.165354330708650910 ) ) ;
#21347 = CARTESIAN_POINT ( 'NONE',  ( 0.8182917201112819283, 3.346456692913386100, 0.4724409448818868706 ) ) ;
#21348 = ADVANCED_FACE ( 'NONE', ( #40102 ), #19444, .T. ) ;
#21349 = ORIENTED_EDGE ( 'NONE', *, *, #1144, .T. ) ;
#21350 = ORIENTED_EDGE ( 'NONE', *, *, #15196, .F. ) ;
#21351 = DIRECTION ( 'NONE',  ( 0.000000000000000000, 0.000000000000000000, 1.000000000000000000 ) ) ;
#21352 = VERTEX_POINT ( 'NONE', #50890 ) ;
#21353 = AXIS2_PLACEMENT_3D ( 'NONE', #21642, #13897, #19027 ) ;
#21354 = DIRECTION ( 'NONE',  ( 1.000000000000000000, 0.000000000000000000, 0.000000000000000000 ) ) ;
#21355 = VERTEX_POINT ( 'NONE', #15587 ) ;
#21356 = EDGE_CURVE ( 'NONE', #26492, #37481, #47033, .T. ) ;
#21357 = DIRECTION ( 'NONE',  ( -0.000000000000000000, 0.000000000000000000, 1.000000000000000000 ) ) ;
#21358 = ADVANCED_FACE ( 'NONE', ( #11961 ), #31853, .F. ) ;
#21359 = ORIENTED_EDGE ( 'NONE', *, *, #26647, .F. ) ;
#21360 = CARTESIAN_POINT ( 'NONE',  ( 1.015142113812069979, 0.000000000000000000, 1.417322834645662777 ) ) ;
#21361 = EDGE_CURVE ( 'NONE', #44686, #33629, #43694, .T. ) ;
#21362 = DIRECTION ( 'NONE',  ( -1.000000000000000000, 0.000000000000000000, 0.000000000000000000 ) ) ;
#21363 = ORIENTED_EDGE ( 'NONE', *, *, #7955, .T. ) ;
#21364 = EDGE_CURVE ( 'NONE', #10525, #34229, #13700, .T. ) ;
#21365 = DIRECTION ( 'NONE',  ( -0.1785568947986229116, 0.000000000000000000, -0.9839295885986321100 ) ) ;
#21366 = ORIENTED_EDGE ( 'NONE', *, *, #14414, .T. ) ;
#21367 = ORIENTED_EDGE ( 'NONE', *, *, #44581, .F. ) ;
#21368 = AXIS2_PLACEMENT_3D ( 'NONE', #50613, #27169, #44189 ) ;
#21369 = ORIENTED_EDGE ( 'NONE', *, *, #46822, .F. ) ;
#21370 = ORIENTED_EDGE ( 'NONE', *, *, #45917, .F. ) ;
#21371 = CARTESIAN_POINT ( 'NONE',  ( 0.08139965876239094178, 1.610780518492231694, 0.000000000000000000 ) ) ;
#21372 = ORIENTED_EDGE ( 'NONE', *, *, #21625, .T. ) ;
#21373 = LINE ( 'NONE', #45851, #35309 ) ;
#21374 = ORIENTED_EDGE ( 'NONE', *, *, #18150, .F. ) ;
#21375 = DIRECTION ( 'NONE',  ( -1.000000000000000000, 0.000000000000000000, 0.000000000000000000 ) ) ;
#21376 = ADVANCED_FACE ( 'NONE', ( #35714 ), #4730, .T. ) ;
#21377 = VECTOR ( 'NONE', #27198, 39.37007874015748143 ) ;
#21378 = FACE_OUTER_BOUND ( 'NONE', #6168, .T. ) ;
#21379 = ADVANCED_FACE ( 'NONE', ( #40863 ), #9366, .F. ) ;
#21380 = VECTOR ( 'NONE', #43982, 39.37007874015748143 ) ;
#21381 = EDGE_LOOP ( 'NONE', ( #2761, #43179, #4711, #46213 ) ) ;
#21382 = CARTESIAN_POINT ( 'NONE',  ( -1.363819533518803029, 0.000000000000000000, 0.5905511811023582691 ) ) ;
#21383 = CARTESIAN_POINT ( 'NONE',  ( 1.015142113812069979, 3.267716535433071279, 1.732283464566921172 ) ) ;
#21384 = EDGE_CURVE ( 'NONE', #23897, #38926, #29749, .T. ) ;
#21385 = VERTEX_POINT ( 'NONE', #33388 ) ;
#21386 = CARTESIAN_POINT ( 'NONE',  ( 2.312113436335841321, 1.646509482104762334, 0.2635349935491774209 ) ) ;
#21387 = DIRECTION ( 'NONE',  ( -1.000000000000000000, 0.000000000000000000, 1.734723475976806848E-16 ) ) ;
#21388 = CIRCLE ( 'NONE', #50150, 2.164630168518208109 ) ;
#21389 = CARTESIAN_POINT ( 'NONE',  ( 1.636583440222563635, 3.346456692913386100, -1.456692913385823296 ) ) ;
#21390 = DIRECTION ( 'NONE',  ( 0.1785568947986229116, 0.000000000000000000, 0.9839295885986321100 ) ) ;
#21391 = PLANE ( 'NONE',  #48196 ) ;
#21392 = EDGE_LOOP ( 'NONE', ( #12793, #28850, #43395, #6388 ) ) ;
#21393 = CARTESIAN_POINT ( 'NONE',  ( 1.015142113812069313, 3.267716535433071279, 0.7874015748031454320 ) ) ;
#21394 = CARTESIAN_POINT ( 'NONE',  ( -0.07591351300297284610, 3.346456692913386100, 1.220472440944875281 ) ) ;
#21395 = ORIENTED_EDGE ( 'NONE', *, *, #44054, .T. ) ;
#21396 = CARTESIAN_POINT ( 'NONE',  ( 2.094031212354920957, 3.223341107052878574, -1.299212598425194320 ) ) ;
#21397 = ORIENTED_EDGE ( 'NONE', *, *, #40399, .F. ) ;
#21398 = CARTESIAN_POINT ( 'NONE',  ( 1.287906020515830141, 0.000000000000000000, 0.7480314960629872445 ) ) ;
#21399 = FACE_OUTER_BOUND ( 'NONE', #29039, .T. ) ;
#21400 = DIRECTION ( 'NONE',  ( -9.390536051998764103E-17, -1.000000000000000000, -6.822623802544789917E-17 ) ) ;
#21401 = DIRECTION ( 'NONE',  ( -0.000000000000000000, 1.000000000000000000, -0.000000000000000000 ) ) ;
#21402 = DIRECTION ( 'NONE',  ( -0.000000000000000000, 1.000000000000000000, -0.000000000000000000 ) ) ;
#21403 = VECTOR ( 'NONE', #26046, 39.37007874015748143 ) ;
#21404 = ORIENTED_EDGE ( 'NONE', *, *, #40207, .F. ) ;
#21405 = DIRECTION ( 'NONE',  ( -3.469446951953613696E-16, 0.000000000000000000, -1.000000000000000000 ) ) ;
#21406 = CARTESIAN_POINT ( 'NONE',  ( -0.7148041136150262709, 1.205361022782829114E-17, -2.044646019095620826 ) ) ;
#21407 = CARTESIAN_POINT ( 'NONE',  ( 2.387237949294865214, 0.9877775034572128243, -1.073873893196610751 ) ) ;
#21408 = VERTEX_POINT ( 'NONE', #24859 ) ;
#21409 = DIRECTION ( 'NONE',  ( 1.000000000000000000, 0.000000000000000000, 0.000000000000000000 ) ) ;
#21410 = EDGE_LOOP ( 'NONE', ( #17318, #39879, #43966, #43891 ) ) ;
#21411 = VECTOR ( 'NONE', #11142, 39.37007874015748143 ) ;
#21412 = LINE ( 'NONE', #48223, #49079 ) ;
#21413 = PLANE ( 'NONE',  #31367 ) ;
#21414 = EDGE_CURVE ( 'NONE', #43528, #9319, #44468, .T. ) ;
#21415 = CARTESIAN_POINT ( 'NONE',  ( 0.000000000000000000, 3.267716535433071279, -0.7874015748031473194 ) ) ;
#21416 = ADVANCED_FACE ( 'NONE', ( #48567 ), #14006, .T. ) ;
#21417 = EDGE_CURVE ( 'NONE', #4560, #40528, #1400, .T. ) ;
#21418 = DIRECTION ( 'NONE',  ( -1.000000000000000000, 0.000000000000000000, 1.734723475976806848E-16 ) ) ;
#21419 = ORIENTED_EDGE ( 'NONE', *, *, #12097, .F. ) ;
#21420 = ORIENTED_EDGE ( 'NONE', *, *, #45563, .F. ) ;
#21421 = DIRECTION ( 'NONE',  ( -0.000000000000000000, 1.000000000000000000, -0.000000000000000000 ) ) ;
#21422 = LINE ( 'NONE', #48231, #46257 ) ;
#21423 = FACE_BOUND ( 'NONE', #35307, .T. ) ;
#21424 = ORIENTED_EDGE ( 'NONE', *, *, #30715, .F. ) ;
#21425 = CARTESIAN_POINT ( 'NONE',  ( -1.091055626815042423, 3.267716535433071279, 1.892679809432644143E-16 ) ) ;
#21426 = LINE ( 'NONE', #5419, #1948 ) ;
#21427 = ORIENTED_EDGE ( 'NONE', *, *, #4108, .F. ) ;
#21428 = ORIENTED_EDGE ( 'NONE', *, *, #36691, .F. ) ;
#21429 = CARTESIAN_POINT ( 'NONE',  ( 0.8182917201112819283, 3.346456692913386100, -1.299212598425193210 ) ) ;
#21430 = CARTESIAN_POINT ( 'NONE',  ( 2.122091976112992828, 0.000000000000000000, 0.4338754535133130252 ) ) ;
#21431 = ORIENTED_EDGE ( 'NONE', *, *, #50978, .T. ) ;
#21432 = VERTEX_POINT ( 'NONE', #21753 ) ;
#21433 = EDGE_CURVE ( 'NONE', #9566, #41713, #41372, .T. ) ;
#21434 = VERTEX_POINT ( 'NONE', #17119 ) ;
#21435 = CARTESIAN_POINT ( 'NONE',  ( -2.101376631542743567, 1.608627760585161992, -0.5301036954757798458 ) ) ;
#21436 = DIRECTION ( 'NONE',  ( -0.000000000000000000, -1.000000000000000000, -0.000000000000000000 ) ) ;
#21437 = EDGE_CURVE ( 'NONE', #16692, #42434, #20987, .T. ) ;
#21438 = VECTOR ( 'NONE', #33695, 39.37007874015748143 ) ;
#21439 = CARTESIAN_POINT ( 'NONE',  ( 2.179222933086670366, 5.118110236220475784, 2.848360286204476122 ) ) ;
#21440 = FACE_OUTER_BOUND ( 'NONE', #15570, .T. ) ;
#21441 = EDGE_CURVE ( 'NONE', #36917, #1405, #5234, .T. ) ;
#21442 = ORIENTED_EDGE ( 'NONE', *, *, #49539, .F. ) ;
#21443 = ORIENTED_EDGE ( 'NONE', *, *, #42236, .T. ) ;
#21444 = CARTESIAN_POINT ( 'NONE',  ( 0.000000000000000000, 3.267716535433071279, 1.102362204724404160 ) ) ;
#21445 = LINE ( 'NONE', #40038, #27104 ) ;
#21446 = EDGE_CURVE ( 'NONE', #8605, #11744, #44711, .T. ) ;
#21447 = CARTESIAN_POINT ( 'NONE',  ( 1.253212129322610613, 3.346456692913386100, 1.692913385826762873 ) ) ;
#21448 = CARTESIAN_POINT ( 'NONE',  ( 0.5455278134075217666, 3.346456692913386100, 1.889763779527550369 ) ) ;
#21449 = LINE ( 'NONE', #26334, #9174 ) ;
#21450 = AXIS2_PLACEMENT_3D ( 'NONE', #28602, #35846, #24486 ) ;
#21451 = VECTOR ( 'NONE', #5363, 39.37007874015748143 ) ;
#21452 = FACE_OUTER_BOUND ( 'NONE', #8270, .T. ) ;
#21453 = CARTESIAN_POINT ( 'NONE',  ( -1.091055626815042645, 3.346456692913386100, -0.5118110236220467790 ) ) ;
#21454 = EDGE_LOOP ( 'NONE', ( #47902, #13839, #6850, #42456 ) ) ;
#21455 = DIRECTION ( 'NONE',  ( 0.000000000000000000, 0.000000000000000000, -1.000000000000000000 ) ) ;
#21456 = DIRECTION ( 'NONE',  ( 0.000000000000000000, -1.000000000000000000, 0.000000000000000000 ) ) ;
#21457 = VECTOR ( 'NONE', #36971, 39.37007874015748143 ) ;
#21458 = ORIENTED_EDGE ( 'NONE', *, *, #14564, .F. ) ;
#21459 = VERTEX_POINT ( 'NONE', #32618 ) ;
#21460 = CARTESIAN_POINT ( 'NONE',  ( -1.905671854841497481, 1.689559879305088996, 2.256015092822653223 ) ) ;
#21461 = LINE ( 'NONE', #44930, #42651 ) ;
#21462 = ORIENTED_EDGE ( 'NONE', *, *, #45287, .T. ) ;
#21463 = VERTEX_POINT ( 'NONE', #13754 ) ;
#21464 = CARTESIAN_POINT ( 'NONE',  ( 0.000000000000000000, 3.267716535433071279, -0.9842519685039344823 ) ) ;
#21465 = ORIENTED_EDGE ( 'NONE', *, *, #30272, .F. ) ;
#21466 = CARTESIAN_POINT ( 'NONE',  ( 1.091055626815042645, 0.000000000000000000, 0.6299212598425161236 ) ) ;
#21467 = DIRECTION ( 'NONE',  ( -3.469446951953613696E-16, 0.000000000000000000, -1.000000000000000000 ) ) ;
#21468 = ORIENTED_EDGE ( 'NONE', *, *, #30297, .T. ) ;
#21469 = EDGE_CURVE ( 'NONE', #3514, #23810, #30342, .T. ) ;
#21470 = ORIENTED_EDGE ( 'NONE', *, *, #47915, .T. ) ;
#21471 = ORIENTED_EDGE ( 'NONE', *, *, #45938, .T. ) ;
#21472 = CARTESIAN_POINT ( 'NONE',  ( 0.7423782071083087075, 3.267716535433071279, -2.575641807848710194E-16 ) ) ;
#21473 = EDGE_CURVE ( 'NONE', #16692, #4787, #17623, .T. ) ;
#21474 = VERTEX_POINT ( 'NONE', #40363 ) ;
#21475 = ORIENTED_EDGE ( 'NONE', *, *, #40290, .F. ) ;
#21476 = DIRECTION ( 'NONE',  ( -1.000000000000000000, 0.000000000000000000, 0.000000000000000000 ) ) ;
#21477 = CARTESIAN_POINT ( 'NONE',  ( 1.560669927219590747, 0.000000000000000000, 0.7874015748031454320 ) ) ;
#21478 = CARTESIAN_POINT ( 'NONE',  ( 0.3632705576371071388, 0.000000000000000000, -0.07179618730611768418 ) ) ;
#21479 = EDGE_CURVE ( 'NONE', #3209, #48480, #48813, .T. ) ;
#21480 = VECTOR ( 'NONE', #19770, 39.37007874015748143 ) ;
#21481 = ORIENTED_EDGE ( 'NONE', *, *, #50377, .T. ) ;
#21482 = VECTOR ( 'NONE', #15311, 39.37007874015748143 ) ;
#21483 = FACE_OUTER_BOUND ( 'NONE', #49498, .T. ) ;
#21484 = DIRECTION ( 'NONE',  ( -0.9998717552508121775, -0.01601477604151182663, 0.000000000000000000 ) ) ;
#21485 = DIRECTION ( 'NONE',  ( 1.734723475976806848E-16, -0.000000000000000000, 1.000000000000000000 ) ) ;
#21486 = ORIENTED_EDGE ( 'NONE', *, *, #34309, .F. ) ;
#21487 = CARTESIAN_POINT ( 'NONE',  ( -1.062992125984251635, 0.000000000000000000, 1.014069264286641570 ) ) ;
#21488 = LINE ( 'NONE', #6511, #7120 ) ;
#21489 = DIRECTION ( 'NONE',  ( 0.4338837391175526803, 0.000000000000000000, 0.9009688679024218105 ) ) ;
#21490 = ORIENTED_EDGE ( 'NONE', *, *, #10614, .F. ) ;
#21491 = VERTEX_POINT ( 'NONE', #1869 ) ;
#21492 = VECTOR ( 'NONE', #10556, 39.37007874015748143 ) ;
#21493 = DIRECTION ( 'NONE',  ( 0.5128992774059071280, 9.962263361493005127E-17, -0.8584487936018655452 ) ) ;
#21494 = EDGE_CURVE ( 'NONE', #33100, #48369, #3267, .T. ) ;
#21495 = CARTESIAN_POINT ( 'NONE',  ( -0.3486774197067334380, 0.000000000000000000, 1.574803149606291974 ) ) ;
#21496 = LINE ( 'NONE', #22264, #30479 ) ;
#21497 = ORIENTED_EDGE ( 'NONE', *, *, #32466, .T. ) ;
#21498 = ORIENTED_EDGE ( 'NONE', *, *, #15529, .T. ) ;
#21499 = B_SPLINE_CURVE_WITH_KNOTS ( 'NONE', 3,
 ( #39166, #16190, #15670, #8695 ),
 .UNSPECIFIED., .F., .F.,
 ( 4, 4 ),
 ( 0.01458567687628280554, 0.03075035112464553563 ),
 .UNSPECIFIED. ) ;
#21500 = EDGE_CURVE ( 'NONE', #17906, #9076, #29235, .T. ) ;
#21501 = DIRECTION ( 'NONE',  ( 1.000000000000000000, 0.000000000000000000, 0.000000000000000000 ) ) ;
#21502 = ORIENTED_EDGE ( 'NONE', *, *, #854, .T. ) ;
#21503 = LINE ( 'NONE', #13253, #34862 ) ;
#21504 = DIRECTION ( 'NONE',  ( 0.2225209339563041788, -1.160734090543304660E-16, 0.9749279121818259508 ) ) ;
#21505 = DIRECTION ( 'NONE',  ( 0.9998717552508121775, 0.01601477604151182663, 0.000000000000000000 ) ) ;
#21506 = DIRECTION ( 'NONE',  ( 1.000000000000000000, -0.000000000000000000, 0.000000000000000000 ) ) ;
#21507 = DIRECTION ( 'NONE',  ( 0.000000000000000000, -1.000000000000000000, 0.000000000000000000 ) ) ;
#21508 = ORIENTED_EDGE ( 'NONE', *, *, #15344, .F. ) ;
#21509 = LINE ( 'NONE', #37270, #40702 ) ;
#21510 = LINE ( 'NONE', #49088, #26047 ) ;
#21511 = CARTESIAN_POINT ( 'NONE',  ( 0.000000000000000000, 3.346456692913386100, 0.000000000000000000 ) ) ;
#21512 = VECTOR ( 'NONE', #37907, 39.37007874015748143 ) ;
#21513 = VERTEX_POINT ( 'NONE', #36740 ) ;
#21514 = LINE ( 'NONE', #48331, #27331 ) ;
#21515 = AXIS2_PLACEMENT_3D ( 'NONE', #1226, #12851, #40475 ) ;
#21516 = DIRECTION ( 'NONE',  ( -0.000000000000000000, -1.000000000000000000, -0.000000000000000000 ) ) ;
#21517 = DIRECTION ( 'NONE',  ( -0.7530714660036196273, 0.000000000000000000, 0.6579387259397027066 ) ) ;
#21518 = ORIENTED_EDGE ( 'NONE', *, *, #2686, .T. ) ;
#21519 = DIRECTION ( 'NONE',  ( -3.469446951953613696E-16, 0.000000000000000000, -1.000000000000000000 ) ) ;
#21520 = LINE ( 'NONE', #40393, #47271 ) ;
#21521 = ORIENTED_EDGE ( 'NONE', *, *, #39418, .F. ) ;
#21522 = DIRECTION ( 'NONE',  ( -0.7071067811865466846, -0.7071067811865483499, -6.409875621278517705E-17 ) ) ;
#21523 = AXIS2_PLACEMENT_3D ( 'NONE', #15875, #43232, #43488 ) ;
#21525 = DIRECTION ( 'NONE',  ( -0.000000000000000000, 1.000000000000000000, -0.000000000000000000 ) ) ;
#21524 = B_SPLINE_CURVE_WITH_KNOTS ( 'NONE', 3,
 ( #23591, #14844, #15094, #35474 ),
 .UNSPECIFIED., .F., .F.,
 ( 4, 4 ),
 ( 0.1211775127643062860, 0.1625894504277921315 ),
 .UNSPECIFIED. ) ;
#21526 = ORIENTED_EDGE ( 'NONE', *, *, #19765, .F. ) ;
#21527 = FACE_OUTER_BOUND ( 'NONE', #39481, .T. ) ;
#21528 = CARTESIAN_POINT ( 'NONE',  ( 1.068402561569974374, 5.905511811023623991, -1.884154513482173110 ) ) ;
#21529 = CARTESIAN_POINT ( 'NONE',  ( -1.091055626815042201, 0.000000000000000000, 0.7480314960629874665 ) ) ;
#21530 = CARTESIAN_POINT ( 'NONE',  ( 0.000000000000000000, 3.267716535433071279, -0.1574803149606304187 ) ) ;
#21531 = CARTESIAN_POINT ( 'NONE',  ( 0.000000000000000000, 3.267716535433071279, -1.141732283464564013 ) ) ;
#21532 = EDGE_CURVE ( 'NONE', #27988, #37613, #5997, .T. ) ;
#21533 = ORIENTED_EDGE ( 'NONE', *, *, #35445, .T. ) ;
#21534 = EDGE_LOOP ( 'NONE', ( #36743, #28414, #5597, #5449 ) ) ;
#21535 = FACE_OUTER_BOUND ( 'NONE', #28839, .T. ) ;
#21536 = CARTESIAN_POINT ( 'NONE',  ( -1.593029370565769431, 3.346456692913386100, 1.377952755905504256 ) ) ;
#21537 = EDGE_CURVE ( 'NONE', #19452, #29807, #37510, .T. ) ;
#21538 = ORIENTED_EDGE ( 'NONE', *, *, #3585, .T. ) ;
#21539 = DIRECTION ( 'NONE',  ( -0.9749279121818227312, 0.000000000000000000, -0.2225209339563184452 ) ) ;
#21540 = DIRECTION ( 'NONE',  ( 1.000000000000000000, -0.000000000000000000, 0.000000000000000000 ) ) ;
#21541 = CARTESIAN_POINT ( 'NONE',  ( 2.339241080213585899, 1.657243480315735873, 1.802537235681917815 ) ) ;
#21542 = EDGE_CURVE ( 'NONE', #13472, #1865, #37114, .T. ) ;
#21543 = ORIENTED_EDGE ( 'NONE', *, *, #40571, .F. ) ;
#21544 = ORIENTED_EDGE ( 'NONE', *, *, #41543, .F. ) ;
#21545 = EDGE_CURVE ( 'NONE', #9586, #47188, #50082, .T. ) ;
#21546 = CARTESIAN_POINT ( 'NONE',  ( -2.165460538733998241, 1.205361022782829114E-17, 0.04798874274652762534 ) ) ;
#21547 = FACE_OUTER_BOUND ( 'NONE', #39433, .T. ) ;
#21548 = CARTESIAN_POINT ( 'NONE',  ( 1.015142113812069091, 3.346456692913386100, -1.417322834645664331 ) ) ;
#21549 = EDGE_CURVE ( 'NONE', #4697, #32558, #22508, .T. ) ;
#21550 = EDGE_LOOP ( 'NONE', ( #886, #19874, #35197, #16106 ) ) ;
#21551 = DIRECTION ( 'NONE',  ( -0.6234898018587318180, 0.000000000000000000, -0.7818314824680309139 ) ) ;
#21552 = FACE_BOUND ( 'NONE', #36185, .T. ) ;
#21553 = VERTEX_POINT ( 'NONE', #6763 ) ;
#21554 = CARTESIAN_POINT ( 'NONE',  ( -2.454875160333845674, 0.000000000000000000, -0.1574803149606298636 ) ) ;
#21555 = ORIENTED_EDGE ( 'NONE', *, *, #17246, .F. ) ;
#21556 = ORIENTED_EDGE ( 'NONE', *, *, #40550, .F. ) ;
#21557 = VECTOR ( 'NONE', #977, 39.37007874015748143 ) ;
#21558 = CARTESIAN_POINT ( 'NONE',  ( 0.07982360342473591996, 1.709180471932028711, 0.000000000000000000 ) ) ;
#21559 = CARTESIAN_POINT ( 'NONE',  ( -1.363819533518803029, 3.346456692913386100, 0.2755905511810996522 ) ) ;
#21560 = AXIS2_PLACEMENT_3D ( 'NONE', #49657, #7102, #19213 ) ;
#21561 = AXIS2_PLACEMENT_3D ( 'NONE', #11259, #26990, #7388 ) ;
#21562 = EDGE_CURVE ( 'NONE', #25006, #20856, #798, .T. ) ;
#21563 = ORIENTED_EDGE ( 'NONE', *, *, #48755, .F. ) ;
#21564 = LINE ( 'NONE', #9435, #6314 ) ;
#21565 = UNCERTAINTY_MEASURE_WITH_UNIT (LENGTH_MEASURE( 1.000000000000000082E-05 ), #25362, 'distance_accuracy_value', 'NONE');
#21566 = CARTESIAN_POINT ( 'NONE',  ( 0.8182917201112819283, 0.000000000000000000, 0.5905511811023579360 ) ) ;
#21567 = ORIENTED_EDGE ( 'NONE', *, *, #1102, .F. ) ;
#21568 = CIRCLE ( 'NONE', #33958, 2.246510896728926010 ) ;
#21569 = EDGE_CURVE ( 'NONE', #11282, #34114, #4448, .T. ) ;
#21570 = VECTOR ( 'NONE', #46951, 39.37007874015748143 ) ;
#21571 = DIRECTION ( 'NONE',  ( 0.000000000000000000, 0.000000000000000000, -1.000000000000000000 ) ) ;
#21572 = CARTESIAN_POINT ( 'NONE',  ( -1.024442997624132911E-17, 3.267716535433071279, 1.777125317778635541E-33 ) ) ;
#21573 = VECTOR ( 'NONE', #1704, 39.37007874015748143 ) ;
#21574 = EDGE_CURVE ( 'NONE', #33100, #22384, #48763, .T. ) ;
#21575 = PLANE ( 'NONE',  #45372 ) ;
#21576 = LINE ( 'NONE', #17445, #2246 ) ;
#21577 = CARTESIAN_POINT ( 'NONE',  ( 0.1450934409768589450, 1.205361022782829114E-17, 2.161127057262026252 ) ) ;
#21578 = ORIENTED_EDGE ( 'NONE', *, *, #19422, .F. ) ;
#21579 = CARTESIAN_POINT ( 'NONE',  ( -1.091055626815042423, 3.267716535433071279, 1.892679809432644143E-16 ) ) ;
#21580 = EDGE_CURVE ( 'NONE', #24780, #36033, #6257, .T. ) ;
#21581 = DIRECTION ( 'NONE',  ( -3.986037398843765983E-20, -1.000000000000000000, -1.160734090543304660E-16 ) ) ;
#21582 = VERTEX_POINT ( 'NONE', #34394 ) ;
#21583 = FACE_OUTER_BOUND ( 'NONE', #8052, .T. ) ;
#21584 = DIRECTION ( 'NONE',  ( 0.000000000000000000, -1.000000000000000000, 0.000000000000000000 ) ) ;
#21585 = VERTEX_POINT ( 'NONE', #38018 ) ;
#21586 = CARTESIAN_POINT ( 'NONE',  ( 0.002207914879453961535, -5.712274067634378313E-18, 0.04916304461325374242 ) ) ;
#21587 = DIRECTION ( 'NONE',  ( 0.000000000000000000, -1.000000000000000000, 0.000000000000000000 ) ) ;
#21588 = CARTESIAN_POINT ( 'NONE',  ( 2.378961647330872786, 3.346456692913386100, -0.1968503937007886062 ) ) ;
#21589 = EDGE_LOOP ( 'NONE', ( #25340, #18740, #41502, #33428 ) ) ;
#21590 = CARTESIAN_POINT ( 'NONE',  ( 0.4696143004045476022, 3.346456692913386100, -2.244094488188969727 ) ) ;
#21591 = ORIENTED_EDGE ( 'NONE', *, *, #27063, .F. ) ;
#21592 = FACE_BOUND ( 'NONE', #9814, .T. ) ;
#21593 = CARTESIAN_POINT ( 'NONE',  ( -1.712496953225537188, 0.000000000000000000, 1.102362204724404160 ) ) ;
#21594 = AXIS2_PLACEMENT_3D ( 'NONE', #12487, #11980, #27717 ) ;
#21595 = VECTOR ( 'NONE', #50878, 39.37007874015748143 ) ;
#21596 = DIRECTION ( 'NONE',  ( -0.000000000000000000, 1.000000000000000000, -0.000000000000000000 ) ) ;
#21597 = CARTESIAN_POINT ( 'NONE',  ( -0.3595914698493425377, 0.000000000000000000, 1.705899337635481405 ) ) ;
#21598 = VECTOR ( 'NONE', #27420, 39.37007874015748143 ) ;
#21599 = ORIENTED_EDGE ( 'NONE', *, *, #8818, .T. ) ;
#21600 = ORIENTED_EDGE ( 'NONE', *, *, #12108, .T. ) ;
#21601 = CARTESIAN_POINT ( 'NONE',  ( -0.5455278134075208785, 0.000000000000000000, 1.062992125984246083 ) ) ;
#21602 = ORIENTED_EDGE ( 'NONE', *, *, #45638, .F. ) ;
#21603 = VECTOR ( 'NONE', #24974, 39.37007874015748143 ) ;
#21604 = LINE ( 'NONE', #37617, #41730 ) ;
#21605 = VERTEX_POINT ( 'NONE', #23016 ) ;
#21606 = ADVANCED_FACE ( 'NONE', ( #50324 ), #22010, .F. ) ;
#21607 = FACE_OUTER_BOUND ( 'NONE', #40478, .T. ) ;
#21608 = VECTOR ( 'NONE', #35994, 39.37007874015748143 ) ;
#21609 = ORIENTED_EDGE ( 'NONE', *, *, #22330, .F. ) ;
#21610 = LINE ( 'NONE', #22375, #5147 ) ;
#21611 = EDGE_CURVE ( 'NONE', #20741, #606, #18380, .T. ) ;
#21612 = CARTESIAN_POINT ( 'NONE',  ( 1.539674616754186820, 0.000000000000000000, -1.403993126671013059 ) ) ;
#21613 = ORIENTED_EDGE ( 'NONE', *, *, #50525, .T. ) ;
#21614 = CARTESIAN_POINT ( 'NONE',  ( -0.5433753726466064027, 1.710786698518002913, 2.902374844046801350 ) ) ;
#21615 = VERTEX_POINT ( 'NONE', #45467 ) ;
#21616 = ORIENTED_EDGE ( 'NONE', *, *, #35364, .T. ) ;
#21617 = B_SPLINE_CURVE_WITH_KNOTS ( 'NONE', 3,
 ( #17785, #1779, #4434, #40332 ),
 .UNSPECIFIED., .F., .F.,
 ( 4, 4 ),
 ( 3.758775566991543122E-07, 0.04545307989631656997 ),
 .UNSPECIFIED. ) ;
#21618 = VERTEX_POINT ( 'NONE', #7274 ) ;
#21619 = EDGE_LOOP ( 'NONE', ( #2596, #8196, #2978, #48770 ) ) ;
#21620 = CARTESIAN_POINT ( 'NONE',  ( 2.685986181519757210, 5.118110236220475784, -1.228718213908073897 ) ) ;
#21621 = VERTEX_POINT ( 'NONE', #34141 ) ;
#21622 = CARTESIAN_POINT ( 'NONE',  ( -2.734482843737247926, 5.905511811023623991, -1.115254632218712683 ) ) ;
#21623 = CARTESIAN_POINT ( 'NONE',  ( -1.712496953225537633, 3.346456692913386100, -0.7874015748031470974 ) ) ;
#21624 = AXIS2_PLACEMENT_3D ( 'NONE', #3075, #51010, #26315 ) ;
#21625 = EDGE_CURVE ( 'NONE', #18215, #28527, #34630, .T. ) ;
#21626 = FACE_OUTER_BOUND ( 'NONE', #21244, .T. ) ;
#21627 = ORIENTED_EDGE ( 'NONE', *, *, #12536, .T. ) ;
#21628 = VECTOR ( 'NONE', #42490, 39.37007874015748143 ) ;
#21629 = CARTESIAN_POINT ( 'NONE',  ( 1.905671854841463952, 1.472358791367697650, 2.256015092822682089 ) ) ;
#21630 = DIRECTION ( 'NONE',  ( 0.000000000000000000, -1.000000000000000000, 0.000000000000000000 ) ) ;
#21631 = ORIENTED_EDGE ( 'NONE', *, *, #18459, .T. ) ;
#21632 = LINE ( 'NONE', #33527, #23278 ) ;
#21633 = CARTESIAN_POINT ( 'NONE',  ( 0.7423782071083084855, 0.000000000000000000, -1.574803149606293529 ) ) ;
#21634 = VECTOR ( 'NONE', #13305, 39.37007874015748143 ) ;
#21635 = PLANE ( 'NONE',  #2094 ) ;
#21636 = ADVANCED_FACE ( 'NONE', ( #30762 ), #32748, .T. ) ;
#21637 = CARTESIAN_POINT ( 'NONE',  ( 1.979793062125284830, 1.205361022782829114E-17, 2.191257344206568813 ) ) ;
#21638 = VECTOR ( 'NONE', #36442, 39.37007874015748143 ) ;
#21639 = CARTESIAN_POINT ( 'NONE',  ( 0.7506868623604561197, 1.205361022782829114E-17, 1.860140722251951484 ) ) ;
#21640 = DIRECTION ( 'NONE',  ( 0.000000000000000000, 0.000000000000000000, 1.000000000000000000 ) ) ;
#21641 = VERTEX_POINT ( 'NONE', #26378 ) ;
#21642 = CARTESIAN_POINT ( 'NONE',  ( 0.08119777152254364916, 1.623385212329073957, 0.000000000000000000 ) ) ;
#21643 = EDGE_CURVE ( 'NONE', #337, #23167, #30004, .T. ) ;
#21644 = LINE ( 'NONE', #18026, #21828 ) ;
#21645 = ORIENTED_EDGE ( 'NONE', *, *, #21663, .F. ) ;
#21646 = DIRECTION ( 'NONE',  ( -1.000000000000000000, 0.000000000000000000, 0.000000000000000000 ) ) ;
#21647 = EDGE_CURVE ( 'NONE', #46376, #35776, #26870, .T. ) ;
#21648 = ORIENTED_EDGE ( 'NONE', *, *, #36897, .T. ) ;
#21649 = CARTESIAN_POINT ( 'NONE',  ( -2.318785326865331342, 1.584680398590042172, 1.828187939057640321 ) ) ;
#21650 = ADVANCED_FACE ( 'NONE', ( #42626 ), #30260, .T. ) ;
#21651 = DIRECTION ( 'NONE',  ( -1.000000000000000000, -0.000000000000000000, -0.000000000000000000 ) ) ;
#21652 = CARTESIAN_POINT ( 'NONE',  ( -0.3742159057234073494, 0.02192591290182492950, 1.786486621533327712 ) ) ;
#21653 = CARTESIAN_POINT ( 'NONE',  ( -1.195183497228115035E-16, 3.346456692913386100, 0.6299212598425161236 ) ) ;
#21654 = LINE ( 'NONE', #34549, #8768 ) ;
#21655 = VERTEX_POINT ( 'NONE', #10385 ) ;
#21656 = DIRECTION ( 'NONE',  ( -0.9998717552508122886, -0.01601477604151180928, 0.000000000000000000 ) ) ;
#21657 = ORIENTED_EDGE ( 'NONE', *, *, #12931, .F. ) ;
#21658 = FACE_OUTER_BOUND ( 'NONE', #18602, .T. ) ;
#21659 = ORIENTED_EDGE ( 'NONE', *, *, #6593, .F. ) ;
#21660 = CARTESIAN_POINT ( 'NONE',  ( -1.293618082698012151, 0.000000000000000000, -1.168738992012460898 ) ) ;
#21661 = CARTESIAN_POINT ( 'NONE',  ( 1.635196357930355893, 0.5249316497054298258, 0.9358222698459752742 ) ) ;
#21662 = EDGE_LOOP ( 'NONE', ( #31294, #36790, #35377, #37954 ) ) ;
#21663 = EDGE_CURVE ( 'NONE', #17447, #24413, #45977, .T. ) ;
#21664 = CARTESIAN_POINT ( 'NONE',  ( -1.353122744573580727, 3.346456692913386100, -1.614173228346451605 ) ) ;
#21665 = VECTOR ( 'NONE', #16535, 39.37007874015748854 ) ;
#21666 = DIRECTION ( 'NONE',  ( -1.000000000000000000, 0.000000000000000000, -0.000000000000000000 ) ) ;
#21667 = EDGE_CURVE ( 'NONE', #30309, #32429, #270, .T. ) ;
#21668 = EDGE_CURVE ( 'NONE', #10066, #32836, #37686, .T. ) ;
#21669 = AXIS2_PLACEMENT_3D ( 'NONE', #23950, #39955, #39697 ) ;
#21670 = CARTESIAN_POINT ( 'NONE',  ( 0.5455278134075211005, 3.267716535433071279, -0.8267716535433055070 ) ) ;
#21671 = EDGE_CURVE ( 'NONE', #9761, #4026, #11393, .T. ) ;
#21672 = ORIENTED_EDGE ( 'NONE', *, *, #7095, .T. ) ;
#21673 = ORIENTED_EDGE ( 'NONE', *, *, #25489, .F. ) ;
#21675 = CARTESIAN_POINT ( 'NONE',  ( -1.377952755905511362, 0.000000000000000000, -1.968503937007874516 ) ) ;
#21674 = AXIS2_PLACEMENT_3D ( 'NONE', #9272, #5140, #1777 ) ;
#21676 = FACE_BOUND ( 'NONE', #32855, .T. ) ;
#21677 = VERTEX_POINT ( 'NONE', #4664 ) ;
#21678 = VECTOR ( 'NONE', #2011, 39.37007874015748143 ) ;
#21679 = DIRECTION ( 'NONE',  ( 0.9998717552508121775, 0.01601477604151182663, 0.000000000000000000 ) ) ;
#21680 = DIRECTION ( 'NONE',  ( -1.000000000000000000, 0.000000000000000000, 1.734723475976806848E-16 ) ) ;
#21681 = ORIENTED_EDGE ( 'NONE', *, *, #48681, .T. ) ;
#21682 = EDGE_LOOP ( 'NONE', ( #34350, #44220, #5858, #11030 ) ) ;
#21683 = ADVANCED_FACE ( 'NONE', ( #4152 ), #20406, .F. ) ;
#21684 = LINE ( 'NONE', #6188, #3492 ) ;
#21685 = AXIS2_PLACEMENT_3D ( 'NONE', #38401, #18526, #6900 ) ;
#21686 = LINE ( 'NONE', #21177, #3938 ) ;
#21687 = ORIENTED_EDGE ( 'NONE', *, *, #35919, .T. ) ;
#21688 = EDGE_LOOP ( 'NONE', ( #22382, #35940, #22282, #20885 ) ) ;
#21689 = ORIENTED_EDGE ( 'NONE', *, *, #18833, .F. ) ;
#21690 = LINE ( 'NONE', #3329, #8725 ) ;
#21691 = DIRECTION ( 'NONE',  ( 1.000000000000000000, -0.000000000000000000, 0.000000000000000000 ) ) ;
#21692 = DIRECTION ( 'NONE',  ( -0.9998717552508122886, -0.01601477604151180928, 0.000000000000000000 ) ) ;
#21693 = ADVANCED_FACE ( 'NONE', ( #39519 ), #11895, .F. ) ;
#21694 = CARTESIAN_POINT ( 'NONE',  ( -1.712496953225537188, 0.000000000000000000, 0.7874015748031456541 ) ) ;
#21695 = ORIENTED_EDGE ( 'NONE', *, *, #47814, .T. ) ;
#21696 = ORIENTED_EDGE ( 'NONE', *, *, #49008, .F. ) ;
#21697 = LINE ( 'NONE', #25563, #41470 ) ;
#21698 = LINE ( 'NONE', #25821, #32895 ) ;
#21699 = CARTESIAN_POINT ( 'NONE',  ( -1.166969139818015755, 0.000000000000000000, 0.5905511811023582691 ) ) ;
#21700 = CARTESIAN_POINT ( 'NONE',  ( 1.091055626815042645, 3.346456692913386100, -0.3149606299212596716 ) ) ;
#21701 = EDGE_CURVE ( 'NONE', #15234, #18703, #9393, .T. ) ;
#21702 = CARTESIAN_POINT ( 'NONE',  ( -1.091055626815042645, 0.000000000000000000, -1.889763779527552146 ) ) ;
#21703 = EDGE_CURVE ( 'NONE', #29397, #32424, #42872, .T. ) ;
#21704 = CARTESIAN_POINT ( 'NONE',  ( 0.000000000000000000, 3.267716535433071279, -0.4724409448818886470 ) ) ;
#21705 = EDGE_CURVE ( 'NONE', #50730, #19354, #31523, .T. ) ;
#21706 = PLANE ( 'NONE',  #30001 ) ;
#21707 = EDGE_CURVE ( 'NONE', #34031, #12607, #50822, .T. ) ;
#21708 = VECTOR ( 'NONE', #47276, 39.37007874015748854 ) ;
#21709 = EDGE_LOOP ( 'NONE', ( #48048, #45891, #38793, #42193 ) ) ;
#21710 = CARTESIAN_POINT ( 'NONE',  ( 0.08119777152254364916, 1.623385212329073957, 0.000000000000000000 ) ) ;
#21711 = CARTESIAN_POINT ( 'NONE',  ( 0.000000000000000000, 6.692913385826772199, 0.000000000000000000 ) ) ;
#21712 = ORIENTED_EDGE ( 'NONE', *, *, #34639, .F. ) ;
#21713 = VECTOR ( 'NONE', #10884, 39.37007874015748143 ) ;
#21714 = ORIENTED_EDGE ( 'NONE', *, *, #37067, .T. ) ;
#21715 = VECTOR ( 'NONE', #22214, 39.37007874015748143 ) ;
#21716 = CARTESIAN_POINT ( 'NONE',  ( -1.363819533518803473, 3.267716535433071279, -0.7874015748031470974 ) ) ;
#21717 = ORIENTED_EDGE ( 'NONE', *, *, #6459, .T. ) ;
#21718 = ADVANCED_FACE ( 'NONE', ( #35396 ), #35144, .F. ) ;
#21719 = AXIS2_PLACEMENT_3D ( 'NONE', #18148, #37017, #25890 ) ;
#21720 = ORIENTED_EDGE ( 'NONE', *, *, #24693, .F. ) ;
#21721 = CARTESIAN_POINT ( 'NONE',  ( -0.8182917201112817063, 3.267716535433071279, 1.419509857074483046E-16 ) ) ;
#21722 = EDGE_CURVE ( 'NONE', #4354, #4010, #47479, .T. ) ;
#21723 = B_SPLINE_CURVE_WITH_KNOTS ( 'NONE', 3,
 ( #4343, #16995, #40230, #8727 ),
 .UNSPECIFIED., .F., .F.,
 ( 4, 4 ),
 ( 2.051448000182432276E-07, 0.002500220163013508554 ),
 .UNSPECIFIED. ) ;
#21724 = ORIENTED_EDGE ( 'NONE', *, *, #24485, .T. ) ;
#21725 = DIRECTION ( 'NONE',  ( 1.734723475976806848E-16, 0.000000000000000000, 1.000000000000000000 ) ) ;
#21726 = EDGE_CURVE ( 'NONE', #1147, #20835, #46967, .T. ) ;
#21727 = LINE ( 'NONE', #48281, #37944 ) ;
#21728 = EDGE_CURVE ( 'NONE', #9285, #17328, #31014, .T. ) ;
#21729 = ORIENTED_EDGE ( 'NONE', *, *, #16552, .F. ) ;
#21730 = ORIENTED_EDGE ( 'NONE', *, *, #19686, .F. ) ;
#21731 = DIRECTION ( 'NONE',  ( 1.000000000000000000, 0.000000000000000000, 0.000000000000000000 ) ) ;
#21733 = EDGE_LOOP ( 'NONE', ( #31243, #13930, #12430, #16469 ) ) ;
#21732 = ADVANCED_FACE ( 'NONE', ( #19376 ), #16024, .F. ) ;
#21734 = ORIENTED_EDGE ( 'NONE', *, *, #2102, .T. ) ;
#21735 = DIRECTION ( 'NONE',  ( -0.000000000000000000, 1.000000000000000000, -0.000000000000000000 ) ) ;
#21736 = DIRECTION ( 'NONE',  ( 0.000000000000000000, 0.000000000000000000, 1.000000000000000000 ) ) ;
#21737 = DIRECTION ( 'NONE',  ( 1.734723475976806848E-16, -0.000000000000000000, 1.000000000000000000 ) ) ;
#21738 = VERTEX_POINT ( 'NONE', #7769 ) ;
#21739 = LINE ( 'NONE', #14237, #8989 ) ;
#21740 = DIRECTION ( 'NONE',  ( 0.000000000000000000, -1.000000000000000000, 0.000000000000000000 ) ) ;
#21741 = DIRECTION ( 'NONE',  ( -0.000000000000000000, 1.000000000000000000, -0.000000000000000000 ) ) ;
#21742 = ORIENTED_EDGE ( 'NONE', *, *, #21701, .F. ) ;
#21743 = CARTESIAN_POINT ( 'NONE',  ( 2.558651102769570803E-16, 1.595182601976580683, -2.089297179032357121 ) ) ;
#21744 = VECTOR ( 'NONE', #23245, 39.37007874015748143 ) ;
#21745 = CARTESIAN_POINT ( 'NONE',  ( 0.000000000000000000, 3.267716535433071279, -0.9842519685039342603 ) ) ;
#21746 = DIRECTION ( 'NONE',  ( 0.3513748240813304724, -1.086859790425929286E-16, 0.9362348706397417564 ) ) ;
#21747 = ORIENTED_EDGE ( 'NONE', *, *, #42689, .F. ) ;
#21748 = VECTOR ( 'NONE', #38971, 39.37007874015748143 ) ;
#21749 = ORIENTED_EDGE ( 'NONE', *, *, #40909, .T. ) ;
#21750 = AXIS2_PLACEMENT_3D ( 'NONE', #43825, #32495, #48187 ) ;
#21751 = CIRCLE ( 'NONE', #39022, 2.066929133858268042 ) ;
#21752 = DIRECTION ( 'NONE',  ( 1.734723475976806848E-16, -0.000000000000000000, 1.000000000000000000 ) ) ;
#21753 = CARTESIAN_POINT ( 'NONE',  ( -0.6383587639822442261, 1.599252270110662399, -2.128056888689588089 ) ) ;
#21754 = LINE ( 'NONE', #45724, #46867 ) ;
#21755 = ORIENTED_EDGE ( 'NONE', *, *, #47608, .F. ) ;
#21756 = VERTEX_POINT ( 'NONE', #534 ) ;
#21757 = VECTOR ( 'NONE', #11655, 39.37007874015748143 ) ;
#21758 = CARTESIAN_POINT ( 'NONE',  ( -0.6383587639822442261, 1.599252270110662399, -2.128056888689588089 ) ) ;
#21759 = VERTEX_POINT ( 'NONE', #32042 ) ;
#21760 = DIRECTION ( 'NONE',  ( 1.000000000000000000, 0.000000000000000000, 0.000000000000000000 ) ) ;
#21761 = CARTESIAN_POINT ( 'NONE',  ( 2.160407304981128984, 5.118110236220475784, -0.1462862061266579361 ) ) ;
#21762 = ADVANCED_FACE ( 'NONE', ( #3901 ), #43119, .F. ) ;
#21763 = CARTESIAN_POINT ( 'NONE',  ( 0.1155636338427008941, -0.5222242541845523167, 0.000000000000000000 ) ) ;
#21764 = ADVANCED_FACE ( 'NONE', ( #47216 ), #47732, .F. ) ;
#21765 = CARTESIAN_POINT ( 'NONE',  ( -1.166969139818015977, 3.346456692913386100, -0.7874015748031470974 ) ) ;
#21766 = CARTESIAN_POINT ( 'NONE',  ( 1.636583440222563857, 3.346456692913386100, 0.4330708661417290162 ) ) ;
#21767 = VERTEX_POINT ( 'NONE', #12929 ) ;
#21768 = EDGE_CURVE ( 'NONE', #15363, #48074, #21184, .T. ) ;
#21769 = DIRECTION ( 'NONE',  ( -3.469446951953613696E-16, 0.000000000000000000, -1.000000000000000000 ) ) ;
#21770 = CARTESIAN_POINT ( 'NONE',  ( 1.636583440222563857, 3.346456692913386100, -1.161035397307311917E-15 ) ) ;
#21771 = PLANE ( 'NONE',  #30654 ) ;
#21772 = ORIENTED_EDGE ( 'NONE', *, *, #19181, .F. ) ;
#21773 = LINE ( 'NONE', #37276, #32295 ) ;
#21774 = DIRECTION ( 'NONE',  ( 1.000000000000000000, 0.000000000000000000, 0.000000000000000000 ) ) ;
#21775 = CARTESIAN_POINT ( 'NONE',  ( 1.686980615242215098, 5.905511811023623991, 1.408267424185160044 ) ) ;
#21776 = ORIENTED_EDGE ( 'NONE', *, *, #26005, .F. ) ;
#21777 = DIRECTION ( 'NONE',  ( -3.469446951953613696E-16, 0.000000000000000000, -1.000000000000000000 ) ) ;
#21778 = AXIS2_PLACEMENT_3D ( 'NONE', #49391, #10450, #29301 ) ;
#21779 = VECTOR ( 'NONE', #17817, 39.37007874015748143 ) ;
#21780 = ORIENTED_EDGE ( 'NONE', *, *, #24049, .F. ) ;
#21781 = VECTOR ( 'NONE', #40869, 39.37007874015748143 ) ;
#21782 = DIRECTION ( 'NONE',  ( 1.000000000000000000, -0.000000000000000000, 0.000000000000000000 ) ) ;
#21783 = FACE_OUTER_BOUND ( 'NONE', #23705, .T. ) ;
#21785 = VERTEX_POINT ( 'NONE', #36938 ) ;
#21784 = EDGE_CURVE ( 'NONE', #37182, #19985, #14371, .T. ) ;
#21786 = CARTESIAN_POINT ( 'NONE',  ( 1.909347346926324684, 3.346456692913386100, 0.2755905511810994302 ) ) ;
#21787 = AXIS2_PLACEMENT_3D ( 'NONE', #5793, #31611, #39357 ) ;
#21788 = CIRCLE ( 'NONE', #9401, 2.244934639244525076 ) ;
#21789 = DIRECTION ( 'NONE',  ( -0.000000000000000000, 0.000000000000000000, 1.000000000000000000 ) ) ;
#21790 = EDGE_CURVE ( 'NONE', #5106, #28960, #44148, .T. ) ;
#21791 = CARTESIAN_POINT ( 'NONE',  ( 0.7423782071083088185, 3.267716535433071279, -2.575641807848710687E-16 ) ) ;
#21792 = LINE ( 'NONE', #29272, #43325 ) ;
#21793 = PLANE ( 'NONE',  #14739 ) ;
#21794 = ORIENTED_EDGE ( 'NONE', *, *, #6288, .T. ) ;
#21795 = ORIENTED_EDGE ( 'NONE', *, *, #17693, .F. ) ;
#21796 = DIRECTION ( 'NONE',  ( -0.01601477604151182663, 0.9998717552508123996, -0.000000000000000000 ) ) ;
#21797 = VECTOR ( 'NONE', #11849, 39.37007874015748143 ) ;
#21798 = DIRECTION ( 'NONE',  ( -3.469446951953613696E-16, 0.000000000000000000, -1.000000000000000000 ) ) ;
#21799 = EDGE_CURVE ( 'NONE', #8220, #19533, #24247, .T. ) ;
#21800 = VERTEX_POINT ( 'NONE', #41317 ) ;
#21801 = LINE ( 'NONE', #18176, #30036 ) ;
#21802 = DIRECTION ( 'NONE',  ( -0.000000000000000000, 1.000000000000000000, -0.000000000000000000 ) ) ;
#21803 = DIRECTION ( 'NONE',  ( 1.000000000000000000, -0.000000000000000000, 0.000000000000000000 ) ) ;
#21804 = ORIENTED_EDGE ( 'NONE', *, *, #6838, .T. ) ;
#21805 = ORIENTED_EDGE ( 'NONE', *, *, #37346, .T. ) ;
#21806 = DIRECTION ( 'NONE',  ( -1.000000000000000000, 0.000000000000000000, 0.000000000000000000 ) ) ;
#21807 = CARTESIAN_POINT ( 'NONE',  ( -1.363819533518803473, 0.000000000000000000, -1.299212598425192544 ) ) ;
#21808 = CARTESIAN_POINT ( 'NONE',  ( -2.059449025298142999, 1.580632209844732960, -1.300463018946054428 ) ) ;
#21809 = ORIENTED_EDGE ( 'NONE', *, *, #5098, .T. ) ;
#21810 = DIRECTION ( 'NONE',  ( 1.734723475976806848E-16, -0.000000000000000000, 1.000000000000000000 ) ) ;
#21811 = PLANE ( 'NONE',  #12836 ) ;
#21812 = ORIENTED_EDGE ( 'NONE', *, *, #39965, .F. ) ;
#21813 = CARTESIAN_POINT ( 'NONE',  ( 2.106197740627111514, 3.346456692913386100, -1.299212598425194320 ) ) ;
#21814 = ORIENTED_EDGE ( 'NONE', *, *, #39366, .F. ) ;
#21815 = EDGE_LOOP ( 'NONE', ( #25614, #31630, #34928, #17050 ) ) ;
#21816 = CARTESIAN_POINT ( 'NONE',  ( 0.000000000000000000, 3.267716535433071279, -1.299212598425193210 ) ) ;
#21817 = FACE_OUTER_BOUND ( 'NONE', #18190, .T. ) ;
#21818 = ORIENTED_EDGE ( 'NONE', *, *, #30500, .F. ) ;
#21819 = CARTESIAN_POINT ( 'NONE',  ( 0.4788131938641113083, 0.000000000000000000, 2.914091152102192162 ) ) ;
#21820 = DIRECTION ( 'NONE',  ( 0.000000000000000000, -1.000000000000000000, 0.000000000000000000 ) ) ;
#21821 = ORIENTED_EDGE ( 'NONE', *, *, #19328, .T. ) ;
#21822 = AXIS2_PLACEMENT_3D ( 'NONE', #43691, #40357, #31586 ) ;
#21823 = VECTOR ( 'NONE', #17632, 39.37007874015748143 ) ;
#21824 = CIRCLE ( 'NONE', #6996, 1.850107469027523432 ) ;
#21825 = DIRECTION ( 'NONE',  ( -0.01601477604151182663, 0.9998717552508123996, -0.000000000000000000 ) ) ;
#21826 = CARTESIAN_POINT ( 'NONE',  ( -0.07591351300297340121, 0.000000000000000000, 2.165354330708650465 ) ) ;
#21827 = VECTOR ( 'NONE', #31682, 39.37007874015748143 ) ;
#21828 = VECTOR ( 'NONE', #49222, 39.37007874015748143 ) ;
#21829 = CARTESIAN_POINT ( 'NONE',  ( -0.2156685157583831947, 1.715903002249486997, -2.945280361644576850 ) ) ;
#21830 = EDGE_CURVE ( 'NONE', #9429, #35180, #20962, .T. ) ;
#21831 = CARTESIAN_POINT ( 'NONE',  ( 0.2727639067037602172, 0.000000000000000000, -2.047244094488182231 ) ) ;
#21832 = LINE ( 'NONE', #37588, #27000 ) ;
#21833 = VECTOR ( 'NONE', #30760, 39.37007874015748143 ) ;
#21834 = ORIENTED_EDGE ( 'NONE', *, *, #4105, .F. ) ;
#21835 = ADVANCED_FACE ( 'NONE', ( #44406 ), #40806, .F. ) ;
#21836 = CARTESIAN_POINT ( 'NONE',  ( 0.000000000000000000, 5.118110236220475784, 0.000000000000000000 ) ) ;
#21837 = EDGE_CURVE ( 'NONE', #49411, #38085, #13186, .T. ) ;
#21838 = DIRECTION ( 'NONE',  ( -0.000000000000000000, 1.000000000000000000, -0.000000000000000000 ) ) ;
#21839 = EDGE_CURVE ( 'NONE', #37269, #12892, #1299, .T. ) ;
#21840 = ORIENTED_EDGE ( 'NONE', *, *, #8722, .F. ) ;
#21841 = DIRECTION ( 'NONE',  ( -0.000000000000000000, 0.000000000000000000, 1.000000000000000000 ) ) ;
#21842 = CARTESIAN_POINT ( 'NONE',  ( 2.044241703397536636, 0.000000000000000000, -0.7159595814952622872 ) ) ;
#21843 = ORIENTED_EDGE ( 'NONE', *, *, #47181, .F. ) ;
#21844 = DIRECTION ( 'NONE',  ( -0.000000000000000000, 1.000000000000000000, -0.000000000000000000 ) ) ;
#21845 = EDGE_CURVE ( 'NONE', #5208, #31969, #46466, .T. ) ;
#21846 = DIRECTION ( 'NONE',  ( -0.000000000000000000, 1.000000000000000000, -0.000000000000000000 ) ) ;
#21847 = ORIENTED_EDGE ( 'NONE', *, *, #45306, .T. ) ;
#21848 = LINE ( 'NONE', #49420, #771 ) ;
#21849 = EDGE_LOOP ( 'NONE', ( #18351, #920, #44107, #39759 ) ) ;
#21850 = FACE_BOUND ( 'NONE', #13363, .T. ) ;
#21851 = CARTESIAN_POINT ( 'NONE',  ( 0.000000000000000000, 3.267716535433071279, 0.9055118110236164419 ) ) ;
#21852 = DIRECTION ( 'NONE',  ( 1.734723475976806848E-16, -0.000000000000000000, 1.000000000000000000 ) ) ;
#21853 = ADVANCED_FACE ( 'NONE', ( #20660 ), #13695, .F. ) ;
#21854 = EDGE_CURVE ( 'NONE', #37890, #5331, #34971, .T. ) ;
#21855 = DIRECTION ( 'NONE',  ( -0.000000000000000000, 1.000000000000000000, -0.000000000000000000 ) ) ;
#21856 = ORIENTED_EDGE ( 'NONE', *, *, #7152, .F. ) ;
#21857 = ORIENTED_EDGE ( 'NONE', *, *, #47230, .F. ) ;
#21858 = VECTOR ( 'NONE', #5437, 39.37007874015748143 ) ;
#21859 = FACE_OUTER_BOUND ( 'NONE', #31031, .T. ) ;
#21860 = ORIENTED_EDGE ( 'NONE', *, *, #36729, .F. ) ;
#21861 = EDGE_CURVE ( 'NONE', #45264, #14807, #1561, .T. ) ;
#21862 = VECTOR ( 'NONE', #4159, 39.37007874015748143 ) ;
#21863 = DIRECTION ( 'NONE',  ( 0.000000000000000000, 1.160734090543304660E-16, -1.000000000000000000 ) ) ;
#21864 = ORIENTED_EDGE ( 'NONE', *, *, #44999, .F. ) ;
#21865 = VECTOR ( 'NONE', #888, 39.37007874015748854 ) ;
#21866 = LINE ( 'NONE', #38128, #23137 ) ;
#21867 = ORIENTED_EDGE ( 'NONE', *, *, #23770, .T. ) ;
#21868 = DIRECTION ( 'NONE',  ( -0.9998717552508122886, -0.01601477604151185785, 0.000000000000000000 ) ) ;
#21869 = CARTESIAN_POINT ( 'NONE',  ( -1.688048600224982154, 0.000000000000000000, -0.4357642695449713277 ) ) ;
#21870 = VECTOR ( 'NONE', #28311, 39.37007874015748143 ) ;
#21871 = ORIENTED_EDGE ( 'NONE', *, *, #6109, .F. ) ;
#21872 = DIRECTION ( 'NONE',  ( 1.283101021437939896E-16, 1.000000000000000000, -1.154811821032073265E-17 ) ) ;
#21873 = ORIENTED_EDGE ( 'NONE', *, *, #48881, .F. ) ;
#21874 = ORIENTED_EDGE ( 'NONE', *, *, #28876, .F. ) ;
#21875 = ADVANCED_FACE ( 'NONE', ( #24798 ), #40549, .F. ) ;
#21876 = ORIENTED_EDGE ( 'NONE', *, *, #21324, .F. ) ;
#21877 = VERTEX_POINT ( 'NONE', #37451 ) ;
#21878 = CARTESIAN_POINT ( 'NONE',  ( 1.091055626815042645, 3.346456692913386100, -8.878505979408855953E-16 ) ) ;
#21879 = ORIENTED_EDGE ( 'NONE', *, *, #20957, .T. ) ;
#21880 = FACE_OUTER_BOUND ( 'NONE', #37082, .T. ) ;
#21881 = DIRECTION ( 'NONE',  ( 0.000000000000000000, -1.000000000000000000, 0.000000000000000000 ) ) ;
#21882 = CARTESIAN_POINT ( 'NONE',  ( -0.3465944589516567476, 5.905511811023623991, 2.185505870675810147 ) ) ;
#21883 = ORIENTED_EDGE ( 'NONE', *, *, #20695, .T. ) ;
#21884 = DIRECTION ( 'NONE',  ( -1.000000000000000000, 0.000000000000000000, 1.734723475976806848E-16 ) ) ;
#21885 = LINE ( 'NONE', #49210, #24630 ) ;
#21886 = VECTOR ( 'NONE', #12616, 39.37007874015748143 ) ;
#21887 = ORIENTED_EDGE ( 'NONE', *, *, #49744, .F. ) ;
#21888 = EDGE_CURVE ( 'NONE', #43399, #9369, #17315, .T. ) ;
#21889 = DIRECTION ( 'NONE',  ( 1.734723475976806848E-16, -0.000000000000000000, 1.000000000000000000 ) ) ;
#21890 = DIRECTION ( 'NONE',  ( 1.000000000000000000, 0.000000000000000000, 0.000000000000000000 ) ) ;
#21891 = VECTOR ( 'NONE', #3370, 39.37007874015748143 ) ;
#21892 = FACE_OUTER_BOUND ( 'NONE', #41983, .T. ) ;
#21893 = AXIS2_PLACEMENT_3D ( 'NONE', #1590, #13978, #25085 ) ;
#21894 = CARTESIAN_POINT ( 'NONE',  ( 2.889674983507178219, 1.665813060096536402, -0.6090712660037608250 ) ) ;
#21895 = EDGE_CURVE ( 'NONE', #4115, #32803, #32298, .T. ) ;
#21896 = ORIENTED_EDGE ( 'NONE', *, *, #30115, .F. ) ;
#21897 = FACE_OUTER_BOUND ( 'NONE', #29277, .T. ) ;
#21898 = EDGE_CURVE ( 'NONE', #38704, #970, #25305, .T. ) ;
#21899 = CARTESIAN_POINT ( 'NONE',  ( -1.662320194739478119, 6.692913385826772199, -1.388601395075575118 ) ) ;
#21900 = ORIENTED_EDGE ( 'NONE', *, *, #44797, .F. ) ;
#21901 = CARTESIAN_POINT ( 'NONE',  ( 0.000000000000000000, 2.755905511811024056, 0.000000000000000000 ) ) ;
#21902 = AXIS2_PLACEMENT_3D ( 'NONE', #15250, #18877, #35383 ) ;
#21903 = ADVANCED_FACE ( 'NONE', ( #1812 ), #12660, .F. ) ;
#21904 = DIRECTION ( 'NONE',  ( -1.000000000000000000, -0.000000000000000000, -0.000000000000000000 ) ) ;
#21905 = VECTOR ( 'NONE', #32204, 39.37007874015748143 ) ;
#21906 = ORIENTED_EDGE ( 'NONE', *, *, #29410, .F. ) ;
#21907 = CARTESIAN_POINT ( 'NONE',  ( 0.000000000000000000, 0.000000000000000000, 0.000000000000000000 ) ) ;
#21908 = ORIENTED_EDGE ( 'NONE', *, *, #14908, .T. ) ;
#21909 = CARTESIAN_POINT ( 'NONE',  ( 1.636583440222563857, 0.000000000000000000, 1.377952755905504256 ) ) ;
#21910 = CARTESIAN_POINT ( 'NONE',  ( -1.536664496436148184E-16, 3.346456692913386100, -0.5118110236220465570 ) ) ;
#21911 = CARTESIAN_POINT ( 'NONE',  ( 3.519654186525858491E-16, 0.000000000000000000, 2.874015748031496731 ) ) ;
#21912 = LINE ( 'NONE', #44872, #42406 ) ;
#21913 = EDGE_CURVE ( 'NONE', #35952, #31499, #37662, .T. ) ;
#21914 = CARTESIAN_POINT ( 'NONE',  ( 1.363819533518803695, 3.346456692913386100, 1.732283464566921172 ) ) ;
#21915 = VERTEX_POINT ( 'NONE', #2578 ) ;
#21916 = LINE ( 'NONE', #29910, #47155 ) ;
#21917 = VERTEX_POINT ( 'NONE', #10326 ) ;
#21918 = ORIENTED_EDGE ( 'NONE', *, *, #49695, .T. ) ;
#21919 = LINE ( 'NONE', #37678, #18821 ) ;
#21920 = VERTEX_POINT ( 'NONE', #14195 ) ;
#21921 = EDGE_CURVE ( 'NONE', #22090, #2321, #23650, .T. ) ;
#21922 = LINE ( 'NONE', #2295, #34533 ) ;
#21923 = DIRECTION ( 'NONE',  ( -0.000000000000000000, 1.000000000000000000, -0.000000000000000000 ) ) ;
#21924 = ORIENTED_EDGE ( 'NONE', *, *, #34992, .F. ) ;
#21925 = CARTESIAN_POINT ( 'NONE',  ( 1.287906020515830141, 3.267716535433071279, 0.1181102362204704270 ) ) ;
#21926 = EDGE_CURVE ( 'NONE', #50326, #19099, #30899, .T. ) ;
#21927 = CARTESIAN_POINT ( 'NONE',  ( 0.2727639067037602172, 3.267716535433071279, -2.047244094488182231 ) ) ;
#21928 = CARTESIAN_POINT ( 'NONE',  ( 1.363819533518803251, 0.000000000000000000, -0.9842519685039348154 ) ) ;
#21929 = VECTOR ( 'NONE', #42387, 39.37007874015748143 ) ;
#21930 = ORIENTED_EDGE ( 'NONE', *, *, #6795, .F. ) ;
#21931 = ORIENTED_EDGE ( 'NONE', *, *, #17246, .T. ) ;
#21932 = VECTOR ( 'NONE', #50169, 39.37007874015748143 ) ;
#21933 = LINE ( 'NONE', #3067, #17475 ) ;
#21934 = FACE_BOUND ( 'NONE', #1589, .T. ) ;
#21935 = ORIENTED_EDGE ( 'NONE', *, *, #18346, .T. ) ;
#21936 = EDGE_CURVE ( 'NONE', #45327, #5560, #10589, .T. ) ;
#21937 = VECTOR ( 'NONE', #43740, 39.37007874015748143 ) ;
#21938 = CARTESIAN_POINT ( 'NONE',  ( 0.000000000000000000, 3.267716535433071279, 0.7874015748031454320 ) ) ;
#21939 = DIRECTION ( 'NONE',  ( 1.734723475976806848E-16, -0.000000000000000000, 1.000000000000000000 ) ) ;
#21940 = VECTOR ( 'NONE', #25272, 39.37007874015748143 ) ;
#21941 = ORIENTED_EDGE ( 'NONE', *, *, #6739, .T. ) ;
#21942 = ORIENTED_EDGE ( 'NONE', *, *, #30505, .T. ) ;
#21943 = DIRECTION ( 'NONE',  ( 1.734723475976806848E-16, -0.000000000000000000, 1.000000000000000000 ) ) ;
#21944 = AXIS2_PLACEMENT_3D ( 'NONE', #39808, #16319, #572 ) ;
#21945 = CARTESIAN_POINT ( 'NONE',  ( 1.062992125984251413, 0.5905511811023621549, 1.062992125984251413 ) ) ;
#21946 = ADVANCED_FACE ( 'NONE', ( #50959 ), #7402, .F. ) ;
#21947 = ORIENTED_EDGE ( 'NONE', *, *, #23193, .F. ) ;
#21948 = ORIENTED_EDGE ( 'NONE', *, *, #15352, .T. ) ;
#21950 = ADVANCED_FACE ( 'NONE', ( #50700 ), #27261, .T. ) ;
#21949 = VERTEX_POINT ( 'NONE', #41823 ) ;
#21951 = DIRECTION ( 'NONE',  ( -3.469446951953613696E-16, 0.000000000000000000, -1.000000000000000000 ) ) ;
#21952 = FACE_OUTER_BOUND ( 'NONE', #39367, .T. ) ;
#21953 = DIRECTION ( 'NONE',  ( -3.986037398843765983E-20, -1.000000000000000000, -1.160734090543304660E-16 ) ) ;
#21954 = FACE_OUTER_BOUND ( 'NONE', #2938, .T. ) ;
#21955 = EDGE_LOOP ( 'NONE', ( #43206, #40976, #2554, #41669 ) ) ;
#21956 = ORIENTED_EDGE ( 'NONE', *, *, #30052, .F. ) ;
#21957 = CARTESIAN_POINT ( 'NONE',  ( 1.548545842648739956, 1.732704746525083772, 1.697655184951773810 ) ) ;
#21958 = CARTESIAN_POINT ( 'NONE',  ( 0.4696143004045479352, 3.346456692913386100, 0.1574803149606283648 ) ) ;
#21959 = DIRECTION ( 'NONE',  ( -0.000000000000000000, 1.000000000000000000, -0.000000000000000000 ) ) ;
#21960 = CARTESIAN_POINT ( 'NONE',  ( 1.287906020515829919, 3.249608194809333384, -2.086614173228340086 ) ) ;
#21961 = CARTESIAN_POINT ( 'NONE',  ( -0.8238130908517355966, 1.694707076513333410, 2.054984861273213337 ) ) ;
#21962 = EDGE_CURVE ( 'NONE', #40673, #12848, #43200, .T. ) ;
#21963 = CARTESIAN_POINT ( 'NONE',  ( 2.367016559580884305, 3.255337473942148119, 0.6299212598425161236 ) ) ;
#21964 = VECTOR ( 'NONE', #15839, 39.37007874015748143 ) ;
#21965 = EDGE_CURVE ( 'NONE', #36441, #38339, #33084, .T. ) ;
#21966 = PLANE ( 'NONE',  #38266 ) ;
#21967 = ORIENTED_EDGE ( 'NONE', *, *, #16836, .F. ) ;
#21968 = CIRCLE ( 'NONE', #39264, 2.165354330708661568 ) ;
#21969 = FACE_BOUND ( 'NONE', #11214, .T. ) ;
#21970 = DIRECTION ( 'NONE',  ( -0.01601477604151182663, 0.9998717552508123996, -0.000000000000000000 ) ) ;
#21971 = VECTOR ( 'NONE', #20016, 39.37007874015748143 ) ;
#21972 = ORIENTED_EDGE ( 'NONE', *, *, #31656, .F. ) ;
#21973 = VECTOR ( 'NONE', #43677, 39.37007874015748143 ) ;
#21974 = ORIENTED_EDGE ( 'NONE', *, *, #40436, .F. ) ;
#21975 = CARTESIAN_POINT ( 'NONE',  ( -1.152895553066196177, 0.000000000000000000, -1.833672301139088745 ) ) ;
#21976 = AXIS2_PLACEMENT_3D ( 'NONE', #36554, #36297, #921 ) ;
#21977 = ORIENTED_EDGE ( 'NONE', *, *, #44980, .F. ) ;
#21978 = VERTEX_POINT ( 'NONE', #2073 ) ;
#21979 = DIRECTION ( 'NONE',  ( 1.000000000000000000, -0.000000000000000000, 0.000000000000000000 ) ) ;
#21980 = EDGE_LOOP ( 'NONE', ( #9980, #26106, #40288, #32422 ) ) ;
#21981 = DIRECTION ( 'NONE',  ( -3.469446951953613696E-16, 0.000000000000000000, -1.000000000000000000 ) ) ;
#21982 = DIRECTION ( 'NONE',  ( 0.000000000000000000, 0.000000000000000000, -1.000000000000000000 ) ) ;
#21983 = EDGE_CURVE ( 'NONE', #41400, #37182, #48664, .T. ) ;
#21984 = ORIENTED_EDGE ( 'NONE', *, *, #34263, .F. ) ;
#21985 = ORIENTED_EDGE ( 'NONE', *, *, #20046, .T. ) ;
#21986 = LINE ( 'NONE', #33869, #46069 ) ;
#21987 = ORIENTED_EDGE ( 'NONE', *, *, #15524, .F. ) ;
#21988 = ORIENTED_EDGE ( 'NONE', *, *, #24280, .F. ) ;
#21989 = LINE ( 'NONE', #9604, #48704 ) ;
#21990 = CARTESIAN_POINT ( 'NONE',  ( -1.676283831994445306, 0.001070912127414903967, 0.4929124452910598198 ) ) ;
#21991 = DIRECTION ( 'NONE',  ( -0.000000000000000000, 1.000000000000000000, -0.000000000000000000 ) ) ;
#21992 = EDGE_CURVE ( 'NONE', #9482, #25262, #3812, .T. ) ;
#21993 = ORIENTED_EDGE ( 'NONE', *, *, #35590, .T. ) ;
#21994 = EDGE_CURVE ( 'NONE', #7323, #5416, #43002, .T. ) ;
#21995 = CARTESIAN_POINT ( 'NONE',  ( 1.909347346926324684, 3.346456692913386100, 0.2755905511810994302 ) ) ;
#21996 = CARTESIAN_POINT ( 'NONE',  ( 0.08139965876239094178, 1.610780518492231694, 0.000000000000000000 ) ) ;
#21997 = DIRECTION ( 'NONE',  ( 1.734723475976806848E-16, -0.000000000000000000, 1.000000000000000000 ) ) ;
#21998 = EDGE_CURVE ( 'NONE', #48458, #14599, #3636, .T. ) ;
#21999 = AXIS2_PLACEMENT_3D ( 'NONE', #3283, #19025, #35290 ) ;
#22000 = EDGE_LOOP ( 'NONE', ( #42374, #47758, #17795, #40398 ) ) ;
#22001 = CARTESIAN_POINT ( 'NONE',  ( -2.182111253630085290, 0.000000000000000000, -6.146657985744592735E-16 ) ) ;
#22002 = CARTESIAN_POINT ( 'NONE',  ( -2.592410190524168545, 1.678844659144130613, 1.413664012936335590 ) ) ;
#22003 = AXIS2_PLACEMENT_3D ( 'NONE', #25250, #30135, #33775 ) ;
#22004 = VECTOR ( 'NONE', #37843, 39.37007874015748143 ) ;
#22005 = CARTESIAN_POINT ( 'NONE',  ( -0.07591351300297277671, 0.000000000000000000, 1.732283464566921172 ) ) ;
#22006 = VERTEX_POINT ( 'NONE', #11773 ) ;
#22007 = ORIENTED_EDGE ( 'NONE', *, *, #11116, .T. ) ;
#22008 = LINE ( 'NONE', #22262, #27444 ) ;
#22009 = VECTOR ( 'NONE', #41123, 39.37007874015748143 ) ;
#22010 = PLANE ( 'NONE',  #24475 ) ;
#22011 = EDGE_CURVE ( 'NONE', #49275, #6745, #7902, .T. ) ;
#22012 = CARTESIAN_POINT ( 'NONE',  ( 0.7521025634872258170, 1.621523052975431867, 2.144027383376515328 ) ) ;
#22013 = ORIENTED_EDGE ( 'NONE', *, *, #32288, .T. ) ;
#22014 = ORIENTED_EDGE ( 'NONE', *, *, #41634, .F. ) ;
#22015 = VECTOR ( 'NONE', #45262, 39.37007874015748143 ) ;
#22016 = FACE_OUTER_BOUND ( 'NONE', #40072, .T. ) ;
#22017 = ORIENTED_EDGE ( 'NONE', *, *, #14908, .F. ) ;
#22018 = LINE ( 'NONE', #7022, #16741 ) ;
#22019 = DIRECTION ( 'NONE',  ( 1.734723475976806848E-16, -0.000000000000000000, 1.000000000000000000 ) ) ;
#22020 = EDGE_CURVE ( 'NONE', #26854, #11981, #29946, .T. ) ;
#22021 = ADVANCED_FACE ( 'NONE', ( #23388 ), #46855, .F. ) ;
#22022 = LINE ( 'NONE', #18902, #40694 ) ;
#22023 = LINE ( 'NONE', #28736, #40085 ) ;
#22024 = CARTESIAN_POINT ( 'NONE',  ( -0.3486774197067339376, 0.000000000000000000, -0.9448818897637762948 ) ) ;
#22025 = VERTEX_POINT ( 'NONE', #16942 ) ;
#22026 = EDGE_CURVE ( 'NONE', #9591, #8503, #40178, .T. ) ;
#22027 = LINE ( 'NONE', #33147, #28304 ) ;
#22028 = CARTESIAN_POINT ( 'NONE',  ( -1.636583440222564301, 3.346456692913386100, 1.574803149606291530 ) ) ;
#22029 = LINE ( 'NONE', #30781, #11705 ) ;
#22030 = ORIENTED_EDGE ( 'NONE', *, *, #1137, .F. ) ;
#22031 = DIRECTION ( 'NONE',  ( -0.000000000000000000, 0.000000000000000000, 1.000000000000000000 ) ) ;
#22032 = CARTESIAN_POINT ( 'NONE',  ( -0.7874015748031493178, 0.000000000000000000, -1.968503937007874072 ) ) ;
#22033 = CARTESIAN_POINT ( 'NONE',  ( -0.6214413264104945434, 0.000000000000000000, 0.1574803149606285035 ) ) ;
#22034 = ORIENTED_EDGE ( 'NONE', *, *, #16179, .T. ) ;
#22035 = AXIS2_PLACEMENT_3D ( 'NONE', #34477, #46562, #3990 ) ;
#22036 = CARTESIAN_POINT ( 'NONE',  ( -2.491402175429631605, 1.567214198537667302, -1.585592796919542025 ) ) ;
#22037 = VECTOR ( 'NONE', #20808, 39.37007874015748143 ) ;
#22038 = ORIENTED_EDGE ( 'NONE', *, *, #38588, .T. ) ;
#22039 = DIRECTION ( 'NONE',  ( 1.734723475976806848E-16, -0.000000000000000000, 1.000000000000000000 ) ) ;
#22040 = LINE ( 'NONE', #37286, #33230 ) ;
#22041 = ORIENTED_EDGE ( 'NONE', *, *, #46960, .T. ) ;
#22042 = LINE ( 'NONE', #2923, #14658 ) ;
#22043 = CARTESIAN_POINT ( 'NONE',  ( -1.891607981616729495, 1.579179190298960256, 1.073803248357834139 ) ) ;
#22044 = CARTESIAN_POINT ( 'NONE',  ( 0.2727639067037602172, 3.346456692913386100, -2.047244094488182231 ) ) ;
#22045 = DIRECTION ( 'NONE',  ( 0.000000000000000000, 0.000000000000000000, -1.000000000000000000 ) ) ;
#22046 = ORIENTED_EDGE ( 'NONE', *, *, #35567, .F. ) ;
#22047 = ORIENTED_EDGE ( 'NONE', *, *, #29656, .T. ) ;
#22048 = DIRECTION ( 'NONE',  ( 0.5508969814520945363, 0.000000000000000000, 0.8345732537213079727 ) ) ;
#22049 = CARTESIAN_POINT ( 'NONE',  ( 1.015142113812069313, 0.000000000000000000, 0.1574803149606286423 ) ) ;
#22050 = ORIENTED_EDGE ( 'NONE', *, *, #14029, .T. ) ;
#22051 = CARTESIAN_POINT ( 'NONE',  ( -0.8182917201112814842, 0.000000000000000000, 0.2755905511810998187 ) ) ;
#22052 = CARTESIAN_POINT ( 'NONE',  ( 0.000000000000000000, 3.267716535433071279, -1.456692913385822186 ) ) ;
#22053 = CARTESIAN_POINT ( 'NONE',  ( 1.909347346926324462, 3.267716535433071279, -0.7874015748031473194 ) ) ;
#22054 = VECTOR ( 'NONE', #39723, 39.37007874015748143 ) ;
#22055 = ORIENTED_EDGE ( 'NONE', *, *, #29269, .T. ) ;
#22056 = VERTEX_POINT ( 'NONE', #36558 ) ;
#22057 = EDGE_CURVE ( 'NONE', #33804, #19688, #14881, .T. ) ;
#22058 = DIRECTION ( 'NONE',  ( -0.01601477604151182663, 0.9998717552508123996, -0.000000000000000000 ) ) ;
#22059 = PLANE ( 'NONE',  #13452 ) ;
#22060 = LINE ( 'NONE', #46031, #20392 ) ;
#22061 = ADVANCED_FACE ( 'NONE', ( #36302 ), #929, .F. ) ;
#22062 = ORIENTED_EDGE ( 'NONE', *, *, #10895, .F. ) ;
#22063 = CARTESIAN_POINT ( 'NONE',  ( 1.686980615242215098, 6.692913385826772199, 1.408267424185160266 ) ) ;
#22064 = EDGE_CURVE ( 'NONE', #36994, #41352, #19768, .T. ) ;
#22065 = CARTESIAN_POINT ( 'NONE',  ( 1.091055626815042645, 3.267716535433071279, -1.892679809432644882E-16 ) ) ;
#22066 = ORIENTED_EDGE ( 'NONE', *, *, #6525, .F. ) ;
#22067 = DIRECTION ( 'NONE',  ( -0.000000000000000000, 1.000000000000000000, -0.000000000000000000 ) ) ;
#22068 = ORIENTED_EDGE ( 'NONE', *, *, #29050, .F. ) ;
#22069 = VERTEX_POINT ( 'NONE', #4286 ) ;
#22070 = CARTESIAN_POINT ( 'NONE',  ( 2.016369045219287948, 1.641772594434526278, 1.140940039539855677 ) ) ;
#22071 = DIRECTION ( 'NONE',  ( -0.04261736568783053986, 0.000000000000000000, -0.9990914673551313241 ) ) ;
#22072 = EDGE_CURVE ( 'NONE', #33123, #35300, #35531, .T. ) ;
#22073 = CARTESIAN_POINT ( 'NONE',  ( 1.091055626815042645, 3.346456692913386100, -0.9448818897637765168 ) ) ;
#22074 = VECTOR ( 'NONE', #25355, 39.37007874015748854 ) ;
#22075 = VECTOR ( 'NONE', #38484, 39.37007874015748143 ) ;
#22076 = VERTEX_POINT ( 'NONE', #24423 ) ;
#22077 = CARTESIAN_POINT ( 'NONE',  ( 0.7308738700548025324, 5.905511811023623991, 2.087463732006447525 ) ) ;
#22078 = LINE ( 'NONE', #10454, #35373 ) ;
#22079 = ORIENTED_EDGE ( 'NONE', *, *, #39152, .T. ) ;
#22080 = VECTOR ( 'NONE', #50752, 39.37007874015748143 ) ;
#22081 = EDGE_CURVE ( 'NONE', #3016, #16822, #28800, .T. ) ;
#22082 = ORIENTED_EDGE ( 'NONE', *, *, #45349, .F. ) ;
#22083 = DIRECTION ( 'NONE',  ( -3.469446951953613696E-16, 0.000000000000000000, -1.000000000000000000 ) ) ;
#22084 = CARTESIAN_POINT ( 'NONE',  ( 2.100227814008711391, 1.467797480264206866, -2.076109931251913565 ) ) ;
#22085 = EDGE_CURVE ( 'NONE', #18042, #23291, #31515, .T. ) ;
#22086 = CARTESIAN_POINT ( 'NONE',  ( 0.5786196242795136335, 3.346456692913386100, -2.086614173228340086 ) ) ;
#22087 = EDGE_CURVE ( 'NONE', #22241, #33634, #16162, .T. ) ;
#22088 = LINE ( 'NONE', #2210, #50028 ) ;
#22089 = CARTESIAN_POINT ( 'NONE',  ( 1.363819533518803695, 0.000000000000000000, 1.732283464566921172 ) ) ;
#22090 = VERTEX_POINT ( 'NONE', #48129 ) ;
#22091 = LINE ( 'NONE', #33724, #6012 ) ;
#22092 = EDGE_CURVE ( 'NONE', #40703, #16654, #43766, .T. ) ;
#22093 = VECTOR ( 'NONE', #31349, 39.37007874015748854 ) ;
#22094 = ADVANCED_FACE ( 'NONE', ( #40437 ), #44290, .F. ) ;
#22095 = DIRECTION ( 'NONE',  ( 1.734723475976806848E-16, 0.000000000000000000, 1.000000000000000000 ) ) ;
#22096 = ORIENTED_EDGE ( 'NONE', *, *, #4929, .F. ) ;
#22097 = CARTESIAN_POINT ( 'NONE',  ( -1.091055626815042423, 3.267716535433071279, 1.892679809432644143E-16 ) ) ;
#22098 = CARTESIAN_POINT ( 'NONE',  ( -0.3499974520433976055, 1.636679305949812147, 2.204257908207249095 ) ) ;
#22099 = ORIENTED_EDGE ( 'NONE', *, *, #5327, .T. ) ;
#22100 = CARTESIAN_POINT ( 'NONE',  ( 0.000000000000000000, 3.267716535433071279, -1.614173228346451605 ) ) ;
#22101 = DIRECTION ( 'NONE',  ( -0.000000000000000000, 0.000000000000000000, 1.000000000000000000 ) ) ;
#22102 = CARTESIAN_POINT ( 'NONE',  ( -2.084291548511495229, 6.692913385826772199, 0.6254821886024592992 ) ) ;
#22103 = ORIENTED_EDGE ( 'NONE', *, *, #40679, .F. ) ;
#22104 = DIRECTION ( 'NONE',  ( 1.000000000000000000, 0.000000000000000000, 0.000000000000000000 ) ) ;
#22105 = ORIENTED_EDGE ( 'NONE', *, *, #4605, .F. ) ;
#22106 = FACE_BOUND ( 'NONE', #1985, .T. ) ;
#22107 = LINE ( 'NONE', #21593, #29214 ) ;
#22108 = CARTESIAN_POINT ( 'NONE',  ( -0.5455278134075214336, 3.346456692913386100, -0.6299212598425175669 ) ) ;
#22109 = PLANE ( 'NONE',  #16105 ) ;
#22110 = CIRCLE ( 'NONE', #49257, 2.244934639244525076 ) ;
#22111 = AXIS2_PLACEMENT_3D ( 'NONE', #20626, #1005, #16764 ) ;
#22112 = ORIENTED_EDGE ( 'NONE', *, *, #32225, .T. ) ;
#22113 = VERTEX_POINT ( 'NONE', #39913 ) ;
#22114 = DIRECTION ( 'NONE',  ( -1.000000000000000000, 0.000000000000000000, 0.000000000000000000 ) ) ;
#22115 = AXIS2_PLACEMENT_3D ( 'NONE', #4470, #12986, #597 ) ;
#22116 = DIRECTION ( 'NONE',  ( 0.000000000000000000, 1.000000000000000000, 0.000000000000000000 ) ) ;
#22117 = VERTEX_POINT ( 'NONE', #44027 ) ;
#22118 = CARTESIAN_POINT ( 'NONE',  ( 0.000000000000000000, 10.31496062992126284, -0.3937007874015748254 ) ) ;
#22119 = VECTOR ( 'NONE', #25333, 39.37007874015748143 ) ;
#22120 = ORIENTED_EDGE ( 'NONE', *, *, #41023, .F. ) ;
#22121 = CARTESIAN_POINT ( 'NONE',  ( -1.363819533518803473, 0.000000000000000000, 1.732283464566920950 ) ) ;
#22122 = AXIS2_PLACEMENT_3D ( 'NONE', #6952, #39199, #43056 ) ;
#22123 = B_SPLINE_CURVE_WITH_KNOTS ( 'NONE', 3,
 ( #13970, #48523, #12953, #1323 ),
 .UNSPECIFIED., .F., .F.,
 ( 4, 4 ),
 ( 0.02786225668000808300, 0.02887988550437843929 ),
 .UNSPECIFIED. ) ;
#22124 = LINE ( 'NONE', #18243, #14921 ) ;
#22125 = EDGE_CURVE ( 'NONE', #48282, #1443, #5057, .T. ) ;
#22126 = ORIENTED_EDGE ( 'NONE', *, *, #20955, .F. ) ;
#22127 = ADVANCED_FACE ( 'NONE', ( #4547 ), #20805, .F. ) ;
#22128 = CARTESIAN_POINT ( 'NONE',  ( -0.3486774197067343262, 0.000000000000000000, -2.401574803149598036 ) ) ;
#22129 = ORIENTED_EDGE ( 'NONE', *, *, #46607, .T. ) ;
#22130 = ORIENTED_EDGE ( 'NONE', *, *, #36870, .F. ) ;
#22131 = CONICAL_SURFACE ( 'NONE', #8927, 2.246510896728926010, 0.01601546068027819014 ) ;
#22132 = EDGE_CURVE ( 'NONE', #1749, #10246, #20284, .T. ) ;
#22133 = ORIENTED_EDGE ( 'NONE', *, *, #48624, .F. ) ;
#22134 = ORIENTED_EDGE ( 'NONE', *, *, #12292, .T. ) ;
#22135 = LINE ( 'NONE', #44840, #32705 ) ;
#22136 = ORIENTED_EDGE ( 'NONE', *, *, #494, .F. ) ;
#22137 = LINE ( 'NONE', #41496, #28734 ) ;
#22138 = DIRECTION ( 'NONE',  ( -0.01601477604151182663, 0.9998717552508123996, -0.000000000000000000 ) ) ;
#22139 = ADVANCED_FACE ( 'NONE', ( #20017 ), #8575, .T. ) ;
#22140 = AXIS2_PLACEMENT_3D ( 'NONE', #45127, #26039, #33291 ) ;
#22141 = LINE ( 'NONE', #9500, #33843 ) ;
#22142 = DIRECTION ( 'NONE',  ( -0.9998717552508121775, -0.01601477604151182316, 0.000000000000000000 ) ) ;
#22143 = PLANE ( 'NONE',  #20380 ) ;
#22144 = ORIENTED_EDGE ( 'NONE', *, *, #50183, .T. ) ;
#22145 = EDGE_CURVE ( 'NONE', #43925, #39410, #35785, .T. ) ;
#22146 = CARTESIAN_POINT ( 'NONE',  ( 0.2727639067037602172, 3.346456692913386100, -2.088563196121306476 ) ) ;
#22147 = LINE ( 'NONE', #30397, #45597 ) ;
#22148 = EDGE_CURVE ( 'NONE', #28307, #22970, #21002, .T. ) ;
#22149 = VECTOR ( 'NONE', #8596, 39.37007874015748143 ) ;
#22150 = CARTESIAN_POINT ( 'NONE',  ( -2.793030215715272213, 1.573188339825353665, 0.9592557174602283077 ) ) ;
#22151 = DIRECTION ( 'NONE',  ( 1.000000000000000000, 0.000000000000000000, 0.000000000000000000 ) ) ;
#22152 = VECTOR ( 'NONE', #4019, 39.37007874015748143 ) ;
#22153 = VECTOR ( 'NONE', #12636, 39.37007874015748143 ) ;
#22154 = ORIENTED_EDGE ( 'NONE', *, *, #8323, .T. ) ;
#22155 = FACE_OUTER_BOUND ( 'NONE', #2536, .T. ) ;
#22156 = DIRECTION ( 'NONE',  ( 0.000000000000000000, 1.000000000000000000, 0.000000000000000000 ) ) ;
#22157 = EDGE_LOOP ( 'NONE', ( #30303, #18241, #4540, #33602 ) ) ;
#22158 = CARTESIAN_POINT ( 'NONE',  ( -1.091055626815042645, 3.346456692913386100, 1.870389530743259199 ) ) ;
#22159 = CARTESIAN_POINT ( 'NONE',  ( 0.5455278134075211005, 0.000000000000000000, -0.8267716535433055070 ) ) ;
#22160 = VECTOR ( 'NONE', #34520, 39.37007874015748143 ) ;
#22161 = ORIENTED_EDGE ( 'NONE', *, *, #29311, .T. ) ;
#22162 = VECTOR ( 'NONE', #41270, 39.37007874015748143 ) ;
#22163 = VERTEX_POINT ( 'NONE', #673 ) ;
#22164 = DIRECTION ( 'NONE',  ( -0.2000875118326022883, -0.000000000000000000, 0.9797780297642105785 ) ) ;
#22165 = LINE ( 'NONE', #22667, #46469 ) ;
#22166 = CARTESIAN_POINT ( 'NONE',  ( 0.7423782071083087075, 3.346456692913386100, -0.6299212598425181220 ) ) ;
#22167 = VECTOR ( 'NONE', #50209, 39.37007874015748143 ) ;
#22168 = CARTESIAN_POINT ( 'NONE',  ( -0.5455278134075208785, 0.000000000000000000, 0.7480314960629874665 ) ) ;
#22169 = FACE_OUTER_BOUND ( 'NONE', #31129, .T. ) ;
#22170 = ORIENTED_EDGE ( 'NONE', *, *, #45530, .F. ) ;
#22171 = DIRECTION ( 'NONE',  ( 0.01601477604151182663, -0.9998717552508123996, 0.000000000000000000 ) ) ;
#22172 = ORIENTED_EDGE ( 'NONE', *, *, #48344, .T. ) ;
#22173 = VERTEX_POINT ( 'NONE', #48634 ) ;
#22174 = DIRECTION ( 'NONE',  ( -1.000000000000000000, 0.000000000000000000, -0.000000000000000000 ) ) ;
#22175 = VERTEX_POINT ( 'NONE', #45540 ) ;
#22176 = DIRECTION ( 'NONE',  ( 0.000000000000000000, 1.000000000000000000, 0.000000000000000000 ) ) ;
#22177 = DIRECTION ( 'NONE',  ( 1.000000000000000000, 0.000000000000000000, 0.000000000000000000 ) ) ;
#22178 = ORIENTED_EDGE ( 'NONE', *, *, #29233, .F. ) ;
#22179 = FACE_OUTER_BOUND ( 'NONE', #40677, .T. ) ;
#22180 = AXIS2_PLACEMENT_3D ( 'NONE', #9669, #25405, #5791 ) ;
#22181 = CARTESIAN_POINT ( 'NONE',  ( -0.8182917201112819283, 3.346456692913386100, 0.1574803149606285035 ) ) ;
#22182 = LINE ( 'NONE', #10559, #31307 ) ;
#22183 = VERTEX_POINT ( 'NONE', #40684 ) ;
#22185 = EDGE_LOOP ( 'NONE', ( #38566, #14760, #44317, #15682 ) ) ;
#22184 = EDGE_CURVE ( 'NONE', #15712, #14697, #40941, .T. ) ;
#22186 = DIRECTION ( 'NONE',  ( 1.000000000000000000, -0.000000000000000000, 0.000000000000000000 ) ) ;
#22187 = FACE_BOUND ( 'NONE', #26188, .T. ) ;
#22188 = EDGE_LOOP ( 'NONE', ( #31856, #45679, #49946, #48604 ) ) ;
#22189 = EDGE_CURVE ( 'NONE', #15045, #31017, #1177, .T. ) ;
#22190 = AXIS2_PLACEMENT_3D ( 'NONE', #49875, #49378, #33183 ) ;
#22191 = VECTOR ( 'NONE', #18710, 39.37007874015748143 ) ;
#22192 = FACE_OUTER_BOUND ( 'NONE', #28077, .T. ) ;
#22193 = LINE ( 'NONE', #6695, #49733 ) ;
#22194 = ADVANCED_FACE ( 'NONE', ( #41445 ), #17442, .F. ) ;
#22196 = ORIENTED_EDGE ( 'NONE', *, *, #39554, .F. ) ;
#22195 = EDGE_CURVE ( 'NONE', #33217, #48211, #36814, .T. ) ;
#22197 = ORIENTED_EDGE ( 'NONE', *, *, #30753, .T. ) ;
#22198 = VECTOR ( 'NONE', #18082, 39.37007874015748143 ) ;
#22199 = DIRECTION ( 'NONE',  ( -0.9998717552508121775, -0.01601477604151182663, 0.000000000000000000 ) ) ;
#22200 = LINE ( 'NONE', #46162, #43510 ) ;
#22201 = ORIENTED_EDGE ( 'NONE', *, *, #38742, .T. ) ;
#22202 = ORIENTED_EDGE ( 'NONE', *, *, #32000, .F. ) ;
#22203 = VECTOR ( 'NONE', #29000, 39.37007874015748143 ) ;
#22204 = VERTEX_POINT ( 'NONE', #2465 ) ;
#22205 = CARTESIAN_POINT ( 'NONE',  ( 0.2727639067037604392, 0.000000000000000000, -1.614173228346451605 ) ) ;
#22206 = DIRECTION ( 'NONE',  ( -0.000000000000000000, 1.000000000000000000, -0.000000000000000000 ) ) ;
#22207 = ADVANCED_FACE ( 'NONE', ( #9699 ), #22587, .T. ) ;
#22208 = DIRECTION ( 'NONE',  ( -0.000000000000000000, 1.000000000000000000, -0.000000000000000000 ) ) ;
#22209 = CARTESIAN_POINT ( 'NONE',  ( 0.1155636338427008941, -0.5222242541845523167, 0.000000000000000000 ) ) ;
#22210 = ORIENTED_EDGE ( 'NONE', *, *, #23574, .F. ) ;
#22211 = VERTEX_POINT ( 'NONE', #22084 ) ;
#22212 = DIRECTION ( 'NONE',  ( 1.000000000000000000, 0.000000000000000000, 0.000000000000000000 ) ) ;
#22213 = CARTESIAN_POINT ( 'NONE',  ( 1.232620761116212105, 1.574803149606302854, -1.780282403660734980 ) ) ;
#22214 = DIRECTION ( 'NONE',  ( -0.000000000000000000, 1.000000000000000000, -0.000000000000000000 ) ) ;
#22215 = EDGE_CURVE ( 'NONE', #15891, #33992, #1437, .T. ) ;
#22216 = DIRECTION ( 'NONE',  ( -0.000000000000000000, -1.000000000000000000, -0.000000000000000000 ) ) ;
#22217 = LINE ( 'NONE', #34090, #38037 ) ;
#22218 = CARTESIAN_POINT ( 'NONE',  ( 2.017116292511733189, 3.346456692913386100, -0.7874015748031473194 ) ) ;
#22219 =( BOUNDED_CURVE ( )  B_SPLINE_CURVE ( 3, ( #4467, #594, #29230, #45461 ),
 .UNSPECIFIED., .F., .F. ) 
 B_SPLINE_CURVE_WITH_KNOTS ( ( 4, 4 ),
 ( 6.010276100315349979, 6.061027312936714040 ),
 .UNSPECIFIED. ) 
 CURVE ( )  GEOMETRIC_REPRESENTATION_ITEM ( )  RATIONAL_B_SPLINE_CURVE ( ( 1.000000000000000000, 0.9997853710521733550, 0.9997853710521733550, 1.000000000000000000 ) ) 
 REPRESENTATION_ITEM ( '' )  );
#22220 = CONICAL_SURFACE ( 'NONE', #21368, 3.033577403570480779, 1.554780866114618743 ) ;
#22221 = EDGE_CURVE ( 'NONE', #24926, #6017, #46203, .T. ) ;
#22222 = CARTESIAN_POINT ( 'NONE',  ( -0.6214413264104939882, 3.267716535433071279, 1.102362204724404160 ) ) ;
#22223 = ORIENTED_EDGE ( 'NONE', *, *, #49898, .F. ) ;
#22224 = DIRECTION ( 'NONE',  ( -1.000000000000000000, 0.000000000000000000, -0.000000000000000000 ) ) ;
#22225 = DIRECTION ( 'NONE',  ( 1.000000000000000000, 0.000000000000000000, -3.469446951953613696E-16 ) ) ;
#22226 = ORIENTED_EDGE ( 'NONE', *, *, #49522, .F. ) ;
#22227 = EDGE_CURVE ( 'NONE', #21491, #28109, #5568, .T. ) ;
#22228 = ORIENTED_EDGE ( 'NONE', *, *, #39366, .T. ) ;
#22229 = VECTOR ( 'NONE', #1043, 39.37007874015748143 ) ;
#22230 = DIRECTION ( 'NONE',  ( 1.000000000000000000, 0.000000000000000000, 0.000000000000000000 ) ) ;
#22231 = ORIENTED_EDGE ( 'NONE', *, *, #34584, .T. ) ;
#22232 = VECTOR ( 'NONE', #41401, 39.37007874015748143 ) ;
#22233 = ORIENTED_EDGE ( 'NONE', *, *, #24518, .F. ) ;
#22234 = LINE ( 'NONE', #26594, #8099 ) ;
#22235 = ORIENTED_EDGE ( 'NONE', *, *, #26380, .T. ) ;
#22236 = LINE ( 'NONE', #22737, #5417 ) ;
#22237 = CARTESIAN_POINT ( 'NONE',  ( 0.07982360342473591996, 1.709180471932028711, 0.000000000000000000 ) ) ;
#22238 = ORIENTED_EDGE ( 'NONE', *, *, #5101, .F. ) ;
#22239 = ORIENTED_EDGE ( 'NONE', *, *, #30531, .F. ) ;
#22240 = DIRECTION ( 'NONE',  ( -0.000000000000000000, 1.000000000000000000, -0.000000000000000000 ) ) ;
#22241 = VERTEX_POINT ( 'NONE', #25693 ) ;
#22242 = VERTEX_POINT ( 'NONE', #29314 ) ;
#22243 = CARTESIAN_POINT ( 'NONE',  ( 1.287906020515830141, 0.000000000000000000, 0.3149606299212578953 ) ) ;
#22244 = PLANE ( 'NONE',  #9508 ) ;
#22245 = CARTESIAN_POINT ( 'NONE',  ( -1.364345965745727973, 1.205361022782829114E-17, 1.150974876880269893 ) ) ;
#22246 = CARTESIAN_POINT ( 'NONE',  ( 1.930190994932110771, 6.692913385826772199, -0.9827944786818446632 ) ) ;
#22247 = EDGE_CURVE ( 'NONE', #45160, #36136, #39469, .T. ) ;
#22248 = ORIENTED_EDGE ( 'NONE', *, *, #42636, .T. ) ;
#22249 = CARTESIAN_POINT ( 'NONE',  ( -0.8942052331142552601, 3.346456692913386100, -2.086614173228339641 ) ) ;
#22250 = CARTESIAN_POINT ( 'NONE',  ( -1.091055626815042201, 0.000000000000000000, 0.4330708661417290162 ) ) ;
#22251 = VECTOR ( 'NONE', #772, 39.37007874015748143 ) ;
#22252 = DIRECTION ( 'NONE',  ( 5.063291518729136385E-17, 1.000000000000000000, -1.184615939703115601E-16 ) ) ;
#22253 = EDGE_CURVE ( 'NONE', #25178, #33862, #37330, .T. ) ;
#22254 = EDGE_LOOP ( 'NONE', ( #21204, #39599, #19543, #9160, #15579, #45719, #35769, #25592, #10727, #10937, #13453, #19041, #8036, #2568, #50994, #38810, #46494, #32035, #10362, #13798, #20999, #3840, #30550 ) ) ;
#22255 = DIRECTION ( 'NONE',  ( 0.9639628606958549062, 0.000000000000000000, -0.2660368455666687892 ) ) ;
#22256 = DIRECTION ( 'NONE',  ( 0.000000000000000000, -1.000000000000000000, 0.000000000000000000 ) ) ;
#22257 = CARTESIAN_POINT ( 'NONE',  ( 1.025452293874513421, 0.4349011127721513215, -1.051609096396380671 ) ) ;
#22258 = ORIENTED_EDGE ( 'NONE', *, *, #17789, .T. ) ;
#22259 = ORIENTED_EDGE ( 'NONE', *, *, #36722, .F. ) ;
#22260 = DIRECTION ( 'NONE',  ( 0.3743958918047329831, 0.9208323613108516659, -0.1090663952022807720 ) ) ;
#22261 = AXIS2_PLACEMENT_3D ( 'NONE', #33772, #25494, #18008 ) ;
#22262 = CARTESIAN_POINT ( 'NONE',  ( 0.7423782071083087075, 3.346456692913386100, 0.3149606299212576177 ) ) ;
#22263 = CARTESIAN_POINT ( 'NONE',  ( 1.642191404871903071, 0.000000000000000000, 0.5853255206279913692 ) ) ;
#22264 = CARTESIAN_POINT ( 'NONE',  ( 1.091055626815042645, 3.346456692913386100, -0.9448818897637765168 ) ) ;
#22265 = ORIENTED_EDGE ( 'NONE', *, *, #24140, .T. ) ;
#22266 = ORIENTED_EDGE ( 'NONE', *, *, #47984, .T. ) ;
#22267 = DIRECTION ( 'NONE',  ( -1.000000000000000000, 0.000000000000000000, 0.000000000000000000 ) ) ;
#22268 = CARTESIAN_POINT ( 'NONE',  ( 1.091055626815042645, 3.346456692913386100, 0.1181102362204704270 ) ) ;
#22269 = VECTOR ( 'NONE', #41597, 39.37007874015748143 ) ;
#22270 = ORIENTED_EDGE ( 'NONE', *, *, #2500, .T. ) ;
#22271 = CARTESIAN_POINT ( 'NONE',  ( 0.000000000000000000, 3.267716535433071279, -1.299212598425193210 ) ) ;
#22272 = DIRECTION ( 'NONE',  ( 1.000000000000000000, 0.000000000000000000, 0.000000000000000000 ) ) ;
#22273 = ADVANCED_FACE ( 'NONE', ( #14075 ), #24932, .F. ) ;
#22274 = CARTESIAN_POINT ( 'NONE',  ( -0.2824664041639280421, 0.01564075248451678515, 1.832131162653048095 ) ) ;
#22275 = PLANE ( 'NONE',  #39259 ) ;
#22276 = PLANE ( 'NONE',  #19625 ) ;
#22277 = ORIENTED_EDGE ( 'NONE', *, *, #18231, .F. ) ;
#22278 = LINE ( 'NONE', #38780, #25881 ) ;
#22279 =( LENGTH_UNIT ( ) NAMED_UNIT ( * ) SI_UNIT ( $, .METRE. ) );
#22280 = CARTESIAN_POINT ( 'NONE',  ( 0.2727639067037604947, 3.346456692913386100, 0.7874015748031454320 ) ) ;
#22281 = EDGE_CURVE ( 'NONE', #183, #30123, #45042, .T. ) ;
#22282 = ORIENTED_EDGE ( 'NONE', *, *, #49775, .T. ) ;
#22283 = DIRECTION ( 'NONE',  ( -0.000000000000000000, 1.000000000000000000, -0.000000000000000000 ) ) ;
#22284 = EDGE_CURVE ( 'NONE', #41046, #23218, #5819, .T. ) ;
#22285 = CARTESIAN_POINT ( 'NONE',  ( -0.6735344408194913202, 1.606463534062856580, -2.625481381298739425 ) ) ;
#22286 = DIRECTION ( 'NONE',  ( -1.000000000000000000, -0.000000000000000000, -0.000000000000000000 ) ) ;
#22288 = EDGE_CURVE ( 'NONE', #50330, #27595, #33463, .T. ) ;
#22287 = ORIENTED_EDGE ( 'NONE', *, *, #1666, .F. ) ;
#22289 = CARTESIAN_POINT ( 'NONE',  ( -2.473332397914018710, 1.566147966415063486, -1.612967339752349183 ) ) ;
#22290 = ADVANCED_FACE ( 'NONE', ( #13827 ), #25952, .F. ) ;
#22291 = ORIENTED_EDGE ( 'NONE', *, *, #25800, .F. ) ;
#22292 = LINE ( 'NONE', #42655, #31284 ) ;
#22293 = VERTEX_POINT ( 'NONE', #37844 ) ;
#22294 = CARTESIAN_POINT ( 'NONE',  ( 0.1155636338427008941, -0.5222242541845523167, 0.000000000000000000 ) ) ;
#22295 = EDGE_CURVE ( 'NONE', #12211, #42980, #23087, .T. ) ;
#22296 = AXIS2_PLACEMENT_3D ( 'NONE', #39147, #47872, #50961 ) ;
#22297 = CARTESIAN_POINT ( 'NONE',  ( -0.3486774197067342151, 3.267716535433071279, -2.204724409448810540 ) ) ;
#22298 = CYLINDRICAL_SURFACE ( 'NONE', #9067, 1.181102362204723200 ) ;
#22299 = DIRECTION ( 'NONE',  ( -0.01601477604151182663, 0.9998717552508123996, -0.000000000000000000 ) ) ;
#22300 = VECTOR ( 'NONE', #2635, 39.37007874015748143 ) ;
#22301 = ORIENTED_EDGE ( 'NONE', *, *, #47137, .T. ) ;
#22302 = EDGE_LOOP ( 'NONE', ( #43096, #38135, #14724, #22355, #16218, #13845, #43181, #42361, #25751, #15054, #5508, #9236, #38685 ) ) ;
#22303 = DIRECTION ( 'NONE',  ( 0.9639628606958550172, -1.160734090543304660E-16, -0.2660368455666688448 ) ) ;
#22304 = LINE ( 'NONE', #37553, #20550 ) ;
#22305 = VERTEX_POINT ( 'NONE', #50898 ) ;
#22306 = DIRECTION ( 'NONE',  ( -3.986037398843765983E-20, -1.000000000000000000, -1.160734090543304660E-16 ) ) ;
#22307 = DIRECTION ( 'NONE',  ( 3.586865599282426309E-17, -1.000000000000000000, -1.103923720497134591E-16 ) ) ;
#22308 = VECTOR ( 'NONE', #5913, 39.37007874015748854 ) ;
#22309 = FACE_OUTER_BOUND ( 'NONE', #35052, .T. ) ;
#22310 = EDGE_CURVE ( 'NONE', #3065, #50816, #35216, .T. ) ;
#22311 = ORIENTED_EDGE ( 'NONE', *, *, #34231, .T. ) ;
#22312 = VERTEX_POINT ( 'NONE', #22839 ) ;
#22313 = FACE_OUTER_BOUND ( 'NONE', #37393, .T. ) ;
#22314 = LINE ( 'NONE', #34692, #2726 ) ;
#22315 = PLANE ( 'NONE',  #37108 ) ;
#22316 = EDGE_CURVE ( 'NONE', #27306, #44282, #7350, .T. ) ;
#22317 = ORIENTED_EDGE ( 'NONE', *, *, #19445, .F. ) ;
#22318 = B_SPLINE_CURVE_WITH_KNOTS ( 'NONE', 3,
 ( #10496, #41737, #6370, #30116 ),
 .UNSPECIFIED., .F., .F.,
 ( 4, 4 ),
 ( 2.329854378366125777E-07, 0.01910013319552298500 ),
 .UNSPECIFIED. ) ;
#22319 = CARTESIAN_POINT ( 'NONE',  ( 1.091055626815043311, 3.346456692913386100, 1.377952755905504256 ) ) ;
#22320 = FACE_BOUND ( 'NONE', #9904, .T. ) ;
#22321 = ORIENTED_EDGE ( 'NONE', *, *, #38667, .T. ) ;
#22322 = EDGE_CURVE ( 'NONE', #12349, #3787, #39085, .T. ) ;
#22323 = DIRECTION ( 'NONE',  ( 7.097135778201508621E-17, 1.000000000000000000, 1.075170113095020677E-16 ) ) ;
#22324 = EDGE_LOOP ( 'NONE', ( #50639, #44191, #34117, #86 ) ) ;
#22325 = VERTEX_POINT ( 'NONE', #42701 ) ;
#22326 = DIRECTION ( 'NONE',  ( -0.01601477604151182663, 0.9998717552508123996, -0.000000000000000000 ) ) ;
#22327 = FACE_OUTER_BOUND ( 'NONE', #36967, .T. ) ;
#22328 = CARTESIAN_POINT ( 'NONE',  ( -1.695772546416001392, 1.551146592414875958, -2.417756147381374010 ) ) ;
#22329 = DIRECTION ( 'NONE',  ( -0.7071067811865483499, -2.200518442539857142E-16, 0.7071067811865465735 ) ) ;
#22330 = EDGE_CURVE ( 'NONE', #50014, #20204, #3213, .T. ) ;
#22331 = DIRECTION ( 'NONE',  ( -1.000000000000000000, 0.000000000000000000, 1.734723475976806848E-16 ) ) ;
#22332 = VERTEX_POINT ( 'NONE', #3722 ) ;
#22333 = ORIENTED_EDGE ( 'NONE', *, *, #33464, .F. ) ;
#22334 = DIRECTION ( 'NONE',  ( 1.000000000000000000, 0.000000000000000000, 0.000000000000000000 ) ) ;
#22335 = CARTESIAN_POINT ( 'NONE',  ( 0.7423782071083091516, 0.000000000000000000, 1.377952755905504256 ) ) ;
#22336 = VECTOR ( 'NONE', #37719, 39.37007874015748143 ) ;
#22337 = EDGE_CURVE ( 'NONE', #12815, #46776, #26949, .T. ) ;
#22338 = LINE ( 'NONE', #38095, #5820 ) ;
#22339 = PLANE ( 'NONE',  #31098 ) ;
#22340 = CARTESIAN_POINT ( 'NONE',  ( -1.166969139818016199, 3.267716535433071279, -1.299212598425192544 ) ) ;
#22341 = VERTEX_POINT ( 'NONE', #49901 ) ;
#22342 = CARTESIAN_POINT ( 'NONE',  ( 2.059322335531026837, 3.346456692913386100, -0.6692913385826764205 ) ) ;
#22343 = VECTOR ( 'NONE', #44066, 39.37007874015748143 ) ;
#22344 = LINE ( 'NONE', #38101, #19899 ) ;
#22345 = ORIENTED_EDGE ( 'NONE', *, *, #28596, .F. ) ;
#22346 = DIRECTION ( 'NONE',  ( 0.000000000000000000, -1.000000000000000000, -0.000000000000000000 ) ) ;
#22347 = EDGE_CURVE ( 'NONE', #21029, #14001, #38836, .T. ) ;
#22348 = DIRECTION ( 'NONE',  ( 1.000000000000000000, -0.000000000000000000, 0.000000000000000000 ) ) ;
#22349 = VERTEX_POINT ( 'NONE', #31346 ) ;
#22350 = CARTESIAN_POINT ( 'NONE',  ( -2.182111253630085734, 3.267716535433071279, -0.8267716535433052849 ) ) ;
#22351 = EDGE_CURVE ( 'NONE', #29652, #5773, #24758, .T. ) ;
#22352 = CARTESIAN_POINT ( 'NONE',  ( -1.731130289826405155, 0.000000000000000000, 0.2179283737756174399 ) ) ;
#22353 = ADVANCED_FACE ( 'NONE', ( #3470 ), #26205, .T. ) ;
#22354 = PLANE ( 'NONE',  #49074 ) ;
#22355 = ORIENTED_EDGE ( 'NONE', *, *, #21962, .F. ) ;
#22356 = DIRECTION ( 'NONE',  ( -1.000000000000000000, 0.000000000000000000, 0.000000000000000000 ) ) ;
#22357 = VERTEX_POINT ( 'NONE', #18959 ) ;
#22358 = DIRECTION ( 'NONE',  ( 0.000000000000000000, -0.000000000000000000, 1.000000000000000000 ) ) ;
#22359 = CARTESIAN_POINT ( 'NONE',  ( -2.139229417893219853, 5.905511811023623991, -0.3394403656973702388 ) ) ;
#22360 = CARTESIAN_POINT ( 'NONE',  ( -1.252433315296644256, 1.589416742343778610, -1.807552045033091082 ) ) ;
#22361 = CARTESIAN_POINT ( 'NONE',  ( -0.6214413264104945434, 3.346456692913386100, -2.244094488188968395 ) ) ;
#22362 = ORIENTED_EDGE ( 'NONE', *, *, #8783, .T. ) ;
#22363 = ORIENTED_EDGE ( 'NONE', *, *, #13841, .F. ) ;
#22364 = CARTESIAN_POINT ( 'NONE',  ( 0.000000000000000000, 3.267716535433071279, -0.9448818897637765168 ) ) ;
#22365 = DIRECTION ( 'NONE',  ( -3.469446951953613696E-16, 0.000000000000000000, -1.000000000000000000 ) ) ;
#22366 = CARTESIAN_POINT ( 'NONE',  ( 2.100227814008711391, 1.467797480264206866, -2.076109931251913565 ) ) ;
#22367 = ADVANCED_FACE ( 'NONE', ( #42195 ), #41953, .F. ) ;
#22368 = DIRECTION ( 'NONE',  ( 0.000000000000000000, 0.000000000000000000, -1.000000000000000000 ) ) ;
#22369 = AXIS2_PLACEMENT_3D ( 'NONE', #20616, #4362, #12617 ) ;
#22370 = DIRECTION ( 'NONE',  ( -1.000000000000000000, -0.000000000000000000, -0.000000000000000000 ) ) ;
#22371 = ADVANCED_FACE ( 'NONE', ( #2708 ), #34712, .T. ) ;
#22372 = AXIS2_PLACEMENT_3D ( 'NONE', #25853, #9858, #6241 ) ;
#22373 = ORIENTED_EDGE ( 'NONE', *, *, #16701, .T. ) ;
#22374 = ORIENTED_EDGE ( 'NONE', *, *, #17947, .F. ) ;
#22375 = CARTESIAN_POINT ( 'NONE',  ( 0.9834642517162937025, 3.346456692913386100, -1.929133858267711110 ) ) ;
#22376 = EDGE_CURVE ( 'NONE', #33634, #8308, #31092, .T. ) ;
#22377 = CARTESIAN_POINT ( 'NONE',  ( 0.04921259842519689481, 1.205361022782829114E-17, 1.934165248549660987 ) ) ;
#22378 = ORIENTED_EDGE ( 'NONE', *, *, #113, .T. ) ;
#22379 = EDGE_CURVE ( 'NONE', #7604, #8873, #22580, .T. ) ;
#22380 = EDGE_CURVE ( 'NONE', #34607, #25178, #18458, .T. ) ;
#22381 = CARTESIAN_POINT ( 'NONE',  ( -0.04921259842519689481, 0.000000000000000000, -2.165433070866142007 ) ) ;
#22382 = ORIENTED_EDGE ( 'NONE', *, *, #13289, .T. ) ;
#22383 = VECTOR ( 'NONE', #32674, 39.37007874015748143 ) ;
#22384 = VERTEX_POINT ( 'NONE', #30333 ) ;
#22385 = AXIS2_PLACEMENT_3D ( 'NONE', #45608, #17265, #48449 ) ;
#22386 = VERTEX_POINT ( 'NONE', #2966 ) ;
#22387 = ORIENTED_EDGE ( 'NONE', *, *, #46001, .T. ) ;
#22388 = CARTESIAN_POINT ( 'NONE',  ( 0.000000000000000000, 3.267716535433071279, 1.732283464566921172 ) ) ;
#22389 = VERTEX_POINT ( 'NONE', #18716 ) ;
#22390 = LINE ( 'NONE', #34015, #42742 ) ;
#22391 = CARTESIAN_POINT ( 'NONE',  ( 2.182111253630085290, 0.000000000000000000, -1.161035397307311917E-15 ) ) ;
#22392 = CARTESIAN_POINT ( 'NONE',  ( 0.000000000000000000, 3.267716535433071279, -0.6299212598425177889 ) ) ;
#22393 = LINE ( 'NONE', #21382, #46682 ) ;
#22394 = CARTESIAN_POINT ( 'NONE',  ( 1.883550378546973603, 0.000000000000000000, -1.069467267250420628 ) ) ;
#22395 = EDGE_LOOP ( 'NONE', ( #33866, #30477, #9598, #48179, #34265 ) ) ;
#22396 = CARTESIAN_POINT ( 'NONE',  ( 0.2052282226254518727, 0.000000000000000000, -1.731265419273307682 ) ) ;
#22397 = DIRECTION ( 'NONE',  ( 1.000000000000000000, 0.000000000000000000, 0.000000000000000000 ) ) ;
#22398 = CARTESIAN_POINT ( 'NONE',  ( 1.835963193532814008, 1.671691464651421155, 1.401186513841017778 ) ) ;
#22399 = DIRECTION ( 'NONE',  ( 1.000000000000000000, 0.000000000000000000, -3.469446951953613696E-16 ) ) ;
#22400 = AXIS2_PLACEMENT_3D ( 'NONE', #32446, #47365, #16175 ) ;
#22401 = ORIENTED_EDGE ( 'NONE', *, *, #47374, .F. ) ;
#22402 = VECTOR ( 'NONE', #37055, 39.37007874015748143 ) ;
#22403 = FACE_OUTER_BOUND ( 'NONE', #51021, .T. ) ;
#22404 = CARTESIAN_POINT ( 'NONE',  ( -0.5455278134075216556, 0.000000000000000000, -2.204724409448810540 ) ) ;
#22405 = ORIENTED_EDGE ( 'NONE', *, *, #24494, .F. ) ;
#22406 = CARTESIAN_POINT ( 'NONE',  ( 0.000000000000000000, 3.267716535433071279, -0.5118110236220464460 ) ) ;
#22407 = DIRECTION ( 'NONE',  ( -3.469446951953613696E-16, 0.000000000000000000, -1.000000000000000000 ) ) ;
#22408 = EDGE_CURVE ( 'NONE', #20663, #12124, #34465, .T. ) ;
#22409 = VECTOR ( 'NONE', #37296, 39.37007874015748143 ) ;
#22410 = EDGE_LOOP ( 'NONE', ( #39465, #5489, #50632, #12062 ) ) ;
#22411 = EDGE_CURVE ( 'NONE', #1486, #36726, #46304, .T. ) ;
#22412 = AXIS2_PLACEMENT_3D ( 'NONE', #16211, #35833, #8212 ) ;
#22413 = DIRECTION ( 'NONE',  ( -1.000000000000000000, 0.000000000000000000, 0.000000000000000000 ) ) ;
#22414 = ORIENTED_EDGE ( 'NONE', *, *, #41233, .F. ) ;
#22415 = CARTESIAN_POINT ( 'NONE',  ( 1.560669927219590525, 0.000000000000000000, 0.2755905511810996522 ) ) ;
#22416 = EDGE_CURVE ( 'NONE', #43660, #13332, #4221, .T. ) ;
#22417 = CARTESIAN_POINT ( 'NONE',  ( -0.4161812636739087856, 0.000000000000000000, -1.692983086477939825 ) ) ;
#22418 = AXIS2_PLACEMENT_3D ( 'NONE', #33909, #18664, #18406 ) ;
#22419 = DIRECTION ( 'NONE',  ( 0.000000000000000000, 0.000000000000000000, -1.000000000000000000 ) ) ;
#22420 = DIRECTION ( 'NONE',  ( 1.734723475976806848E-16, 0.000000000000000000, 1.000000000000000000 ) ) ;
#22421 = CARTESIAN_POINT ( 'NONE',  ( -0.2727639067037608278, 0.000000000000000000, 2.165354330708650465 ) ) ;
#22422 = ORIENTED_EDGE ( 'NONE', *, *, #16845, .F. ) ;
#22423 = CARTESIAN_POINT ( 'NONE',  ( 1.091055626815042645, 3.346456692913386100, -0.1968503937007883287 ) ) ;
#22424 = ORIENTED_EDGE ( 'NONE', *, *, #24917, .T. ) ;
#22425 = EDGE_LOOP ( 'NONE', ( #9978, #8337, #41600, #47179 ) ) ;
#22426 = DIRECTION ( 'NONE',  ( -0.5407162030609373726, -0.6444004775717706579, -0.5407162030609373726 ) ) ;
#22427 = ORIENTED_EDGE ( 'NONE', *, *, #33812, .T. ) ;
#22428 = CARTESIAN_POINT ( 'NONE',  ( -0.8942052331142552601, 3.346456692913386100, -0.9448818897637760728 ) ) ;
#22429 = LINE ( 'NONE', #18557, #44176 ) ;
#22430 = VERTEX_POINT ( 'NONE', #24615 ) ;
#22431 = DIRECTION ( 'NONE',  ( 1.000000000000000000, 0.000000000000000000, 0.000000000000000000 ) ) ;
#22432 = EDGE_CURVE ( 'NONE', #784, #50140, #36493, .T. ) ;
#22433 = CARTESIAN_POINT ( 'NONE',  ( 0.000000000000000000, 3.267716535433071279, 2.047244094488179567 ) ) ;
#22434 = CARTESIAN_POINT ( 'NONE',  ( -0.8182917201112819283, 0.000000000000000000, -0.4724409448818886470 ) ) ;
#22435 = ORIENTED_EDGE ( 'NONE', *, *, #30819, .T. ) ;
#22436 = ORIENTED_EDGE ( 'NONE', *, *, #13576, .F. ) ;
#22437 = EDGE_CURVE ( 'NONE', #25003, #47775, #29133, .T. ) ;
#22438 = LINE ( 'NONE', #10054, #9218 ) ;
#22439 = FACE_BOUND ( 'NONE', #13645, .T. ) ;
#22440 = ORIENTED_EDGE ( 'NONE', *, *, #10574, .F. ) ;
#22441 = VECTOR ( 'NONE', #10943, 39.37007874015748143 ) ;
#22442 = CARTESIAN_POINT ( 'NONE',  ( -0.8182917201112819283, 3.346456692913386100, -1.732283464566922726 ) ) ;
#22443 = CARTESIAN_POINT ( 'NONE',  ( -0.5455270741695672498, 1.205361022782829114E-17, -1.791688814994948808 ) ) ;
#22444 = ORIENTED_EDGE ( 'NONE', *, *, #2947, .T. ) ;
#22445 = ORIENTED_EDGE ( 'NONE', *, *, #1701, .F. ) ;
#22446 = LINE ( 'NONE', #19312, #36483 ) ;
#22447 = VECTOR ( 'NONE', #18053, 39.37007874015748143 ) ;
#22448 = LINE ( 'NONE', #35078, #24579 ) ;
#22449 = ORIENTED_EDGE ( 'NONE', *, *, #5121, .F. ) ;
#22450 = ORIENTED_EDGE ( 'NONE', *, *, #3745, .F. ) ;
#22451 = VECTOR ( 'NONE', #32165, 39.37007874015748143 ) ;
#22452 = ORIENTED_EDGE ( 'NONE', *, *, #19758, .F. ) ;
#22453 = DIRECTION ( 'NONE',  ( 0.9998717552508121775, 0.01601477604151182663, 0.000000000000000000 ) ) ;
#22454 = VECTOR ( 'NONE', #40197, 39.37007874015748143 ) ;
#22455 = FACE_OUTER_BOUND ( 'NONE', #31789, .T. ) ;
#22456 = CARTESIAN_POINT ( 'NONE',  ( -0.2727639067037607723, 3.267716535433071279, 0.4724409448818869817 ) ) ;
#22457 = EDGE_LOOP ( 'NONE', ( #4695, #20494, #16975, #47129, #6060 ) ) ;
#22458 = ORIENTED_EDGE ( 'NONE', *, *, #3746, .T. ) ;
#22459 = LINE ( 'NONE', #14712, #1030 ) ;
#22460 =( NAMED_UNIT ( * ) PLANE_ANGLE_UNIT ( ) SI_UNIT ( $, .RADIAN. ) );
#22461 = LINE ( 'NONE', #26077, #43092 ) ;
#22462 = DIRECTION ( 'NONE',  ( 1.000000000000000000, 0.000000000000000000, 0.000000000000000000 ) ) ;
#22463 = CARTESIAN_POINT ( 'NONE',  ( -0.7381027496704855029, 1.707760278544290689, -2.859439394060923512 ) ) ;
#22464 = DIRECTION ( 'NONE',  ( -0.01601477604151182663, 0.9998717552508123996, -0.000000000000000000 ) ) ;
#22465 = CARTESIAN_POINT ( 'NONE',  ( 1.775400203342705430, 5.905511811023623991, -2.359903268218702888 ) ) ;
#22466 = ADVANCED_FACE ( 'NONE', ( #47040 ), #1112, .F. ) ;
#22467 = ORIENTED_EDGE ( 'NONE', *, *, #31643, .T. ) ;
#22468 = DIRECTION ( 'NONE',  ( -3.469446951953613696E-16, 0.000000000000000000, -1.000000000000000000 ) ) ;
#22469 = LINE ( 'NONE', #41839, #12895 ) ;
#22470 = ADVANCED_FACE ( 'NONE', ( #35722 ), #43237, .T. ) ;
#22471 = ORIENTED_EDGE ( 'NONE', *, *, #22310, .T. ) ;
#22472 = EDGE_CURVE ( 'NONE', #18617, #13074, #19326, .T. ) ;
#22473 = VERTEX_POINT ( 'NONE', #23846 ) ;
#22474 = FACE_OUTER_BOUND ( 'NONE', #10219, .T. ) ;
#22475 = VECTOR ( 'NONE', #12395, 39.37007874015748143 ) ;
#22476 = CARTESIAN_POINT ( 'NONE',  ( -1.740978969773838037, 0.000000000000000000, 0.09160132170885167124 ) ) ;
#22477 = VERTEX_POINT ( 'NONE', #27709 ) ;
#22478 = VECTOR ( 'NONE', #6372, 39.37007874015748143 ) ;
#22479 = VERTEX_POINT ( 'NONE', #16100 ) ;
#22480 = CARTESIAN_POINT ( 'NONE',  ( 0.000000000000000000, 3.267716535433071279, -0.4724409448818883694 ) ) ;
#22481 = AXIS2_PLACEMENT_3D ( 'NONE', #28967, #40353, #16861 ) ;
#22482 = ORIENTED_EDGE ( 'NONE', *, *, #46574, .T. ) ;
#22483 = AXIS2_PLACEMENT_3D ( 'NONE', #12999, #16874, #21760 ) ;
#22484 = AXIS2_PLACEMENT_3D ( 'NONE', #36686, #48509, #25311 ) ;
#22485 = LINE ( 'NONE', #10612, #16101 ) ;
#22486 = PLANE ( 'NONE',  #19775 ) ;
#22487 = EDGE_CURVE ( 'NONE', #22384, #45444, #11716, .T. ) ;
#22488 = VERTEX_POINT ( 'NONE', #16360 ) ;
#22489 = DIRECTION ( 'NONE',  ( -1.000000000000000000, 0.000000000000000000, 1.734723475976806848E-16 ) ) ;
#22490 = ORIENTED_EDGE ( 'NONE', *, *, #33087, .T. ) ;
#22491 = VERTEX_POINT ( 'NONE', #20734 ) ;
#22492 = ADVANCED_FACE ( 'NONE', ( #39595 ), #15838, .F. ) ;
#22493 = DIRECTION ( 'NONE',  ( -0.000000000000000000, 1.000000000000000000, -0.000000000000000000 ) ) ;
#22494 = FACE_OUTER_BOUND ( 'NONE', #40808, .T. ) ;
#22495 = CARTESIAN_POINT ( 'NONE',  ( 0.1067246931122726866, 0.02962905676920215767, 0.000000000000000000 ) ) ;
#22496 = LINE ( 'NONE', #50552, #44137 ) ;
#22497 = VERTEX_POINT ( 'NONE', #19710 ) ;
#22498 = DIRECTION ( 'NONE',  ( -0.3090169943749582204, -1.103800545167488837E-16, 0.9510565162951500895 ) ) ;
#22499 = DIRECTION ( 'NONE',  ( 1.000000000000000000, 0.000000000000000000, -3.469446951953613696E-16 ) ) ;
#22500 = LINE ( 'NONE', #38256, #42649 ) ;
#22501 = EDGE_LOOP ( 'NONE', ( #47670, #41935, #1130, #25118 ) ) ;
#22502 = CARTESIAN_POINT ( 'NONE',  ( 0.000000000000000000, 2.755905511811024056, 0.000000000000000000 ) ) ;
#22503 = ORIENTED_EDGE ( 'NONE', *, *, #39126, .T. ) ;
#22504 = EDGE_LOOP ( 'NONE', ( #34181, #10505, #1557, #25742 ) ) ;
#22505 = EDGE_CURVE ( 'NONE', #50243, #1125, #24099, .T. ) ;
#22506 = CARTESIAN_POINT ( 'NONE',  ( 0.1968503937007873017, 0.000000000000000000, -0.6299212598425177889 ) ) ;
#22507 =( BOUNDED_CURVE ( )  B_SPLINE_CURVE ( 3, ( #50167, #42463, #22851, #15356 ),
 .UNSPECIFIED., .F., .F. ) 
 B_SPLINE_CURVE_WITH_KNOTS ( ( 4, 4 ),
 ( 2.340218168529833331, 2.391075478467469484 ),
 .UNSPECIFIED. ) 
 CURVE ( )  GEOMETRIC_REPRESENTATION_ITEM ( )  RATIONAL_B_SPLINE_CURVE ( ( 1.000000000000000000, 0.9997844727828222311, 0.9997844727828222311, 1.000000000000000000 ) ) 
 REPRESENTATION_ITEM ( '' )  );
#22508 = LINE ( 'NONE', #7013, #21198 ) ;
#22509 = DIRECTION ( 'NONE',  ( -1.000000000000000000, 0.000000000000000000, 0.000000000000000000 ) ) ;
#22510 = ORIENTED_EDGE ( 'NONE', *, *, #2884, .T. ) ;
#22511 = ORIENTED_EDGE ( 'NONE', *, *, #39726, .T. ) ;
#22512 = VECTOR ( 'NONE', #28780, 39.37007874015748143 ) ;
#22513 = DIRECTION ( 'NONE',  ( -0.9909497617679352555, 0.000000000000000000, 0.1342332658176522697 ) ) ;
#22514 = ORIENTED_EDGE ( 'NONE', *, *, #45021, .T. ) ;
#22515 = LINE ( 'NONE', #46235, #4346 ) ;
#22516 = DIRECTION ( 'NONE',  ( 0.000000000000000000, -1.000000000000000000, 0.000000000000000000 ) ) ;
#22517 = VECTOR ( 'NONE', #2584, 39.37007874015748143 ) ;
#22518 = B_SPLINE_CURVE_WITH_KNOTS ( 'NONE', 3,
 ( #14265, #46237, #18655, #34403 ),
 .UNSPECIFIED., .F., .F.,
 ( 4, 4 ),
 ( 0.002149632668185018445, 0.004753995714153514546 ),
 .UNSPECIFIED. ) ;
#22519 = DIRECTION ( 'NONE',  ( -0.000000000000000000, 1.000000000000000000, -0.000000000000000000 ) ) ;
#22520 = CARTESIAN_POINT ( 'NONE',  ( 1.557927422371225612, 0.000000000000000000, 0.7824709080581413456 ) ) ;
#22521 = FACE_OUTER_BOUND ( 'NONE', #25562, .T. ) ;
#22522 = VECTOR ( 'NONE', #11779, 39.37007874015748143 ) ;
#22523 = VERTEX_POINT ( 'NONE', #36242 ) ;
#22524 = DIRECTION ( 'NONE',  ( -1.000000000000000000, 0.000000000000000000, 0.000000000000000000 ) ) ;
#22525 = CARTESIAN_POINT ( 'NONE',  ( 1.723687301221655810, 5.905511811023623991, -1.311649477509801098 ) ) ;
#22526 = CARTESIAN_POINT ( 'NONE',  ( 0.2727639067037604947, 0.000000000000000000, -1.417322834645664331 ) ) ;
#22527 = ADVANCED_FACE ( 'NONE', ( #43451 ), #18537, .T. ) ;
#22528 = ORIENTED_EDGE ( 'NONE', *, *, #18615, .T. ) ;
#22529 = CARTESIAN_POINT ( 'NONE',  ( 1.560669927219590747, 3.346456692913386100, 1.414498409778230492 ) ) ;
#22530 = CARTESIAN_POINT ( 'NONE',  ( -1.825231763670859042, 0.5249316497054293817, -0.4670754313976908101 ) ) ;
#22531 = CARTESIAN_POINT ( 'NONE',  ( 0.4787700707360283414, 1.205361022782829114E-17, -1.919768535593459724 ) ) ;
#22532 = ADVANCED_FACE ( 'NONE', ( #47295 ), #12228, .T. ) ;
#22533 = ORIENTED_EDGE ( 'NONE', *, *, #13198, .T. ) ;
#22534 = EDGE_CURVE ( 'NONE', #39686, #17583, #12738, .T. ) ;
#22535 = PLANE ( 'NONE',  #322 ) ;
#22536 = VERTEX_POINT ( 'NONE', #24359 ) ;
#22537 = CYLINDRICAL_SURFACE ( 'NONE', #6574, 2.066929133858268042 ) ;
#22538 = VERTEX_POINT ( 'NONE', #20218 ) ;
#22539 = FACE_OUTER_BOUND ( 'NONE', #47447, .T. ) ;
#22540 = CARTESIAN_POINT ( 'NONE',  ( 0.000000000000000000, 1.574803149606302854, 0.000000000000000000 ) ) ;
#22541 = DIRECTION ( 'NONE',  ( -1.000000000000000000, 0.000000000000000000, 1.734723475976806848E-16 ) ) ;
#22542 = LINE ( 'NONE', #42411, #33491 ) ;
#22543 = EDGE_CURVE ( 'NONE', #38185, #43953, #35983, .T. ) ;
#22544 = VECTOR ( 'NONE', #33376, 39.37007874015748143 ) ;
#22545 = ORIENTED_EDGE ( 'NONE', *, *, #34380, .F. ) ;
#22546 = VERTEX_POINT ( 'NONE', #40111 ) ;
#22547 = CARTESIAN_POINT ( 'NONE',  ( 2.353959093805374377E-19, 5.905511811023623991, 2.952755905511811108 ) ) ;
#22548 = CARTESIAN_POINT ( 'NONE',  ( 1.287906020515829919, 3.267716535433071279, -1.456692913385822630 ) ) ;
#22549 = ORIENTED_EDGE ( 'NONE', *, *, #1274, .T. ) ;
#22550 = VECTOR ( 'NONE', #37858, 39.37007874015748143 ) ;
#22551 = CARTESIAN_POINT ( 'NONE',  ( 0.3015460593140593115, 0.000000000000000000, 1.937268728265797213 ) ) ;
#22552 = DIRECTION ( 'NONE',  ( -1.000000000000000000, -0.000000000000000000, -0.000000000000000000 ) ) ;
#22553 = CARTESIAN_POINT ( 'NONE',  ( 0.000000000000000000, 3.267716535433071279, -1.417322834645664331 ) ) ;
#22554 = VECTOR ( 'NONE', #50763, 39.37007874015748143 ) ;
#22555 = VECTOR ( 'NONE', #15155, 39.37007874015748854 ) ;
#22556 = ORIENTED_EDGE ( 'NONE', *, *, #14540, .F. ) ;
#22557 = ORIENTED_EDGE ( 'NONE', *, *, #20471, .F. ) ;
#22558 = CARTESIAN_POINT ( 'NONE',  ( 1.502052629464437183, 0.01692425682782448815, -1.368022823756944950 ) ) ;
#22559 = CARTESIAN_POINT ( 'NONE',  ( -0.5455278134075208785, 3.346456692913386100, 1.692913385826762873 ) ) ;
#22560 = EDGE_CURVE ( 'NONE', #19371, #25220, #865, .T. ) ;
#22561 = CARTESIAN_POINT ( 'NONE',  ( 3.927031490892378253E-16, 3.346456692913386100, 1.062992125984246083 ) ) ;
#22562 = ORIENTED_EDGE ( 'NONE', *, *, #46128, .T. ) ;
#22563 = DIRECTION ( 'NONE',  ( -0.01601477604151182663, 0.9998717552508123996, -0.000000000000000000 ) ) ;
#22564 = FACE_OUTER_BOUND ( 'NONE', #25819, .T. ) ;
#22565 = CIRCLE ( 'NONE', #6898, 2.165354330708661568 ) ;
#22566 = EDGE_LOOP ( 'NONE', ( #47927, #32798, #50048, #29141 ) ) ;
#22567 = CARTESIAN_POINT ( 'NONE',  ( 1.560669927219590525, 3.267716535433071279, 1.220472440944875281 ) ) ;
#22568 = VERTEX_POINT ( 'NONE', #37009 ) ;
#22569 = ORIENTED_EDGE ( 'NONE', *, *, #46758, .F. ) ;
#22570 = DIRECTION ( 'NONE',  ( 0.9998717552508121775, 0.01601477604151182663, 0.000000000000000000 ) ) ;
#22571 = PLANE ( 'NONE',  #20093 ) ;
#22572 = EDGE_CURVE ( 'NONE', #50201, #21785, #6268, .T. ) ;
#22573 = DIRECTION ( 'NONE',  ( -3.469446951953613696E-16, 0.000000000000000000, -1.000000000000000000 ) ) ;
#22574 = CARTESIAN_POINT ( 'NONE',  ( 0.04921259842519669359, 1.574803149606302854, 2.164795024401847456 ) ) ;
#22575 = LINE ( 'NONE', #30328, #32933 ) ;
#22576 = ORIENTED_EDGE ( 'NONE', *, *, #6125, .T. ) ;
#22577 = EDGE_CURVE ( 'NONE', #16254, #16314, #44720, .T. ) ;
#22578 = ORIENTED_EDGE ( 'NONE', *, *, #24207, .T. ) ;
#22579 = CARTESIAN_POINT ( 'NONE',  ( 0.1968503937007878568, 3.267716535433071279, 0.9448818897637749625 ) ) ;
#22580 = LINE ( 'NONE', #38341, #47341 ) ;
#22581 = EDGE_CURVE ( 'NONE', #16346, #50666, #37262, .T. ) ;
#22582 = FACE_OUTER_BOUND ( 'NONE', #10942, .T. ) ;
#22583 = VECTOR ( 'NONE', #12799, 39.37007874015748143 ) ;
#22584 = DIRECTION ( 'NONE',  ( 0.8805955318567321166, 0.000000000000000000, 0.4738686624730094055 ) ) ;
#22585 = CARTESIAN_POINT ( 'NONE',  ( -1.232620761116186126, 5.905511811023623991, -1.780282403660754076 ) ) ;
#22586 = ORIENTED_EDGE ( 'NONE', *, *, #21962, .T. ) ;
#22587 = CONICAL_SURFACE ( 'NONE', #35780, 2.246510896728926010, 0.01601546068027819014 ) ;
#22588 = CARTESIAN_POINT ( 'NONE',  ( -0.04921259842519708910, 1.710906707958852691, 2.478400121980571580 ) ) ;
#22589 = AXIS2_PLACEMENT_3D ( 'NONE', #27852, #47695, #23729 ) ;
#22590 = LINE ( 'NONE', #10968, #3410 ) ;
#22591 = AXIS2_PLACEMENT_3D ( 'NONE', #10153, #50107, #42150 ) ;
#22592 = EDGE_CURVE ( 'NONE', #16822, #24184, #25885, .T. ) ;
#22593 = CIRCLE ( 'NONE', #323, 2.165354330708661568 ) ;
#22594 = VERTEX_POINT ( 'NONE', #33397 ) ;
#22595 = LINE ( 'NONE', #6347, #9187 ) ;
#22596 = CARTESIAN_POINT ( 'NONE',  ( 2.326943258702977246, 1.646747008850265370, -0.05524094006260020506 ) ) ;
#22597 = VERTEX_POINT ( 'NONE', #13506 ) ;
#22598 = DIRECTION ( 'NONE',  ( 1.000000000000000000, -0.000000000000000000, 0.000000000000000000 ) ) ;
#22599 = ADVANCED_FACE ( 'NONE', ( #25122 ), #44477, .F. ) ;
#22600 = DIRECTION ( 'NONE',  ( 0.000000000000000000, 0.000000000000000000, 1.000000000000000000 ) ) ;
#22601 = EDGE_CURVE ( 'NONE', #25893, #47284, #5242, .T. ) ;
#22602 = CARTESIAN_POINT ( 'NONE',  ( -1.181102362204724310, 0.4724409448818890911, -1.062992125984252079 ) ) ;
#22603 = VECTOR ( 'NONE', #36437, 39.37007874015748143 ) ;
#22604 = EDGE_CURVE ( 'NONE', #42532, #49343, #40873, .T. ) ;
#22605 = ORIENTED_EDGE ( 'NONE', *, *, #13871, .T. ) ;
#22606 = CARTESIAN_POINT ( 'NONE',  ( -0.8942052331142547050, 3.346456692913386100, 0.6299212598425164567 ) ) ;
#22607 = ORIENTED_EDGE ( 'NONE', *, *, #36811, .T. ) ;
#22608 = FACE_BOUND ( 'NONE', #15849, .T. ) ;
#22609 = DIRECTION ( 'NONE',  ( 1.000000000000000000, -0.000000000000000000, 0.000000000000000000 ) ) ;
#22610 = CARTESIAN_POINT ( 'NONE',  ( 1.068402561569975484, 0.000000000000000000, -1.884154513482173554 ) ) ;
#22611 = VERTEX_POINT ( 'NONE', #49078 ) ;
#22612 = VERTEX_POINT ( 'NONE', #9635 ) ;
#22613 = CARTESIAN_POINT ( 'NONE',  ( -0.5455278134075214336, 0.000000000000000000, -0.3149606299212593941 ) ) ;
#22614 = CARTESIAN_POINT ( 'NONE',  ( 0.000000000000000000, 3.267716535433071279, 1.062992125984246083 ) ) ;
#22615 = LINE ( 'NONE', #27235, #38405 ) ;
#22616 = CARTESIAN_POINT ( 'NONE',  ( 0.000000000000000000, 3.267716535433071279, 0.000000000000000000 ) ) ;
#22617 = DIRECTION ( 'NONE',  ( 1.000000000000000000, 0.000000000000000000, -3.469446951953613696E-16 ) ) ;
#22618 = EDGE_LOOP ( 'NONE', ( #48921, #50284, #6219, #24942 ) ) ;
#22619 = VERTEX_POINT ( 'NONE', #2393 ) ;
#22620 = CARTESIAN_POINT ( 'NONE',  ( -0.3486774197067340486, 3.346456692913386100, -0.5118110236220467790 ) ) ;
#22621 = EDGE_CURVE ( 'NONE', #27965, #43528, #32629, .T. ) ;
#22622 = AXIS2_PLACEMENT_3D ( 'NONE', #43112, #42622, #46717 ) ;
#22623 = CARTESIAN_POINT ( 'NONE',  ( -1.985260859929297794, 3.267716535433071279, 6.887757239314512246E-16 ) ) ;
#22624 = CIRCLE ( 'NONE', #29210, 2.443628662382284489 ) ;
#22625 = ORIENTED_EDGE ( 'NONE', *, *, #25261, .F. ) ;
#22626 = CARTESIAN_POINT ( 'NONE',  ( 1.091055626815042645, 3.346456692913386100, -0.6299212598425181220 ) ) ;
#22627 = VECTOR ( 'NONE', #45067, 39.37007874015748143 ) ;
#22628 = ORIENTED_EDGE ( 'NONE', *, *, #24644, .F. ) ;
#22629 = EDGE_LOOP ( 'NONE', ( #3135, #32610, #2912, #2505 ) ) ;
#22630 = B_SPLINE_CURVE_WITH_KNOTS ( 'NONE', 3,
 ( #29228, #20715, #39826, #24598 ),
 .UNSPECIFIED., .F., .F.,
 ( 4, 4 ),
 ( 0.001625204961501889710, 0.002876679757166853129 ),
 .UNSPECIFIED. ) ;
#22631 = EDGE_CURVE ( 'NONE', #15706, #2298, #40621, .T. ) ;
#22632 = CIRCLE ( 'NONE', #16019, 2.106299212598425008 ) ;
#22633 = AXIS2_PLACEMENT_3D ( 'NONE', #32717, #20819, #36576 ) ;
#22634 = EDGE_CURVE ( 'NONE', #370, #16904, #13762, .T. ) ;
#22635 = EDGE_CURVE ( 'NONE', #869, #50130, #42480, .T. ) ;
#22636 = VERTEX_POINT ( 'NONE', #21761 ) ;
#22637 = VERTEX_POINT ( 'NONE', #41380 ) ;
#22638 = DIRECTION ( 'NONE',  ( 1.000000000000000000, 0.000000000000000000, 0.000000000000000000 ) ) ;
#22639 = VECTOR ( 'NONE', #35734, 39.37007874015748143 ) ;
#22640 = DIRECTION ( 'NONE',  ( -0.000000000000000000, 1.000000000000000000, -0.000000000000000000 ) ) ;
#22641 = CARTESIAN_POINT ( 'NONE',  ( 0.4696143004045483793, 3.267716535433071279, -1.629301903132388985E-16 ) ) ;
#22642 = DIRECTION ( 'NONE',  ( 0.000000000000000000, -1.000000000000000000, -0.000000000000000000 ) ) ;
#22643 = FACE_OUTER_BOUND ( 'NONE', #10184, .T. ) ;
#22644 = DIRECTION ( 'NONE',  ( 0.2225209339563041788, 0.000000000000000000, 0.9749279121818259508 ) ) ;
#22645 = EDGE_LOOP ( 'NONE', ( #1044, #23372, #47564, #30676 ) ) ;
#22646 = DIRECTION ( 'NONE',  ( -0.000000000000000000, 1.000000000000000000, -0.000000000000000000 ) ) ;
#22647 = CARTESIAN_POINT ( 'NONE',  ( 0.000000000000000000, 3.346456692913386100, 0.000000000000000000 ) ) ;
#22648 = DIRECTION ( 'NONE',  ( -1.000000000000000000, 0.000000000000000000, -0.000000000000000000 ) ) ;
#22649 = DIRECTION ( 'NONE',  ( -0.000000000000000000, 0.000000000000000000, 1.000000000000000000 ) ) ;
#22650 = EDGE_CURVE ( 'NONE', #1302, #42304, #22624, .T. ) ;
#22651 = VERTEX_POINT ( 'NONE', #5503 ) ;
#22652 = DIRECTION ( 'NONE',  ( 1.000000000000000000, -0.000000000000000000, 0.000000000000000000 ) ) ;
#22653 = CARTESIAN_POINT ( 'NONE',  ( -2.437180031585919782, 1.681273446161504426, -1.667735833703134718 ) ) ;
#22654 = ORIENTED_EDGE ( 'NONE', *, *, #8592, .T. ) ;
#22655 = DIRECTION ( 'NONE',  ( -0.000000000000000000, 1.000000000000000000, -0.000000000000000000 ) ) ;
#22656 = EDGE_CURVE ( 'NONE', #37684, #26933, #48575, .T. ) ;
#22657 = DIRECTION ( 'NONE',  ( -0.2225209339563041788, 1.288287287306305283E-16, -0.9749279121818259508 ) ) ;
#22658 = EDGE_CURVE ( 'NONE', #11104, #33373, #41131, .T. ) ;
#22659 = VERTEX_POINT ( 'NONE', #1628 ) ;
#22660 = VECTOR ( 'NONE', #32306, 39.37007874015748143 ) ;
#22661 = ADVANCED_FACE ( 'NONE', ( #37518 ), #9887, .T. ) ;
#22662 = VECTOR ( 'NONE', #25066, 39.37007874015748143 ) ;
#22663 = CARTESIAN_POINT ( 'NONE',  ( 2.378961647330872786, 0.000000000000000000, 0.1181102362204698858 ) ) ;
#22664 = ORIENTED_EDGE ( 'NONE', *, *, #43770, .F. ) ;
#22665 = CARTESIAN_POINT ( 'NONE',  ( 1.775400203342704764, 0.000000000000000000, -2.359903268218703332 ) ) ;
#22666 = VECTOR ( 'NONE', #14356, 39.37007874015748143 ) ;
#22667 = CARTESIAN_POINT ( 'NONE',  ( -0.8182917201112819283, 3.346456692913386100, -0.3543307086614175816 ) ) ;
#22668 = DIRECTION ( 'NONE',  ( 1.000000000000000000, 0.000000000000000000, 0.000000000000000000 ) ) ;
#22669 = DIRECTION ( 'NONE',  ( -3.469446951953613696E-16, 0.000000000000000000, -1.000000000000000000 ) ) ;
#22670 = CARTESIAN_POINT ( 'NONE',  ( 0.000000000000000000, 3.267716535433071279, 0.2755905511810996522 ) ) ;
#22671 = ORIENTED_EDGE ( 'NONE', *, *, #27134, .T. ) ;
#22672 = DIRECTION ( 'NONE',  ( 1.000000000000000000, 0.000000000000000000, -3.469446951953613696E-16 ) ) ;
#22673 = AXIS2_PLACEMENT_3D ( 'NONE', #44403, #47986, #8532 ) ;
#22674 = ORIENTED_EDGE ( 'NONE', *, *, #27046, .F. ) ;
#22675 = ORIENTED_EDGE ( 'NONE', *, *, #37032, .T. ) ;
#22676 = CARTESIAN_POINT ( 'NONE',  ( 0.5755393941981044037, 0.6859011407150840123, -1.392964542809770334 ) ) ;
#22677 = VERTEX_POINT ( 'NONE', #2136 ) ;
#22678 = CARTESIAN_POINT ( 'NONE',  ( 1.466506618346834934, 1.205361022782829114E-17, -1.470210429041567401 ) ) ;
#22679 = PLANE ( 'NONE',  #40060 ) ;
#22680 = EDGE_LOOP ( 'NONE', ( #43288, #46995, #27109, #3312 ) ) ;
#22681 = CARTESIAN_POINT ( 'NONE',  ( 0.000000000000000000, 0.000000000000000000, 0.000000000000000000 ) ) ;
#22682 = FACE_OUTER_BOUND ( 'NONE', #27343, .T. ) ;
#22684 = B_SPLINE_CURVE_WITH_KNOTS ( 'NONE', 3,
 ( #16394, #34997, #8642, #24390 ),
 .UNSPECIFIED., .F., .F.,
 ( 4, 4 ),
 ( 0.01072160935731267424, 0.03072004101276351595 ),
 .UNSPECIFIED. ) ;
#22683 = CARTESIAN_POINT ( 'NONE',  ( -1.712496953225537188, 0.000000000000000000, 0.5905511811023582691 ) ) ;
#22685 = ORIENTED_EDGE ( 'NONE', *, *, #50400, .T. ) ;
#22686 = VERTEX_POINT ( 'NONE', #17889 ) ;
#22687 = CARTESIAN_POINT ( 'NONE',  ( -1.636583440222564301, 3.267716535433071279, -0.6299212598425177889 ) ) ;
#22688 = FACE_BOUND ( 'NONE', #1722, .T. ) ;
#22689 = ORIENTED_EDGE ( 'NONE', *, *, #15047, .F. ) ;
#22690 = CARTESIAN_POINT ( 'NONE',  ( -1.636583440222564301, 3.346456692913386100, -1.259842519685034468 ) ) ;
#22691 = EDGE_CURVE ( 'NONE', #48087, #44092, #29757, .T. ) ;
#22692 = VERTEX_POINT ( 'NONE', #38773 ) ;
#22693 = VERTEX_POINT ( 'NONE', #34151 ) ;
#22694 = LINE ( 'NONE', #20853, #41456 ) ;
#22695 = EDGE_CURVE ( 'NONE', #869, #43448, #11120, .T. ) ;
#22696 = VECTOR ( 'NONE', #10773, 39.37007874015748143 ) ;
#22697 = DIRECTION ( 'NONE',  ( -2.582876339026174526E-17, -1.000000000000000000, -1.131632063491654496E-16 ) ) ;
#22698 = AXIS2_PLACEMENT_3D ( 'NONE', #39502, #8000, #40275 ) ;
#22699 = AXIS2_PLACEMENT_3D ( 'NONE', #18087, #10086, #33083 ) ;
#22700 = EDGE_LOOP ( 'NONE', ( #6240, #19841 ) ) ;
#22701 = DIRECTION ( 'NONE',  ( -2.582876339026174526E-17, -1.000000000000000000, -1.131632063491654496E-16 ) ) ;
#22702 = CIRCLE ( 'NONE', #32630, 2.165354330708661568 ) ;
#22703 = VERTEX_POINT ( 'NONE', #18898 ) ;
#22704 = LINE ( 'NONE', #50512, #38403 ) ;
#22705 = FACE_OUTER_BOUND ( 'NONE', #3417, .T. ) ;
#22706 = CARTESIAN_POINT ( 'NONE',  ( 1.363819533518803695, 3.267716535433071279, 1.535433070866133898 ) ) ;
#22707 = VERTEX_POINT ( 'NONE', #3401 ) ;
#22708 = EDGE_LOOP ( 'NONE', ( #44970, #3368, #42148, #43346 ) ) ;
#22709 = VECTOR ( 'NONE', #23111, 39.37007874015748143 ) ;
#22710 = LINE ( 'NONE', #46919, #4633 ) ;
#22711 = DIRECTION ( 'NONE',  ( -3.469446951953613696E-16, 0.000000000000000000, -1.000000000000000000 ) ) ;
#22712 = LINE ( 'NONE', #17824, #15911 ) ;
#22713 = EDGE_CURVE ( 'NONE', #11113, #11168, #14775, .T. ) ;
#22714 = PLANE ( 'NONE',  #11966 ) ;
#22715 = DIRECTION ( 'NONE',  ( -0.000000000000000000, 1.000000000000000000, -0.000000000000000000 ) ) ;
#22716 = EDGE_CURVE ( 'NONE', #10279, #40291, #34899, .T. ) ;
#22717 = DIRECTION ( 'NONE',  ( 0.000000000000000000, 0.000000000000000000, 1.000000000000000000 ) ) ;
#22718 = LINE ( 'NONE', #30213, #39098 ) ;
#22719 = EDGE_CURVE ( 'NONE', #388, #43639, #10893, .T. ) ;
#22720 = VERTEX_POINT ( 'NONE', #45730 ) ;
#22721 = CARTESIAN_POINT ( 'NONE',  ( -1.363819533518803029, 0.000000000000000000, 0.9055118110236167750 ) ) ;
#22722 = DIRECTION ( 'NONE',  ( -3.469446951953613696E-16, 0.000000000000000000, -1.000000000000000000 ) ) ;
#22723 = EDGE_CURVE ( 'NONE', #8328, #26516, #26637, .T. ) ;
#22724 = EDGE_CURVE ( 'NONE', #20325, #31865, #11149, .T. ) ;
#22725 = VERTEX_POINT ( 'NONE', #42381 ) ;
#22726 = ORIENTED_EDGE ( 'NONE', *, *, #29518, .T. ) ;
#22727 = DIRECTION ( 'NONE',  ( -1.000000000000000000, 0.000000000000000000, 5.782411586589357392E-17 ) ) ;
#22728 = PLANE ( 'NONE',  #37738 ) ;
#22729 = VERTEX_POINT ( 'NONE', #49835 ) ;
#22730 = MECHANICAL_DESIGN_GEOMETRIC_PRESENTATION_REPRESENTATION (  '', ( #40046 ), #44164 ) ;
#22731 = B_SPLINE_CURVE_WITH_KNOTS ( 'NONE', 3,
 ( #3790, #31668, #19776, #11534 ),
 .UNSPECIFIED., .F., .F.,
 ( 4, 4 ),
 ( 3.606898746852332451E-07, 0.04590458542295366290 ),
 .UNSPECIFIED. ) ;
#22732 = VECTOR ( 'NONE', #43316, 39.37007874015748854 ) ;
#22733 = ORIENTED_EDGE ( 'NONE', *, *, #39612, .T. ) ;
#22734 = DIRECTION ( 'NONE',  ( 1.000000000000000000, -0.000000000000000000, 0.000000000000000000 ) ) ;
#22735 = VECTOR ( 'NONE', #40525, 39.37007874015748143 ) ;
#22736 = ORIENTED_EDGE ( 'NONE', *, *, #40002, .T. ) ;
#22737 = CARTESIAN_POINT ( 'NONE',  ( 2.182111253630085290, 0.000000000000000000, -0.1968503937007886062 ) ) ;
#22738 = DIRECTION ( 'NONE',  ( -1.000000000000000000, 0.000000000000000000, 1.734723475976806848E-16 ) ) ;
#22739 = ORIENTED_EDGE ( 'NONE', *, *, #43445, .T. ) ;
#22740 = VECTOR ( 'NONE', #2806, 39.37007874015748143 ) ;
#22741 = B_SPLINE_CURVE_WITH_KNOTS ( 'NONE', 3,
 ( #13547, #5029, #1665, #12781 ),
 .UNSPECIFIED., .F., .F.,
 ( 4, 4 ),
 ( 2.052460024355699288E-07, 0.01596358452146435375 ),
 .UNSPECIFIED. ) ;
#22742 = FACE_OUTER_BOUND ( 'NONE', #12, .T. ) ;
#22743 = ORIENTED_EDGE ( 'NONE', *, *, #16710, .F. ) ;
#22744 = EDGE_LOOP ( 'NONE', ( #24387, #4913, #43335, #14112 ) ) ;
#22745 = CARTESIAN_POINT ( 'NONE',  ( -0.3225722872767163296, 0.000000000000000000, 1.868935683883109045 ) ) ;
#22746 = CARTESIAN_POINT ( 'NONE',  ( -0.5433753727366142927, 1.612341559703608596, 2.902374844030467305 ) ) ;
#22747 = DIRECTION ( 'NONE',  ( 0.01601477604151182663, -0.9998717552508123996, 0.000000000000000000 ) ) ;
#22748 = DIRECTION ( 'NONE',  ( -0.000000000000000000, 0.000000000000000000, 1.000000000000000000 ) ) ;
#22749 = ORIENTED_EDGE ( 'NONE', *, *, #32074, .F. ) ;
#22750 = CARTESIAN_POINT ( 'NONE',  ( 0.000000000000000000, 6.692913385826772199, 0.000000000000000000 ) ) ;
#22751 = LINE ( 'NONE', #27117, #27471 ) ;
#22752 = CARTESIAN_POINT ( 'NONE',  ( 0.000000000000000000, 3.267716535433071279, 1.377952755905504256 ) ) ;
#22753 = ORIENTED_EDGE ( 'NONE', *, *, #14726, .T. ) ;
#22754 = B_SPLINE_CURVE_WITH_KNOTS ( 'NONE', 3,
 ( #46002, #27151, #22285, #50347 ),
 .UNSPECIFIED., .F., .F.,
 ( 4, 4 ),
 ( 0.01224259289618789825, 0.03073794493652437163 ),
 .UNSPECIFIED. ) ;
#22755 = FACE_OUTER_BOUND ( 'NONE', #25848, .T. ) ;
#22756 = EDGE_CURVE ( 'NONE', #32762, #39747, #38055, .T. ) ;
#22757 = EDGE_CURVE ( 'NONE', #42801, #19974, #10276, .T. ) ;
#22758 = ORIENTED_EDGE ( 'NONE', *, *, #37827, .F. ) ;
#22759 = ORIENTED_EDGE ( 'NONE', *, *, #35593, .T. ) ;
#22760 = EDGE_CURVE ( 'NONE', #27748, #9948, #27139, .T. ) ;
#22761 = DIRECTION ( 'NONE',  ( -0.7071067811865482389, 0.000000000000000000, 0.7071067811865467956 ) ) ;
#22762 = CARTESIAN_POINT ( 'NONE',  ( -2.182111253630085290, 0.000000000000000000, 0.1181102362204704270 ) ) ;
#22764 = CARTESIAN_POINT ( 'NONE',  ( -1.977197495136348460, 1.643425115977502848, -0.8986141922004805549 ) ) ;
#22763 = VECTOR ( 'NONE', #24555, 39.37007874015748854 ) ;
#22765 = DIRECTION ( 'NONE',  ( -3.469446951953613696E-16, 0.000000000000000000, -1.000000000000000000 ) ) ;
#22766 = ORIENTED_EDGE ( 'NONE', *, *, #37663, .T. ) ;
#22767 = ORIENTED_EDGE ( 'NONE', *, *, #43321, .T. ) ;
#22768 = VECTOR ( 'NONE', #42643, 39.37007874015748143 ) ;
#22769 = CARTESIAN_POINT ( 'NONE',  ( -0.8182917201112819283, 3.346456692913386100, -0.4724409448818886470 ) ) ;
#22770 = VECTOR ( 'NONE', #40744, 39.37007874015748143 ) ;
#22771 = CARTESIAN_POINT ( 'NONE',  ( -2.576863348864732117, 1.205361022782829114E-17, 1.442554885838412071 ) ) ;
#22772 = VERTEX_POINT ( 'NONE', #31024 ) ;
#22773 = DIRECTION ( 'NONE',  ( 0.000000000000000000, 0.000000000000000000, 1.000000000000000000 ) ) ;
#22774 = CARTESIAN_POINT ( 'NONE',  ( 0.8329809839909848579, 0.000000000000000000, -2.833254665166554442 ) ) ;
#22775 = VECTOR ( 'NONE', #43166, 39.37007874015748143 ) ;
#22776 = EDGE_CURVE ( 'NONE', #39707, #48162, #46732, .T. ) ;
#22777 = VECTOR ( 'NONE', #35199, 39.37007874015748143 ) ;
#22778 = LINE ( 'NONE', #34652, #36568 ) ;
#22779 = FACE_OUTER_BOUND ( 'NONE', #12421, .T. ) ;
#22780 = FACE_OUTER_BOUND ( 'NONE', #19928, .T. ) ;
#22781 = AXIS2_PLACEMENT_3D ( 'NONE', #36593, #47905, #8966 ) ;
#22782 = ORIENTED_EDGE ( 'NONE', *, *, #23742, .F. ) ;
#22783 = PLANE ( 'NONE',  #34107 ) ;
#22784 = EDGE_CURVE ( 'NONE', #43935, #34736, #42132, .T. ) ;
#22785 = LINE ( 'NONE', #49594, #26515 ) ;
#22786 = EDGE_LOOP ( 'NONE', ( #8870, #32577, #49493, #30885 ) ) ;
#22787 = CARTESIAN_POINT ( 'NONE',  ( -1.117755760306016644, 0.3937007874015748254, -1.220472440944882164 ) ) ;
#22788 = CARTESIAN_POINT ( 'NONE',  ( -1.676283831994445306, 0.001070912127414903967, 0.4929124452910598198 ) ) ;
#22789 = DIRECTION ( 'NONE',  ( 0.000000000000000000, 0.000000000000000000, 1.000000000000000000 ) ) ;
#22790 = ORIENTED_EDGE ( 'NONE', *, *, #11853, .F. ) ;
#22791 = LINE ( 'NONE', #3165, #6935 ) ;
#22792 = VERTEX_POINT ( 'NONE', #14261 ) ;
#22793 = FACE_OUTER_BOUND ( 'NONE', #17967, .T. ) ;
#22794 = ORIENTED_EDGE ( 'NONE', *, *, #20598, .T. ) ;
#22795 = DIRECTION ( 'NONE',  ( -3.469446951953613696E-16, 0.000000000000000000, -1.000000000000000000 ) ) ;
#22796 = ADVANCED_FACE ( 'NONE', ( #50090 ), #15024, .F. ) ;
#22797 = ORIENTED_EDGE ( 'NONE', *, *, #36855, .T. ) ;
#22798 = DIRECTION ( 'NONE',  ( -4.561975526775602830E-17, -1.000000000000000000, -1.067327232801823148E-16 ) ) ;
#22799 = DIRECTION ( 'NONE',  ( -3.469446951953613696E-16, 0.000000000000000000, -1.000000000000000000 ) ) ;
#22800 = LINE ( 'NONE', #3431, #26852 ) ;
#22801 = VECTOR ( 'NONE', #14089, 39.37007874015748143 ) ;
#22802 = ORIENTED_EDGE ( 'NONE', *, *, #17440, .F. ) ;
#22803 = EDGE_LOOP ( 'NONE', ( #42242, #24975, #26437, #43830 ) ) ;
#22804 = ORIENTED_EDGE ( 'NONE', *, *, #9634, .F. ) ;
#22805 = DIRECTION ( 'NONE',  ( 1.000000000000000000, 0.000000000000000000, -3.469446951953613696E-16 ) ) ;
#22806 = VECTOR ( 'NONE', #34266, 39.37007874015748143 ) ;
#22807 = DIRECTION ( 'NONE',  ( -0.9998717552508121775, -0.01601477604151182663, 0.000000000000000000 ) ) ;
#22808 = CIRCLE ( 'NONE', #1354, 1.850107469027523432 ) ;
#22809 = ORIENTED_EDGE ( 'NONE', *, *, #15333, .T. ) ;
#22810 = CARTESIAN_POINT ( 'NONE',  ( 0.5455278134075208785, 0.000000000000000000, -1.889763779527552812 ) ) ;
#22811 = LINE ( 'NONE', #31064, #49122 ) ;
#22812 = CARTESIAN_POINT ( 'NONE',  ( 2.378961647330872786, 3.267716535433071279, 0.3149606299212573401 ) ) ;
#22813 = ORIENTED_EDGE ( 'NONE', *, *, #42061, .F. ) ;
#22814 = ORIENTED_EDGE ( 'NONE', *, *, #49037, .T. ) ;
#22815 = CARTESIAN_POINT ( 'NONE',  ( 0.1968503937007875237, 3.267716535433071279, -6.829619984160660511E-17 ) ) ;
#22816 = CARTESIAN_POINT ( 'NONE',  ( 1.015142113812069979, 3.267716535433071279, 1.220472440944875281 ) ) ;
#22817 = VECTOR ( 'NONE', #16936, 39.37007874015748143 ) ;
#22818 = DIRECTION ( 'NONE',  ( -8.021399753802198224E-17, -1.000000000000000000, 8.389726389140549123E-17 ) ) ;
#22819 = ORIENTED_EDGE ( 'NONE', *, *, #30270, .F. ) ;
#22820 = CARTESIAN_POINT ( 'NONE',  ( -2.695799277629577162, 1.677241212940233872, -1.205759334241492509 ) ) ;
#22822 = VECTOR ( 'NONE', #11944, 39.37007874015748143 ) ;
#22821 = PLANE ( 'NONE',  #29339 ) ;
#22823 = ORIENTED_EDGE ( 'NONE', *, *, #33072, .F. ) ;
#22824 = EDGE_CURVE ( 'NONE', #20090, #12774, #6772, .T. ) ;
#22825 = CARTESIAN_POINT ( 'NONE',  ( 1.909347346926324684, 3.346456692913386100, -0.6692913385826764205 ) ) ;
#22826 = ORIENTED_EDGE ( 'NONE', *, *, #25620, .T. ) ;
#22827 = ORIENTED_EDGE ( 'NONE', *, *, #41773, .F. ) ;
#22828 = PLANE ( 'NONE',  #8948 ) ;
#22829 = DIRECTION ( 'NONE',  ( 1.000000000000000000, 0.000000000000000000, 0.000000000000000000 ) ) ;
#22830 = ADVANCED_FACE ( 'NONE', ( #11401 ), #7526, .F. ) ;
#22831 = FACE_OUTER_BOUND ( 'NONE', #34014, .T. ) ;
#22832 = EDGE_CURVE ( 'NONE', #14060, #9230, #2644, .T. ) ;
#22833 = CARTESIAN_POINT ( 'NONE',  ( 3.937007874015748143, 4.960629921259846142, -1.023622047244094224 ) ) ;
#22834 = EDGE_CURVE ( 'NONE', #14569, #17840, #18652, .T. ) ;
#22835 = FACE_OUTER_BOUND ( 'NONE', #24908, .T. ) ;
#22836 = ORIENTED_EDGE ( 'NONE', *, *, #49301, .F. ) ;
#22837 = ORIENTED_EDGE ( 'NONE', *, *, #23986, .T. ) ;
#22838 = DIRECTION ( 'NONE',  ( -0.4338837391175526803, 0.000000000000000000, -0.9009688679024218105 ) ) ;
#22839 = CARTESIAN_POINT ( 'NONE',  ( 1.511286805986086890, 0.000000000000000000, 0.8691436966267173103 ) ) ;
#22840 = EDGE_CURVE ( 'NONE', #20337, #22536, #35913, .T. ) ;
#22841 = CONICAL_SURFACE ( 'NONE', #35220, 2.165354330708661568, 0.2617993877991570129 ) ;
#22842 = CARTESIAN_POINT ( 'NONE',  ( -0.7053729475263631477, 3.346456692913386100, 2.047244094488179567 ) ) ;
#22843 = CARTESIAN_POINT ( 'NONE',  ( 1.003959327938112933, 1.731243926512280762, 2.534982793440925253 ) ) ;
#22844 = ORIENTED_EDGE ( 'NONE', *, *, #33276, .T. ) ;
#22845 = CARTESIAN_POINT ( 'NONE',  ( 1.034308760555261886, 1.626043101691516890, -2.034340803895991812 ) ) ;
#22846 = ADVANCED_FACE ( 'NONE', ( #12671 ), #39270, .F. ) ;
#22847 = CARTESIAN_POINT ( 'NONE',  ( 1.015142113812069313, 0.000000000000000000, -0.7874015748031473194 ) ) ;
#22848 = ORIENTED_EDGE ( 'NONE', *, *, #457, .T. ) ;
#22849 = CARTESIAN_POINT ( 'NONE',  ( 0.000000000000000000, 3.267716535433071279, 2.204724409448808764 ) ) ;
#22850 = DIRECTION ( 'NONE',  ( 1.000000000000000000, 0.000000000000000000, -3.469446951953613696E-16 ) ) ;
#22851 = CARTESIAN_POINT ( 'NONE',  ( -1.198835066468417310, 0.000000000000000000, 1.347140709999463670 ) ) ;
#22852 = VECTOR ( 'NONE', #20472, 39.37007874015748143 ) ;
#22853 = EDGE_CURVE ( 'NONE', #12600, #29231, #16554, .T. ) ;
#22854 = FACE_OUTER_BOUND ( 'NONE', #1718, .T. ) ;
#22855 = LINE ( 'NONE', #39356, #36565 ) ;
#22856 = CARTESIAN_POINT ( 'NONE',  ( 0.8329809839909849689, 1.496921813388997435, -2.833254665166554442 ) ) ;
#22857 = ORIENTED_EDGE ( 'NONE', *, *, #30811, .F. ) ;
#22858 = LINE ( 'NONE', #18978, #30450 ) ;
#22859 = ORIENTED_EDGE ( 'NONE', *, *, #15438, .F. ) ;
#22860 = FACE_BOUND ( 'NONE', #37484, .T. ) ;
#22861 = EDGE_CURVE ( 'NONE', #31043, #9429, #36173, .T. ) ;
#22862 = CARTESIAN_POINT ( 'NONE',  ( -1.695772546416001836, 1.594396608463251486, -2.417756147381374010 ) ) ;
#22863 = DIRECTION ( 'NONE',  ( 8.902872254219889125E-17, 1.000000000000000000, 9.311674343991287120E-17 ) ) ;
#22864 = ORIENTED_EDGE ( 'NONE', *, *, #15529, .F. ) ;
#22865 = VERTEX_POINT ( 'NONE', #24033 ) ;
#22866 = CARTESIAN_POINT ( 'NONE',  ( 2.151753172350863164, 1.709557817375465305, -0.8661840175195394398 ) ) ;
#22867 = LINE ( 'NONE', #18235, #23781 ) ;
#22868 = EDGE_CURVE ( 'NONE', #11359, #10643, #2062, .T. ) ;
#22869 = CARTESIAN_POINT ( 'NONE',  ( 0.000000000000000000, 3.267716535433071279, 0.4330708661417290162 ) ) ;
#22870 = CARTESIAN_POINT ( 'NONE',  ( 1.636583440222563857, 0.000000000000000000, -0.1968503937007886062 ) ) ;
#22871 = CARTESIAN_POINT ( 'NONE',  ( 0.000000000000000000, 3.346456692913386100, 0.000000000000000000 ) ) ;
#22872 = ADVANCED_FACE ( 'NONE', ( #800 ), #18575, .T. ) ;
#22873 = CARTESIAN_POINT ( 'NONE',  ( -0.8942052331142552601, 3.267716535433071279, -1.141732283464563569 ) ) ;
#22874 = ORIENTED_EDGE ( 'NONE', *, *, #3519, .F. ) ;
#22875 = CARTESIAN_POINT ( 'NONE',  ( -1.166969139818016199, 3.267716535433071279, -0.3543307086614174151 ) ) ;
#22876 = CARTESIAN_POINT ( 'NONE',  ( -1.330241805570659519, 1.620978897557992404, -1.747195297779411627 ) ) ;
#22877 = CIRCLE ( 'NONE', #32772, 1.850107469027523432 ) ;
#22878 = VECTOR ( 'NONE', #17587, 39.37007874015748143 ) ;
#22879 = PLANE ( 'NONE',  #28128 ) ;
#22880 = VECTOR ( 'NONE', #30084, 39.37007874015748143 ) ;
#22881 = ORIENTED_EDGE ( 'NONE', *, *, #27201, .T. ) ;
#22882 = PLANE ( 'NONE',  #15835 ) ;
#22883 = VERTEX_POINT ( 'NONE', #279 ) ;
#22884 = VERTEX_POINT ( 'NONE', #39526 ) ;
#22885 = ADVANCED_FACE ( 'NONE', ( #28408 ), #8030, .F. ) ;
#22886 = B_SPLINE_CURVE_WITH_KNOTS ( 'NONE', 3,
 ( #17655, #33160, #41157, #48844 ),
 .UNSPECIFIED., .F., .F.,
 ( 4, 4 ),
 ( 2.000077559038616695E-07, 0.002660951063790191386 ),
 .UNSPECIFIED. ) ;
#22887 = ORIENTED_EDGE ( 'NONE', *, *, #16524, .F. ) ;
#22888 = ORIENTED_EDGE ( 'NONE', *, *, #32930, .F. ) ;
#22889 = LINE ( 'NONE', #46351, #49115 ) ;
#22890 = EDGE_CURVE ( 'NONE', #47335, #48366, #50830, .T. ) ;
#22892 = DIRECTION ( 'NONE',  ( -0.000000000000000000, 1.000000000000000000, -0.000000000000000000 ) ) ;
#22891 = VECTOR ( 'NONE', #20553, 39.37007874015748143 ) ;
#22893 = CARTESIAN_POINT ( 'NONE',  ( 1.636583440222563635, 3.346456692913386100, -1.259842519685035800 ) ) ;
#22894 = LINE ( 'NONE', #11527, #27213 ) ;
#22895 = CARTESIAN_POINT ( 'NONE',  ( 0.000000000000000000, 6.692913385826772199, 0.000000000000000000 ) ) ;
#22896 = DIRECTION ( 'NONE',  ( 0.000000000000000000, 1.000000000000000000, 0.000000000000000000 ) ) ;
#22897 = VERTEX_POINT ( 'NONE', #15772 ) ;
#22898 = CARTESIAN_POINT ( 'NONE',  ( 0.2727639067037610499, 3.346456692913386100, 1.102362204724404160 ) ) ;
#22899 = LINE ( 'NONE', #4482, #10215 ) ;
#22900 = PLANE ( 'NONE',  #429 ) ;
#22901 = CARTESIAN_POINT ( 'NONE',  ( -1.363819533518803473, 0.000000000000000000, -0.1574803149606300023 ) ) ;
#22902 = ORIENTED_EDGE ( 'NONE', *, *, #12773, .F. ) ;
#22903 = DIRECTION ( 'NONE',  ( 1.000000000000000000, 0.000000000000000000, 0.000000000000000000 ) ) ;
#22904 = DIRECTION ( 'NONE',  ( -0.000000000000000000, 1.000000000000000000, -0.000000000000000000 ) ) ;
#22905 = ORIENTED_EDGE ( 'NONE', *, *, #18295, .T. ) ;
#22906 = LINE ( 'NONE', #27019, #47650 ) ;
#22907 = AXIS2_PLACEMENT_3D ( 'NONE', #21021, #36772, #45004 ) ;
#22908 = AXIS2_PLACEMENT_3D ( 'NONE', #32781, #48462, #9782 ) ;
#22909 = EDGE_CURVE ( 'NONE', #2752, #34446, #15528, .T. ) ;
#22910 = CARTESIAN_POINT ( 'NONE',  ( -1.091055626815042645, 3.267716535433071279, -1.141732283464563569 ) ) ;
#22911 = FACE_OUTER_BOUND ( 'NONE', #18603, .T. ) ;
#22912 = VERTEX_POINT ( 'NONE', #39781 ) ;
#22913 = LINE ( 'NONE', #14665, #49478 ) ;
#22914 = EDGE_CURVE ( 'NONE', #39080, #20810, #27638, .T. ) ;
#22915 = DIRECTION ( 'NONE',  ( -0.000000000000000000, 1.000000000000000000, -0.000000000000000000 ) ) ;
#22916 = CARTESIAN_POINT ( 'NONE',  ( -2.182111253630085290, 3.346456692913386100, 0.6299212598425164567 ) ) ;
#22917 = ADVANCED_FACE ( 'NONE', ( #4415 ), #43641, .F. ) ;
#22918 = PLANE ( 'NONE',  #37494 ) ;
#22919 = DIRECTION ( 'NONE',  ( -0.000000000000000000, 1.000000000000000000, -0.000000000000000000 ) ) ;
#22920 = VERTEX_POINT ( 'NONE', #24299 ) ;
#22921 = EDGE_CURVE ( 'NONE', #3036, #36717, #23779, .T. ) ;
#22922 = AXIS2_PLACEMENT_3D ( 'NONE', #725, #15702, #47413 ) ;
#22923 = DIRECTION ( 'NONE',  ( -0.9998717552508122886, -0.01601477604151181275, 0.000000000000000000 ) ) ;
#22924 = EDGE_LOOP ( 'NONE', ( #35761, #38712, #35436, #6904 ) ) ;
#22925 = ORIENTED_EDGE ( 'NONE', *, *, #42528, .F. ) ;
#22926 = CARTESIAN_POINT ( 'NONE',  ( -0.07591351300297333182, 3.267716535433071279, 0.1574803149606283648 ) ) ;
#22927 = VERTEX_POINT ( 'NONE', #8287 ) ;
#22928 = EDGE_CURVE ( 'NONE', #50789, #43058, #19888, .T. ) ;
#22929 = CARTESIAN_POINT ( 'NONE',  ( 0.000000000000000000, 3.346456692913386100, 0.000000000000000000 ) ) ;
#22930 = AXIS2_PLACEMENT_3D ( 'NONE', #32898, #21507, #29763 ) ;
#22931 = LINE ( 'NONE', #26796, #38414 ) ;
#22932 = ORIENTED_EDGE ( 'NONE', *, *, #11004, .T. ) ;
#22933 = EDGE_CURVE ( 'NONE', #14052, #2108, #35406, .T. ) ;
#22934 = CARTESIAN_POINT ( 'NONE',  ( -1.064142702668968932, 0.000000000000000000, -1.380941303491921346 ) ) ;
#22935 = CARTESIAN_POINT ( 'NONE',  ( 2.160407304981128984, 6.692913385826772199, -0.1462862061266579361 ) ) ;
#22936 = CARTESIAN_POINT ( 'NONE',  ( 0.2727639067037610499, 3.346456692913386100, 2.362204724409437961 ) ) ;
#22937 = ORIENTED_EDGE ( 'NONE', *, *, #36369, .T. ) ;
#22938 = ORIENTED_EDGE ( 'NONE', *, *, #15769, .T. ) ;
#22939 = DIRECTION ( 'NONE',  ( -3.986037398843765983E-20, -1.000000000000000000, -1.160734090543304660E-16 ) ) ;
#22940 = FACE_BOUND ( 'NONE', #43565, .T. ) ;
#22941 = ORIENTED_EDGE ( 'NONE', *, *, #20544, .T. ) ;
#22942 = EDGE_CURVE ( 'NONE', #5467, #9285, #40040, .T. ) ;
#22943 = FACE_OUTER_BOUND ( 'NONE', #48614, .T. ) ;
#22944 = VECTOR ( 'NONE', #10041, 39.37007874015748143 ) ;
#22945 = ORIENTED_EDGE ( 'NONE', *, *, #29240, .F. ) ;
#22946 = ORIENTED_EDGE ( 'NONE', *, *, #31777, .T. ) ;
#22947 = EDGE_CURVE ( 'NONE', #33248, #47415, #4530, .T. ) ;
#22948 = FACE_OUTER_BOUND ( 'NONE', #43542, .T. ) ;
#22949 = ADVANCED_FACE ( 'NONE', ( #7778 ), #13445, .F. ) ;
#22950 = DIRECTION ( 'NONE',  ( 0.01601477604151182663, -0.9998717552508123996, 0.000000000000000000 ) ) ;
#22951 = VERTEX_POINT ( 'NONE', #29702 ) ;
#22952 = AXIS2_PLACEMENT_3D ( 'NONE', #18192, #49637, #49390 ) ;
#22953 = LINE ( 'NONE', #14951, #20444 ) ;
#22954 = ORIENTED_EDGE ( 'NONE', *, *, #7689, .T. ) ;
#22955 = PLANE ( 'NONE',  #33481 ) ;
#22956 = FACE_OUTER_BOUND ( 'NONE', #47724, .T. ) ;
#22957 = AXIS2_PLACEMENT_3D ( 'NONE', #46504, #27155, #11173 ) ;
#22958 = CARTESIAN_POINT ( 'NONE',  ( 0.1067246931122726866, 0.02962905676920215767, 0.000000000000000000 ) ) ;
#22959 = AXIS2_PLACEMENT_3D ( 'NONE', #27259, #10762, #39143 ) ;
#22960 = ORIENTED_EDGE ( 'NONE', *, *, #26497, .T. ) ;
#22961 = EDGE_LOOP ( 'NONE', ( #4135, #40199, #16237, #8517 ) ) ;
#22962 = CARTESIAN_POINT ( 'NONE',  ( -1.693234526714950228, 0.000000000000000000, -0.4369479234249735167 ) ) ;
#22963 = LINE ( 'NONE', #43582, #39362 ) ;
#22964 = DIRECTION ( 'NONE',  ( -0.000000000000000000, 1.000000000000000000, -0.000000000000000000 ) ) ;
#22965 = CARTESIAN_POINT ( 'NONE',  ( 0.000000000000000000, 2.755905511811024056, 0.000000000000000000 ) ) ;
#22966 = CARTESIAN_POINT ( 'NONE',  ( 2.106197740627112402, 3.267716535433071279, 1.102362204724403938 ) ) ;
#22967 = VECTOR ( 'NONE', #29886, 39.37007874015748143 ) ;
#22968 = CARTESIAN_POINT ( 'NONE',  ( 0.1968503937007873017, 3.346456692913386100, -0.9448818897637765168 ) ) ;
#22969 = DIRECTION ( 'NONE',  ( 0.000000000000000000, 1.000000000000000000, 0.000000000000000000 ) ) ;
#22970 = VERTEX_POINT ( 'NONE', #44918 ) ;
#22971 = LINE ( 'NONE', #7233, #19266 ) ;
#22972 = DIRECTION ( 'NONE',  ( -0.01601477604151182663, 0.9998717552508123996, -0.000000000000000000 ) ) ;
#22973 = B_SPLINE_CURVE_WITH_KNOTS ( 'NONE', 3,
 ( #12422, #807, #8553, #40313 ),
 .UNSPECIFIED., .F., .F.,
 ( 4, 4 ),
 ( 4.780700947777823547E-07, 0.04951104265158085688 ),
 .UNSPECIFIED. ) ;
#22974 = ORIENTED_EDGE ( 'NONE', *, *, #19384, .T. ) ;
#22975 = EDGE_LOOP ( 'NONE', ( #49223, #39394, #16679, #21502, #13732, #21687, #11689, #333 ) ) ;
#22976 = PLANE ( 'NONE',  #47223 ) ;
#22977 = DIRECTION ( 'NONE',  ( -0.7660444431189771253, 0.6427876096865404731, -2.879229771426817147E-16 ) ) ;
#22978 = EDGE_CURVE ( 'NONE', #10179, #10605, #5702, .T. ) ;
#22979 = VECTOR ( 'NONE', #24963, 39.37007874015748143 ) ;
#22980 = ORIENTED_EDGE ( 'NONE', *, *, #48148, .T. ) ;
#22981 = EDGE_CURVE ( 'NONE', #6479, #48094, #45419, .T. ) ;
#22982 = EDGE_CURVE ( 'NONE', #28186, #25938, #17825, .T. ) ;
#22983 = CARTESIAN_POINT ( 'NONE',  ( -2.009930929872525418, 1.574803149606302854, -0.8055662819784117357 ) ) ;
#22984 = ORIENTED_EDGE ( 'NONE', *, *, #20311, .F. ) ;
#22985 = DIRECTION ( 'NONE',  ( -0.000000000000000000, 1.000000000000000000, -0.000000000000000000 ) ) ;
#22986 = ORIENTED_EDGE ( 'NONE', *, *, #29954, .F. ) ;
#22987 = AXIS2_PLACEMENT_3D ( 'NONE', #28194, #24847, #40082 ) ;
#22988 = AXIS2_PLACEMENT_3D ( 'NONE', #44118, #5662, #28888 ) ;
#22989 = CARTESIAN_POINT ( 'NONE',  ( -1.628069513120385503, 0.001843152681973240061, -0.6423508795876955446 ) ) ;
#22990 = DIRECTION ( 'NONE',  ( -0.9998717552508122886, -0.01601477604151180928, 0.000000000000000000 ) ) ;
#22991 = AXIS2_PLACEMENT_3D ( 'NONE', #17570, #44154, #5177 ) ;
#22992 = ORIENTED_EDGE ( 'NONE', *, *, #11063, .T. ) ;
#22993 = CARTESIAN_POINT ( 'NONE',  ( 0.08119777152254364916, 1.623385212329073957, 0.000000000000000000 ) ) ;
#22994 = ORIENTED_EDGE ( 'NONE', *, *, #33311, .F. ) ;
#22995 = EDGE_LOOP ( 'NONE', ( #228, #12223, #8418, #42027 ) ) ;
#22996 = DIRECTION ( 'NONE',  ( -0.000000000000000000, 1.000000000000000000, -0.000000000000000000 ) ) ;
#22997 = CARTESIAN_POINT ( 'NONE',  ( -0.8783128861146038968, 0.01385187720497466773, 1.565997986929510644 ) ) ;
#22998 = CARTESIAN_POINT ( 'NONE',  ( 0.000000000000000000, 6.692913385826772199, 0.000000000000000000 ) ) ;
#22999 = EDGE_CURVE ( 'NONE', #32548, #8583, #9571, .T. ) ;
#23000 = AXIS2_PLACEMENT_3D ( 'NONE', #9133, #36255, #19968 ) ;
#23001 = ORIENTED_EDGE ( 'NONE', *, *, #36053, .T. ) ;
#23002 = EDGE_CURVE ( 'NONE', #42568, #21081, #28670, .T. ) ;
#23003 = CARTESIAN_POINT ( 'NONE',  ( -2.182111253630085290, 0.000000000000000000, 0.1181102362204704270 ) ) ;
#23004 = CARTESIAN_POINT ( 'NONE',  ( 2.889674983507178219, 2.755905511811027164, -0.6090712660037607140 ) ) ;
#23005 = ORIENTED_EDGE ( 'NONE', *, *, #32989, .T. ) ;
#23006 = EDGE_CURVE ( 'NONE', #4010, #26232, #396, .T. ) ;
#23007 = LINE ( 'NONE', #38756, #28164 ) ;
#23008 = ADVANCED_FACE ( 'NONE', ( #25312 ), #17322, .F. ) ;
#23009 = EDGE_LOOP ( 'NONE', ( #29025, #38320, #24012, #29868 ) ) ;
#23010 = ORIENTED_EDGE ( 'NONE', *, *, #15135, .F. ) ;
#23011 = CARTESIAN_POINT ( 'NONE',  ( 2.372302221414760215, 29.20466208540896602, 74.87852387875602744 ) ) ;
#23012 = VERTEX_POINT ( 'NONE', #20669 ) ;
#23013 = DIRECTION ( 'NONE',  ( -0.000000000000000000, 1.000000000000000000, -0.000000000000000000 ) ) ;
#23014 = CARTESIAN_POINT ( 'NONE',  ( 0.8182917201112819283, 0.000000000000000000, -0.3543307086614175816 ) ) ;
#23015 = CIRCLE ( 'NONE', #26337, 2.246510896728926010 ) ;
#23016 = CARTESIAN_POINT ( 'NONE',  ( 0.5786196242795136335, 3.346456692913386100, -2.086614173228340086 ) ) ;
#23017 = PLANE ( 'NONE',  #2437 ) ;
#23018 = EDGE_LOOP ( 'NONE', ( #11624, #39138, #24298, #18801 ) ) ;
#23019 = EDGE_LOOP ( 'NONE', ( #39650, #5460, #20138, #18837 ) ) ;
#23020 = CARTESIAN_POINT ( 'NONE',  ( 1.363819533518803251, 3.346456692913386100, -0.6692913385826764205 ) ) ;
#23021 = ORIENTED_EDGE ( 'NONE', *, *, #35117, .F. ) ;
#23022 = DIRECTION ( 'NONE',  ( -1.000000000000000000, 0.000000000000000000, 0.000000000000000000 ) ) ;
#23023 = CARTESIAN_POINT ( 'NONE',  ( 1.695772546416036919, 1.205361022782829114E-17, -2.417756147381349141 ) ) ;
#23024 = VECTOR ( 'NONE', #34705, 39.37007874015748143 ) ;
#23025 = AXIS2_PLACEMENT_3D ( 'NONE', #33483, #9205, #45560 ) ;
#23026 = CARTESIAN_POINT ( 'NONE',  ( -1.363819533518803473, 3.346456692913386100, -0.4724409448818886470 ) ) ;
#23027 = DIRECTION ( 'NONE',  ( 1.000000000000000000, 0.000000000000000000, 0.000000000000000000 ) ) ;
#23028 = CARTESIAN_POINT ( 'NONE',  ( 0.000000000000000000, 0.000000000000000000, 0.000000000000000000 ) ) ;
#23029 = ORIENTED_EDGE ( 'NONE', *, *, #29099, .T. ) ;
#23030 = DIRECTION ( 'NONE',  ( -0.000000000000000000, 1.000000000000000000, -0.000000000000000000 ) ) ;
#23031 = DIRECTION ( 'NONE',  ( -0.01601477604151182663, 0.9998717552508123996, -0.000000000000000000 ) ) ;
#23032 = VECTOR ( 'NONE', #1064, 39.37007874015748143 ) ;
#23033 = ORIENTED_EDGE ( 'NONE', *, *, #47137, .F. ) ;
#23034 = CARTESIAN_POINT ( 'NONE',  ( 0.000000000000000000, 1.574803149606302854, 0.000000000000000000 ) ) ;
#23035 = CARTESIAN_POINT ( 'NONE',  ( -1.688048600224982154, 0.000000000000000000, -0.4357642695449713277 ) ) ;
#23036 = DIRECTION ( 'NONE',  ( 0.000000000000000000, 1.000000000000000000, 0.000000000000000000 ) ) ;
#23037 = VERTEX_POINT ( 'NONE', #29446 ) ;
#23038 = B_SPLINE_CURVE_WITH_KNOTS ( 'NONE', 3,
 ( #45577, #6873, #49435, #18239 ),
 .UNSPECIFIED., .F., .F.,
 ( 4, 4 ),
 ( 0.0005868951926194780231, 0.04882122509610800631 ),
 .UNSPECIFIED. ) ;
#23039 = PLANE ( 'NONE',  #43204 ) ;
#23040 = ADVANCED_FACE ( 'NONE', ( #13703 ), #33593, .F. ) ;
#23041 = EDGE_CURVE ( 'NONE', #47517, #37178, #1819, .T. ) ;
#23042 = EDGE_LOOP ( 'NONE', ( #14208, #12577, #16000 ) ) ;
#23043 = CARTESIAN_POINT ( 'NONE',  ( 0.2727639067037604392, 0.000000000000000000, -0.9842519685039348154 ) ) ;
#23044 = ORIENTED_EDGE ( 'NONE', *, *, #4158, .T. ) ;
#23045 = LINE ( 'NONE', #47250, #10568 ) ;
#23046 = EDGE_CURVE ( 'NONE', #29367, #17250, #37462, .T. ) ;
#23047 = ORIENTED_EDGE ( 'NONE', *, *, #7495, .F. ) ;
#23048 = DIRECTION ( 'NONE',  ( 0.8090169943749507819, -1.160734090543304660E-16, -0.5877852522924685852 ) ) ;
#23049 = DIRECTION ( 'NONE',  ( -0.000000000000000000, -1.000000000000000000, -0.000000000000000000 ) ) ;
#23050 = DIRECTION ( 'NONE',  ( 0.000000000000000000, -1.000000000000000000, 0.000000000000000000 ) ) ;
#23051 = VECTOR ( 'NONE', #28520, 39.37007874015748143 ) ;
#23052 = EDGE_LOOP ( 'NONE', ( #44363, #29724, #6638, #45286 ) ) ;
#23053 = ORIENTED_EDGE ( 'NONE', *, *, #35855, .T. ) ;
#23054 = ORIENTED_EDGE ( 'NONE', *, *, #38188, .T. ) ;
#23055 = CARTESIAN_POINT ( 'NONE',  ( 1.139183960333101098, 3.346456692913386100, -1.771653543307081691 ) ) ;
#23056 = DIRECTION ( 'NONE',  ( -1.000000000000000000, 0.000000000000000000, -0.000000000000000000 ) ) ;
#23057 = ORIENTED_EDGE ( 'NONE', *, *, #49068, .T. ) ;
#23058 = EDGE_LOOP ( 'NONE', ( #27289, #41974, #36293, #12854 ) ) ;
#23059 = DIRECTION ( 'NONE',  ( -0.9998717552508121775, -0.01601477604151182316, 0.000000000000000000 ) ) ;
#23060 = CARTESIAN_POINT ( 'NONE',  ( -0.8182917201112819283, 3.346456692913386100, -0.9842519685039342603 ) ) ;
#23061 = CARTESIAN_POINT ( 'NONE',  ( 2.505971853429350471, 0.9863260818638780458, 0.7624944251838070564 ) ) ;
#23062 = AXIS2_PLACEMENT_3D ( 'NONE', #28663, #48504, #5173 ) ;
#23063 = ORIENTED_EDGE ( 'NONE', *, *, #24368, .F. ) ;
#23064 = B_SPLINE_CURVE_WITH_KNOTS ( 'NONE', 3,
 ( #8688, #24444, #35803, #48147 ),
 .UNSPECIFIED., .F., .F.,
 ( 4, 4 ),
 ( 0.001375932973688854437, 0.003876164346139760603 ),
 .UNSPECIFIED. ) ;
#23065 = ORIENTED_EDGE ( 'NONE', *, *, #4640, .T. ) ;
#23066 = ADVANCED_FACE ( 'NONE', ( #49280 ), #28927, .F. ) ;
#23067 = PLANE ( 'NONE',  #732 ) ;
#23068 = CARTESIAN_POINT ( 'NONE',  ( 2.106197740627111514, 3.267716535433070391, -1.239052911296964155 ) ) ;
#23069 = CARTESIAN_POINT ( 'NONE',  ( -2.182111253630085290, 3.346456692913386100, 0.6299212598425164567 ) ) ;
#23070 = ORIENTED_EDGE ( 'NONE', *, *, #50857, .F. ) ;
#23071 = CARTESIAN_POINT ( 'NONE',  ( -1.478474649365228100, 1.688261849119575997, -1.951220303998286054 ) ) ;
#23072 = DIRECTION ( 'NONE',  ( 1.000000000000000000, 0.000000000000000000, 0.000000000000000000 ) ) ;
#23073 = ORIENTED_EDGE ( 'NONE', *, *, #11737, .F. ) ;
#23074 = EDGE_CURVE ( 'NONE', #39080, #50597, #40815, .T. ) ;
#23075 = CARTESIAN_POINT ( 'NONE',  ( -1.083598637574820334, 1.538470290252458739, 2.747180975113330259 ) ) ;
#23076 = ORIENTED_EDGE ( 'NONE', *, *, #50588, .T. ) ;
#23077 = EDGE_LOOP ( 'NONE', ( #14534, #25307, #17872, #50565 ) ) ;
#23078 = AXIS2_PLACEMENT_3D ( 'NONE', #22237, #2607, #26849 ) ;
#23079 = CARTESIAN_POINT ( 'NONE',  ( 0.5110594979943910987, 0.000000000000000000, -1.666798357583575418 ) ) ;
#23080 = FACE_OUTER_BOUND ( 'NONE', #40841, .T. ) ;
#23081 = CARTESIAN_POINT ( 'NONE',  ( 0.000000000000000000, 1.574803149606302854, 0.000000000000000000 ) ) ;
#23082 = CARTESIAN_POINT ( 'NONE',  ( -1.083598637574820112, 0.000000000000000000, 2.747180975113330259 ) ) ;
#23083 = LINE ( 'NONE', #10957, #50174 ) ;
#23084 = ORIENTED_EDGE ( 'NONE', *, *, #12964, .T. ) ;
#23085 = VERTEX_POINT ( 'NONE', #17070 ) ;
#23086 = DIRECTION ( 'NONE',  ( -3.469446951953613696E-16, 0.000000000000000000, -1.000000000000000000 ) ) ;
#23087 = LINE ( 'NONE', #11219, #9439 ) ;
#23088 = CARTESIAN_POINT ( 'NONE',  ( -0.8182917201112819283, 0.000000000000000000, 2.047244094488179567 ) ) ;
#23089 = LINE ( 'NONE', #50903, #19590 ) ;
#23090 = ORIENTED_EDGE ( 'NONE', *, *, #40231, .F. ) ;
#23091 = DIRECTION ( 'NONE',  ( -3.469446951953613696E-16, 0.000000000000000000, -1.000000000000000000 ) ) ;
#23092 = CARTESIAN_POINT ( 'NONE',  ( -2.182111253630085290, 0.000000000000000000, -6.146657985744592735E-16 ) ) ;
#23093 = CONICAL_SURFACE ( 'NONE', #50245, 1.850107469027523210, 0.6386652850508578450 ) ;
#23094 = VERTEX_POINT ( 'NONE', #44661 ) ;
#23095 = DIRECTION ( 'NONE',  ( 1.000000000000000000, 0.000000000000000000, 0.000000000000000000 ) ) ;
#23096 = VECTOR ( 'NONE', #34702, 39.37007874015748143 ) ;
#23097 = FACE_OUTER_BOUND ( 'NONE', #43706, .T. ) ;
#23098 = CARTESIAN_POINT ( 'NONE',  ( -1.636583440222563635, 0.000000000000000000, 0.6299212598425164567 ) ) ;
#23099 = DIRECTION ( 'NONE',  ( -3.469446951953613696E-16, 0.000000000000000000, -1.000000000000000000 ) ) ;
#23100 = DIRECTION ( 'NONE',  ( -0.01601477604151182663, 0.9998717552508123996, -0.000000000000000000 ) ) ;
#23101 = DIRECTION ( 'NONE',  ( 0.000000000000000000, 0.000000000000000000, -1.000000000000000000 ) ) ;
#23102 = EDGE_CURVE ( 'NONE', #46376, #34365, #32566, .T. ) ;
#23103 = ADVANCED_FACE ( 'NONE', ( #48255 ), #12941, .F. ) ;
#23104 = ORIENTED_EDGE ( 'NONE', *, *, #14425, .F. ) ;
#23105 = LINE ( 'NONE', #10982, #9028 ) ;
#23106 = AXIS2_PLACEMENT_3D ( 'NONE', #20115, #11614, #8513 ) ;
#23107 = ORIENTED_EDGE ( 'NONE', *, *, #9468, .F. ) ;
#23108 = CARTESIAN_POINT ( 'NONE',  ( -2.182111253630085734, 0.000000000000000000, -0.6299212598425177889 ) ) ;
#23109 = EDGE_CURVE ( 'NONE', #3300, #18896, #32832, .T. ) ;
#23110 = DIRECTION ( 'NONE',  ( -0.000000000000000000, 1.000000000000000000, -0.000000000000000000 ) ) ;
#23111 = DIRECTION ( 'NONE',  ( -0.000000000000000000, 1.000000000000000000, -0.000000000000000000 ) ) ;
#23112 = EDGE_CURVE ( 'NONE', #33027, #11117, #2904, .T. ) ;
#23113 = VERTEX_POINT ( 'NONE', #45669 ) ;
#23114 = ORIENTED_EDGE ( 'NONE', *, *, #44134, .F. ) ;
#23115 = DIRECTION ( 'NONE',  ( -1.000000000000000000, -0.000000000000000000, -0.000000000000000000 ) ) ;
#23116 = CARTESIAN_POINT ( 'NONE',  ( 1.018961996185594021, 0.04424020667788951949, 1.609505285524495344 ) ) ;
#23117 = CARTESIAN_POINT ( 'NONE',  ( 0.9914495361338625523, 1.636256239573039117, 2.781765111341823360 ) ) ;
#23118 = DIRECTION ( 'NONE',  ( 0.000000000000000000, 0.000000000000000000, -1.000000000000000000 ) ) ;
#23119 = CARTESIAN_POINT ( 'NONE',  ( -1.636583440222564301, 3.346456692913386100, -0.8267716535433052849 ) ) ;
#23120 = CARTESIAN_POINT ( 'NONE',  ( 2.623503965249848857, 5.905511811023623991, 1.355882097269874187 ) ) ;
#23121 = ORIENTED_EDGE ( 'NONE', *, *, #17277, .F. ) ;
#23122 = EDGE_CURVE ( 'NONE', #45841, #23012, #31972, .T. ) ;
#23123 = CARTESIAN_POINT ( 'NONE',  ( 0.5455278134075216556, 3.267716535433071279, 1.377952755905504256 ) ) ;
#23124 = LINE ( 'NONE', #34256, #43901 ) ;
#23125 = FACE_OUTER_BOUND ( 'NONE', #16157, .T. ) ;
#23126 = ORIENTED_EDGE ( 'NONE', *, *, #1820, .F. ) ;
#23127 = EDGE_CURVE ( 'NONE', #20592, #50824, #20166, .T. ) ;
#23128 = CARTESIAN_POINT ( 'NONE',  ( -0.5286458662987738588, 5.905511811023623991, 2.100489422084708124 ) ) ;
#23129 = ORIENTED_EDGE ( 'NONE', *, *, #48372, .F. ) ;
#23130 = ORIENTED_EDGE ( 'NONE', *, *, #48040, .T. ) ;
#23131 = AXIS2_PLACEMENT_3D ( 'NONE', #2537, #50474, #18282 ) ;
#23132 = B_SPLINE_CURVE_WITH_KNOTS ( 'NONE', 3,
 ( #50207, #30900, #11277, #49960 ),
 .UNSPECIFIED., .F., .F.,
 ( 4, 4 ),
 ( 0.001826648268129119979, 0.004326648414133393156 ),
 .UNSPECIFIED. ) ;
#23133 = ADVANCED_FACE ( 'NONE', ( #6468 ), #3092, .F. ) ;
#23134 = EDGE_LOOP ( 'NONE', ( #40777, #14961, #20082, #31966 ) ) ;
#23135 = ORIENTED_EDGE ( 'NONE', *, *, #10755, .T. ) ;
#23136 = CARTESIAN_POINT ( 'NONE',  ( 1.909347346926324684, 3.346456692913386100, -0.6692913385826764205 ) ) ;
#23137 = VECTOR ( 'NONE', #22370, 39.37007874015748143 ) ;
#23138 = CARTESIAN_POINT ( 'NONE',  ( 2.240374965981713817, 0.5220472870780150654, -0.4608727740821708108 ) ) ;
#23139 = EDGE_CURVE ( 'NONE', #2113, #34134, #46113, .T. ) ;
#23140 = DIRECTION ( 'NONE',  ( -3.469446951953613696E-16, 0.000000000000000000, -1.000000000000000000 ) ) ;
#23141 = CARTESIAN_POINT ( 'NONE',  ( 2.122871581070786995, 0.000000000000000000, 0.2710165112059633730 ) ) ;
#23142 = DIRECTION ( 'NONE',  ( -0.000000000000000000, 0.000000000000000000, 1.000000000000000000 ) ) ;
#23143 = CARTESIAN_POINT ( 'NONE',  ( 0.000000000000000000, 3.267716535433071279, 0.6299212598425164567 ) ) ;
#23144 = FACE_OUTER_BOUND ( 'NONE', #45386, .T. ) ;
#23145 = ORIENTED_EDGE ( 'NONE', *, *, #41835, .F. ) ;
#23146 = DIRECTION ( 'NONE',  ( -3.758567531283081874E-16, 0.000000000000000000, 1.000000000000000000 ) ) ;
#23147 = CARTESIAN_POINT ( 'NONE',  ( 0.4696143004045478797, 3.267716535433071279, -1.629301903132387260E-16 ) ) ;
#23148 = CARTESIAN_POINT ( 'NONE',  ( -0.6214413264104939882, 0.000000000000000000, 1.417322834645662777 ) ) ;
#23149 = CARTESIAN_POINT ( 'NONE',  ( 1.838947341486932396, 0.05737377265108637575, 0.6492553997849701553 ) ) ;
#23150 = B_SPLINE_CURVE_WITH_KNOTS ( 'NONE', 3,
 ( #36471, #28195, #4718, #1088 ),
 .UNSPECIFIED., .F., .F.,
 ( 4, 4 ),
 ( 0.01072160763121544902, 0.03070979195761600056 ),
 .UNSPECIFIED. ) ;
#23151 = ORIENTED_EDGE ( 'NONE', *, *, #14977, .F. ) ;
#23152 = PLANE ( 'NONE',  #14122 ) ;
#23153 = CARTESIAN_POINT ( 'NONE',  ( 1.560669927219590525, 0.000000000000000000, -0.3543307086614178592 ) ) ;
#23154 = EDGE_LOOP ( 'NONE', ( #28056, #10004, #6811, #316 ) ) ;
#23155 = DIRECTION ( 'NONE',  ( -1.000000000000000000, 0.000000000000000000, 1.734723475976806848E-16 ) ) ;
#23156 = PLANE ( 'NONE',  #25101 ) ;
#23157 = CARTESIAN_POINT ( 'NONE',  ( 2.164658444855302122, 5.905511811023623991, -0.04795272066889885720 ) ) ;
#23158 = ORIENTED_EDGE ( 'NONE', *, *, #13159, .F. ) ;
#23159 = CARTESIAN_POINT ( 'NONE',  ( -1.001904449526793695, 1.691854617476330036, -1.967052558704270426 ) ) ;
#23160 = EDGE_CURVE ( 'NONE', #16446, #40209, #49525, .T. ) ;
#23161 = CYLINDRICAL_SURFACE ( 'NONE', #7727, 2.165354330708661568 ) ;
#23162 = AXIS2_PLACEMENT_3D ( 'NONE', #6970, #46924, #46677 ) ;
#23163 = VECTOR ( 'NONE', #21476, 39.37007874015748143 ) ;
#23164 = CARTESIAN_POINT ( 'NONE',  ( -0.6235241006192322466, 1.205361022782829114E-17, 2.074304693190349269 ) ) ;
#23166 = EDGE_CURVE ( 'NONE', #9666, #46382, #46176, .T. ) ;
#23165 = CARTESIAN_POINT ( 'NONE',  ( 1.363819533518803251, 3.267716535433071279, 0.9055118110236164419 ) ) ;
#23167 = VERTEX_POINT ( 'NONE', #2586 ) ;
#23168 = EDGE_CURVE ( 'NONE', #26808, #24752, #50031, .T. ) ;
#23169 = EDGE_LOOP ( 'NONE', ( #34598, #37596, #19388, #19412 ) ) ;
#23170 = VERTEX_POINT ( 'NONE', #19081 ) ;
#23171 = CARTESIAN_POINT ( 'NONE',  ( 0.000000000000000000, 3.267716535433071279, -0.6692913385826764205 ) ) ;
#23172 = ORIENTED_EDGE ( 'NONE', *, *, #19083, .T. ) ;
#23173 = DIRECTION ( 'NONE',  ( -3.469446951953613696E-16, 0.000000000000000000, -1.000000000000000000 ) ) ;
#23174 = VECTOR ( 'NONE', #16262, 39.37007874015748143 ) ;
#23175 = PLANE ( 'NONE',  #30192 ) ;
#23176 = VERTEX_POINT ( 'NONE', #41831 ) ;
#23177 = PLANE ( 'NONE',  #25578 ) ;
#23178 = VECTOR ( 'NONE', #15664, 39.37007874015748143 ) ;
#23179 = ORIENTED_EDGE ( 'NONE', *, *, #41357, .T. ) ;
#23180 = FACE_OUTER_BOUND ( 'NONE', #28936, .T. ) ;
#23181 = VERTEX_POINT ( 'NONE', #34089 ) ;
#23182 = ORIENTED_EDGE ( 'NONE', *, *, #8048, .T. ) ;
#23183 = LINE ( 'NONE', #43560, #15791 ) ;
#23184 = EDGE_LOOP ( 'NONE', ( #14198, #39230, #937, #11664 ) ) ;
#23185 = DIRECTION ( 'NONE',  ( -0.000000000000000000, 1.000000000000000000, -0.000000000000000000 ) ) ;
#23186 = ADVANCED_FACE ( 'NONE', ( #50276 ), #49779, .T. ) ;
#23187 = VERTEX_POINT ( 'NONE', #50522 ) ;
#23188 = ORIENTED_EDGE ( 'NONE', *, *, #41443, .T. ) ;
#23189 = CARTESIAN_POINT ( 'NONE',  ( -0.3486774197067340486, 3.267716535433071279, -1.141732283464563791 ) ) ;
#23190 = DIRECTION ( 'NONE',  ( -1.105928667600727183E-16, 1.000000000000000000, 6.607616187506045307E-17 ) ) ;
#23191 = EDGE_LOOP ( 'NONE', ( #13041, #18659, #9039, #1095 ) ) ;
#23192 = DIRECTION ( 'NONE',  ( 0.000000000000000000, -1.000000000000000000, 0.000000000000000000 ) ) ;
#23193 = EDGE_CURVE ( 'NONE', #21920, #32010, #14968, .T. ) ;
#23194 = ORIENTED_EDGE ( 'NONE', *, *, #8905, .F. ) ;
#23195 = CARTESIAN_POINT ( 'NONE',  ( 0.000000000000000000, 3.346456692913386100, 0.000000000000000000 ) ) ;
#23196 = VECTOR ( 'NONE', #36885, 39.37007874015748143 ) ;
#23197 = FACE_OUTER_BOUND ( 'NONE', #34953, .T. ) ;
#23198 = VECTOR ( 'NONE', #24408, 39.37007874015748143 ) ;
#23199 = ADVANCED_FACE ( 'NONE', ( #42580 ), #31758, .T. ) ;
#23200 = CARTESIAN_POINT ( 'NONE',  ( -1.166969139818015755, 3.346456692913386100, 0.9055118110236167750 ) ) ;
#23201 = ORIENTED_EDGE ( 'NONE', *, *, #1881, .F. ) ;
#23202 = ORIENTED_EDGE ( 'NONE', *, *, #12545, .T. ) ;
#23203 = CIRCLE ( 'NONE', #48745, 1.743387098533651480 ) ;
#23204 = DIRECTION ( 'NONE',  ( 0.000000000000000000, 0.000000000000000000, -1.000000000000000000 ) ) ;
#23205 = PLANE ( 'NONE',  #31226 ) ;
#23206 = CARTESIAN_POINT ( 'NONE',  ( -1.675814739737315540, 1.582635513994296250, 1.399362935606387470 ) ) ;
#23207 = EDGE_CURVE ( 'NONE', #11574, #41494, #10837, .T. ) ;
#23208 = AXIS2_PLACEMENT_3D ( 'NONE', #22381, #6119, #25996 ) ;
#23209 = FACE_OUTER_BOUND ( 'NONE', #25706, .T. ) ;
#23210 = EDGE_CURVE ( 'NONE', #9920, #3300, #39371, .T. ) ;
#23211 = CARTESIAN_POINT ( 'NONE',  ( 0.8182917201112824834, 0.000000000000000000, 1.732283464566921172 ) ) ;
#23212 = VECTOR ( 'NONE', #11982, 39.37007874015748143 ) ;
#23213 = CARTESIAN_POINT ( 'NONE',  ( 1.097585813245683717, 0.5905511811023621549, 0.9794755770252102645 ) ) ;
#23214 = CARTESIAN_POINT ( 'NONE',  ( -2.159905143290285601, 5.905511811023623991, 0.1535224723189611284 ) ) ;
#23215 = B_SPLINE_CURVE_WITH_KNOTS ( 'NONE', 3,
 ( #46332, #10994, #7126, #38866 ),
 .UNSPECIFIED., .F., .F.,
 ( 4, 4 ),
 ( 0.1211873102087489551, 0.1625992483279400380 ),
 .UNSPECIFIED. ) ;
#23216 = ORIENTED_EDGE ( 'NONE', *, *, #32381, .T. ) ;
#23217 = LINE ( 'NONE', #227, #39106 ) ;
#23218 = VERTEX_POINT ( 'NONE', #46424 ) ;
#23220 = ADVANCED_FACE ( 'NONE', ( #34345 ), #22714, .F. ) ;
#23219 = ORIENTED_EDGE ( 'NONE', *, *, #37018, .T. ) ;
#23221 = CARTESIAN_POINT ( 'NONE',  ( -1.985260859929297794, 3.346456692913386100, 0.1181102362204704270 ) ) ;
#23222 = LINE ( 'NONE', #45681, #3926 ) ;
#23223 = ORIENTED_EDGE ( 'NONE', *, *, #47263, .T. ) ;
#23224 = ADVANCED_FACE ( 'NONE', ( #30966 ), #7227, .T. ) ;
#23225 = EDGE_CURVE ( 'NONE', #13914, #49472, #6211, .T. ) ;
#23226 = DIRECTION ( 'NONE',  ( 0.01601477604151182663, -0.9998717552508123996, 0.000000000000000000 ) ) ;
#23227 = VERTEX_POINT ( 'NONE', #23975 ) ;
#23228 = CARTESIAN_POINT ( 'NONE',  ( -0.9149808212874269708, 1.594821661612501940, -2.013400720915880626 ) ) ;
#23229 = ORIENTED_EDGE ( 'NONE', *, *, #21643, .T. ) ;
#23230 = VECTOR ( 'NONE', #5000, 39.37007874015748143 ) ;
#23231 = CARTESIAN_POINT ( 'NONE',  ( 1.325491792074624087, 1.739919523179865202, -2.638988599164732385 ) ) ;
#23232 = DIRECTION ( 'NONE',  ( -3.986037398843765983E-20, -1.000000000000000000, -1.160734090543304660E-16 ) ) ;
#23233 = AXIS2_PLACEMENT_3D ( 'NONE', #31325, #31577, #47279 ) ;
#23234 = ORIENTED_EDGE ( 'NONE', *, *, #3357, .T. ) ;
#23235 = VECTOR ( 'NONE', #11566, 39.37007874015748143 ) ;
#23236 = CARTESIAN_POINT ( 'NONE',  ( -1.439733046521776139, 3.346456692913386100, -4.780733988912460139E-16 ) ) ;
#23237 = ORIENTED_EDGE ( 'NONE', *, *, #37539, .T. ) ;
#23238 = ORIENTED_EDGE ( 'NONE', *, *, #16107, .F. ) ;
#23239 = DIRECTION ( 'NONE',  ( -0.000000000000000000, 1.000000000000000000, -0.000000000000000000 ) ) ;
#23240 = DIRECTION ( 'NONE',  ( -1.000000000000000000, -0.000000000000000000, -0.000000000000000000 ) ) ;
#23241 = CARTESIAN_POINT ( 'NONE',  ( 0.5455278134075212115, 3.346456692913386100, -0.9448818897637765168 ) ) ;
#23242 = AXIS2_PLACEMENT_3D ( 'NONE', #49169, #9970, #22104 ) ;
#23243 = EDGE_LOOP ( 'NONE', ( #26844, #20630, #44011, #29739 ) ) ;
#23244 = DIRECTION ( 'NONE',  ( 1.734723475976806848E-16, -0.000000000000000000, 1.000000000000000000 ) ) ;
#23245 = DIRECTION ( 'NONE',  ( -0.000000000000000000, 1.000000000000000000, -0.000000000000000000 ) ) ;
#23246 = EDGE_CURVE ( 'NONE', #38330, #33353, #38961, .T. ) ;
#23247 = VERTEX_POINT ( 'NONE', #36113 ) ;
#23248 = LINE ( 'NONE', #43369, #30692 ) ;
#23249 = ORIENTED_EDGE ( 'NONE', *, *, #35135, .T. ) ;
#23250 = ORIENTED_EDGE ( 'NONE', *, *, #30629, .F. ) ;
#23251 = DIRECTION ( 'NONE',  ( -0.8184814127304661513, 0.2728986718806659661, -0.5055833184555330595 ) ) ;
#23252 = EDGE_CURVE ( 'NONE', #15892, #36336, #745, .T. ) ;
#23253 = VERTEX_POINT ( 'NONE', #220 ) ;
#23254 = FACE_OUTER_BOUND ( 'NONE', #3955, .T. ) ;
#23255 = LINE ( 'NONE', #31271, #35710 ) ;
#23256 = ADVANCED_FACE ( 'NONE', ( #23209 ), #11344, .F. ) ;
#23257 = ADVANCED_FACE ( 'NONE', ( #23457 ), #3595, .F. ) ;
#23258 = DIRECTION ( 'NONE',  ( -3.469446951953613696E-16, 0.000000000000000000, -1.000000000000000000 ) ) ;
#23259 = DIRECTION ( 'NONE',  ( -0.000000000000000000, 1.000000000000000000, -0.000000000000000000 ) ) ;
#23260 = VERTEX_POINT ( 'NONE', #43070 ) ;
#23261 = ORIENTED_EDGE ( 'NONE', *, *, #21192, .T. ) ;
#23262 =( LENGTH_UNIT ( ) NAMED_UNIT ( * ) SI_UNIT ( $, .METRE. ) );
#23263 = LINE ( 'NONE', #276, #19329 ) ;
#23264 = ORIENTED_EDGE ( 'NONE', *, *, #5359, .F. ) ;
#23265 = DIRECTION ( 'NONE',  ( 1.734723475976806848E-16, -0.000000000000000000, 1.000000000000000000 ) ) ;
#23266 = DIRECTION ( 'NONE',  ( -1.000000000000000000, 0.000000000000000000, -0.000000000000000000 ) ) ;
#23267 = VECTOR ( 'NONE', #27059, 39.37007874015748143 ) ;
#23268 = EDGE_CURVE ( 'NONE', #42285, #4915, #19580, .T. ) ;
#23269 = LINE ( 'NONE', #50831, #47228 ) ;
#23270 = CARTESIAN_POINT ( 'NONE',  ( -1.091055626815042645, 0.000000000000000000, -1.889763779527552146 ) ) ;
#23272 = CARTESIAN_POINT ( 'NONE',  ( 0.7423782071083092626, 0.000000000000000000, 1.259842519685033357 ) ) ;
#23271 = AXIS2_PLACEMENT_3D ( 'NONE', #37621, #9740, #45579 ) ;
#23273 = ORIENTED_EDGE ( 'NONE', *, *, #46352, .F. ) ;
#23274 = FACE_OUTER_BOUND ( 'NONE', #44713, .T. ) ;
#23275 = CARTESIAN_POINT ( 'NONE',  ( 4.268512490100411402E-16, 3.346456692913386100, 1.889763779527550369 ) ) ;
#23276 = VECTOR ( 'NONE', #36034, 39.37007874015748143 ) ;
#23277 = EDGE_CURVE ( 'NONE', #32481, #32615, #12358, .T. ) ;
#23278 = VECTOR ( 'NONE', #18263, 39.37007874015748143 ) ;
#23279 = ORIENTED_EDGE ( 'NONE', *, *, #40295, .T. ) ;
#23280 = VECTOR ( 'NONE', #43724, 39.37007874015748143 ) ;
#23281 = DIRECTION ( 'NONE',  ( -1.000000000000000000, 0.000000000000000000, -0.000000000000000000 ) ) ;
#23282 = LINE ( 'NONE', #50841, #31951 ) ;
#23283 = CARTESIAN_POINT ( 'NONE',  ( 0.7423782071083085965, 0.000000000000000000, -1.141732283464564013 ) ) ;
#23284 = ORIENTED_EDGE ( 'NONE', *, *, #31867, .T. ) ;
#23285 = EDGE_CURVE ( 'NONE', #1516, #38821, #18445, .T. ) ;
#23286 = EDGE_CURVE ( 'NONE', #45509, #11074, #27079, .T. ) ;
#23287 = VERTEX_POINT ( 'NONE', #11841 ) ;
#23288 = DIRECTION ( 'NONE',  ( -3.986037398843765983E-20, -1.000000000000000000, -1.160734090543304660E-16 ) ) ;
#23289 = ORIENTED_EDGE ( 'NONE', *, *, #50334, .F. ) ;
#23290 = DIRECTION ( 'NONE',  ( -0.000000000000000000, 1.000000000000000000, -0.000000000000000000 ) ) ;
#23291 = VERTEX_POINT ( 'NONE', #20357 ) ;
#23292 = LINE ( 'NONE', #42409, #49890 ) ;
#23293 = CARTESIAN_POINT ( 'NONE',  ( 0.6156999374152626325, 1.721443042822825120, -2.415922764597543626 ) ) ;
#23294 = CARTESIAN_POINT ( 'NONE',  ( 0.08139965876239094178, 1.610780518492231694, 0.000000000000000000 ) ) ;
#23295 = ORIENTED_EDGE ( 'NONE', *, *, #28596, .T. ) ;
#23296 = VERTEX_POINT ( 'NONE', #7717 ) ;
#23297 = ORIENTED_EDGE ( 'NONE', *, *, #5261, .T. ) ;
#23298 = DIRECTION ( 'NONE',  ( -0.000000000000000000, 0.000000000000000000, 1.000000000000000000 ) ) ;
#23299 = CARTESIAN_POINT ( 'NONE',  ( 0.07982360342473591996, 1.709180471932028711, 0.000000000000000000 ) ) ;
#23300 = ORIENTED_EDGE ( 'NONE', *, *, #38034, .F. ) ;
#23301 = ORIENTED_EDGE ( 'NONE', *, *, #16257, .T. ) ;
#23302 = DIRECTION ( 'NONE',  ( -1.000000000000000000, 0.000000000000000000, 1.734723475976806848E-16 ) ) ;
#23303 = CARTESIAN_POINT ( 'NONE',  ( -1.091055626815042645, 3.232777166330607521, 2.204724409448808764 ) ) ;
#23304 = LINE ( 'NONE', #35695, #24479 ) ;
#23305 = ORIENTED_EDGE ( 'NONE', *, *, #49650, .T. ) ;
#23306 = ORIENTED_EDGE ( 'NONE', *, *, #41150, .F. ) ;
#23307 = CARTESIAN_POINT ( 'NONE',  ( 0.5455278134075212115, 3.267716535433071279, -6.146657985744592735E-16 ) ) ;
#23308 = DIRECTION ( 'NONE',  ( -0.9195277725514544587, 0.000000000000000000, 0.3930250316539147803 ) ) ;
#23309 = CARTESIAN_POINT ( 'NONE',  ( 2.151809081513405886, 1.574803149606302854, 0.2418202932658659043 ) ) ;
#23310 = ORIENTED_EDGE ( 'NONE', *, *, #14616, .F. ) ;
#23311 = CARTESIAN_POINT ( 'NONE',  ( 1.909347346926324684, 0.000000000000000000, -0.1574803149606304187 ) ) ;
#23312 = CIRCLE ( 'NONE', #6035, 1.850107469027523432 ) ;
#23313 = CARTESIAN_POINT ( 'NONE',  ( -1.091055626815042201, 3.267716535433071279, 1.892679809432643896E-16 ) ) ;
#23314 = EDGE_LOOP ( 'NONE', ( #44399, #41057, #178, #6105 ) ) ;
#23315 = DIRECTION ( 'NONE',  ( -0.01601477604151182663, 0.9998717552508123996, -0.000000000000000000 ) ) ;
#23316 = VERTEX_POINT ( 'NONE', #32245 ) ;
#23317 = ORIENTED_EDGE ( 'NONE', *, *, #45713, .F. ) ;
#23318 = LINE ( 'NONE', #15583, #7290 ) ;
#23319 = LINE ( 'NONE', #19440, #3600 ) ;
#23320 = VECTOR ( 'NONE', #18014, 39.37007874015748143 ) ;
#23321 = VECTOR ( 'NONE', #28863, 39.37007874015748143 ) ;
#23322 = CARTESIAN_POINT ( 'NONE',  ( 0.000000000000000000, 3.346456692913386100, 0.000000000000000000 ) ) ;
#23323 = EDGE_CURVE ( 'NONE', #44282, #50136, #51027, .T. ) ;
#23324 = DIRECTION ( 'NONE',  ( 0.000000000000000000, 0.000000000000000000, -1.000000000000000000 ) ) ;
#23325 = CARTESIAN_POINT ( 'NONE',  ( 0.000000000000000000, 3.267716535433071279, -1.259842519685035800 ) ) ;
#23326 = ORIENTED_EDGE ( 'NONE', *, *, #28160, .F. ) ;
#23328 = ADVANCED_FACE ( 'NONE', ( #12105 ), #35854, .T. ) ;
#23327 = ORIENTED_EDGE ( 'NONE', *, *, #36314, .T. ) ;
#23329 = CIRCLE ( 'NONE', #14268, 2.106299212598425008 ) ;
#23330 = ORIENTED_EDGE ( 'NONE', *, *, #37818, .T. ) ;
#23331 = PLANE ( 'NONE',  #35185 ) ;
#23332 = CARTESIAN_POINT ( 'NONE',  ( 0.000000000000000000, 3.267716535433071279, 0.5905511811023579360 ) ) ;
#23333 = PLANE ( 'NONE',  #19541 ) ;
#23334 = DIRECTION ( 'NONE',  ( -3.469446951953613696E-16, 0.000000000000000000, -1.000000000000000000 ) ) ;
#23335 = ORIENTED_EDGE ( 'NONE', *, *, #4075, .T. ) ;
#23336 = CARTESIAN_POINT ( 'NONE',  ( -0.04921259842519767197, 6.692913385826772199, 2.164795024401847456 ) ) ;
#23337 = EDGE_CURVE ( 'NONE', #30055, #9679, #3852, .T. ) ;
#23338 = PLANE ( 'NONE',  #9209 ) ;
#23339 = ORIENTED_EDGE ( 'NONE', *, *, #9929, .T. ) ;
#23340 = DIRECTION ( 'NONE',  ( 1.000000000000000000, 0.000000000000000000, 0.000000000000000000 ) ) ;
#23341 = EDGE_CURVE ( 'NONE', #17272, #43136, #27841, .T. ) ;
#23342 = LINE ( 'NONE', #39101, #26157 ) ;
#23343 = CARTESIAN_POINT ( 'NONE',  ( 0.000000000000000000, 3.267716535433071279, 0.3149606299212580063 ) ) ;
#23344 = DIRECTION ( 'NONE',  ( 1.734723475976806848E-16, -0.000000000000000000, 1.000000000000000000 ) ) ;
#23345 = CARTESIAN_POINT ( 'NONE',  ( 2.867773316779195447, 1.763947033723992641, -0.7050287376752004675 ) ) ;
#23346 = CARTESIAN_POINT ( 'NONE',  ( -1.439733046521777027, 0.000000000000000000, 1.377952755905504256 ) ) ;
#23347 = AXIS2_PLACEMENT_3D ( 'NONE', #6507, #22499, #50313 ) ;
#23348 = ADVANCED_FACE ( 'NONE', ( #47169 ), #43585, .T. ) ;
#23349 = ORIENTED_EDGE ( 'NONE', *, *, #45912, .F. ) ;
#23350 = VECTOR ( 'NONE', #50915, 39.37007874015748143 ) ;
#23351 = CARTESIAN_POINT ( 'NONE',  ( -1.636583440222563635, 0.000000000000000000, -0.1968503937007879123 ) ) ;
#23352 = ORIENTED_EDGE ( 'NONE', *, *, #38216, .F. ) ;
#23353 = CARTESIAN_POINT ( 'NONE',  ( 1.636583440222563635, 0.000000000000000000, -1.141732283464564013 ) ) ;
#23354 = VECTOR ( 'NONE', #37706, 39.37007874015748143 ) ;
#23355 = VECTOR ( 'NONE', #41635, 39.37007874015748143 ) ;
#23356 = DIRECTION ( 'NONE',  ( -3.469446951953613696E-16, 0.000000000000000000, -1.000000000000000000 ) ) ;
#23357 = DIRECTION ( 'NONE',  ( 1.734723475976806848E-16, 0.000000000000000000, 1.000000000000000000 ) ) ;
#23358 = EDGE_LOOP ( 'NONE', ( #48505, #2096, #5427, #23963 ) ) ;
#23359 = ORIENTED_EDGE ( 'NONE', *, *, #48415, .F. ) ;
#23360 = CARTESIAN_POINT ( 'NONE',  ( -0.8182917201112819283, 0.000000000000000000, -1.929133858267710000 ) ) ;
#23361 = CIRCLE ( 'NONE', #24222, 2.106299212598425008 ) ;
#23362 = CARTESIAN_POINT ( 'NONE',  ( 2.012225602506017452, 1.648623513513363559, -1.855798130189954875 ) ) ;
#23363 = ORIENTED_EDGE ( 'NONE', *, *, #34770, .F. ) ;
#23364 = DIRECTION ( 'NONE',  ( -5.695547044540863592E-17, 1.000000000000000000, 1.156482317317871725E-16 ) ) ;
#23365 = CARTESIAN_POINT ( 'NONE',  ( -0.5455278134075208785, 3.346456692913386100, 1.574803149606291974 ) ) ;
#23366 = DIRECTION ( 'NONE',  ( 1.000000000000000000, 0.000000000000000000, 0.000000000000000000 ) ) ;
#23367 = CARTESIAN_POINT ( 'NONE',  ( -0.3937007874015747699, 0.3937007874015748254, -1.220472440944881942 ) ) ;
#23368 = ORIENTED_EDGE ( 'NONE', *, *, #29099, .F. ) ;
#23369 = CARTESIAN_POINT ( 'NONE',  ( 1.833433833923351353, 3.267716535433071279, 0.7480314960629872445 ) ) ;
#23370 = CARTESIAN_POINT ( 'NONE',  ( 1.953585199828834940, 3.267716535433071279, -0.7874015748031473194 ) ) ;
#23371 = CARTESIAN_POINT ( 'NONE',  ( -1.410501566226149750, -1.929059041884500851E-16, 1.689247093817288992 ) ) ;
#23372 = ORIENTED_EDGE ( 'NONE', *, *, #30289, .F. ) ;
#23373 = LINE ( 'NONE', #23128, #36451 ) ;
#23374 = VERTEX_POINT ( 'NONE', #20087 ) ;
#23375 = ORIENTED_EDGE ( 'NONE', *, *, #16757, .T. ) ;
#23376 = LINE ( 'NONE', #11765, #33329 ) ;
#23377 = ORIENTED_EDGE ( 'NONE', *, *, #50402, .T. ) ;
#23378 = ORIENTED_EDGE ( 'NONE', *, *, #25319, .F. ) ;
#23379 = DIRECTION ( 'NONE',  ( 1.000000000000000000, -0.000000000000000000, 0.000000000000000000 ) ) ;
#23380 = ORIENTED_EDGE ( 'NONE', *, *, #36148, .F. ) ;
#23381 = AXIS2_PLACEMENT_3D ( 'NONE', #43754, #48628, #8410 ) ;
#23382 = EDGE_CURVE ( 'NONE', #25003, #3200, #6729, .T. ) ;
#23383 = EDGE_CURVE ( 'NONE', #49655, #13594, #16233, .T. ) ;
#23384 = AXIS2_PLACEMENT_3D ( 'NONE', #11043, #10539, #33796 ) ;
#23385 = CARTESIAN_POINT ( 'NONE',  ( -0.8329809839909438907, 1.607838722253305486, -2.833254665166566877 ) ) ;
#23386 = FACE_OUTER_BOUND ( 'NONE', #6138, .T. ) ;
#23387 = EDGE_CURVE ( 'NONE', #8195, #7477, #44099, .T. ) ;
#23388 = FACE_OUTER_BOUND ( 'NONE', #20963, .T. ) ;
#23389 = AXIS2_PLACEMENT_3D ( 'NONE', #24904, #48354, #36022 ) ;
#23390 = VECTOR ( 'NONE', #24813, 39.37007874015748143 ) ;
#23391 = ADVANCED_FACE ( 'NONE', ( #32505 ), #16131, .T. ) ;
#23392 = CARTESIAN_POINT ( 'NONE',  ( 0.000000000000000000, 1.574803149606302854, 0.000000000000000000 ) ) ;
#23393 = CARTESIAN_POINT ( 'NONE',  ( -1.909347346926324462, 3.346456692913386100, -0.1574803149606297248 ) ) ;
#23394 = CARTESIAN_POINT ( 'NONE',  ( 0.000000000000000000, 3.267716535433071279, 0.000000000000000000 ) ) ;
#23395 = VECTOR ( 'NONE', #23030, 39.37007874015748143 ) ;
#23396 = ORIENTED_EDGE ( 'NONE', *, *, #20167, .F. ) ;
#23397 = PLANE ( 'NONE',  #38986 ) ;
#23398 = CARTESIAN_POINT ( 'NONE',  ( 1.722315188406978059, 1.746093451223542869, -2.398471789169309254 ) ) ;
#23399 = CARTESIAN_POINT ( 'NONE',  ( 1.887300604142603921, 1.205361022782829114E-17, 0.9597141752041703500 ) ) ;
#23400 = EDGE_LOOP ( 'NONE', ( #26652, #19620, #9258, #45505 ) ) ;
#23401 = PLANE ( 'NONE',  #33118 ) ;
#23402 = EDGE_CURVE ( 'NONE', #9101, #3769, #28350, .T. ) ;
#23403 = DIRECTION ( 'NONE',  ( -0.08963930890344089242, 0.000000000000000000, 0.9959742939952384022 ) ) ;
#23404 = ORIENTED_EDGE ( 'NONE', *, *, #9244, .F. ) ;
#23405 = DIRECTION ( 'NONE',  ( -0.000000000000000000, 1.000000000000000000, -0.000000000000000000 ) ) ;
#23406 = DIRECTION ( 'NONE',  ( -0.8660254037844362651, 0.000000000000000000, 0.5000000000000039968 ) ) ;
#23407 = EDGE_CURVE ( 'NONE', #44687, #39932, #5635, .T. ) ;
#23408 = DIRECTION ( 'NONE',  ( 1.000000000000000000, 0.000000000000000000, 0.000000000000000000 ) ) ;
#23409 = VERTEX_POINT ( 'NONE', #5123 ) ;
#23410 = DIRECTION ( 'NONE',  ( 1.000000000000000000, 0.000000000000000000, 0.000000000000000000 ) ) ;
#23411 = DIRECTION ( 'NONE',  ( 1.734723475976806848E-16, -0.000000000000000000, 1.000000000000000000 ) ) ;
#23412 = FACE_OUTER_BOUND ( 'NONE', #49622, .T. ) ;
#23413 = LINE ( 'NONE', #50478, #30086 ) ;
#23414 = VERTEX_POINT ( 'NONE', #17008 ) ;
#23415 =( GEOMETRIC_REPRESENTATION_CONTEXT ( 3 ) GLOBAL_UNCERTAINTY_ASSIGNED_CONTEXT ( ( #18453 ) ) GLOBAL_UNIT_ASSIGNED_CONTEXT ( ( #2633, #18378, #42122 ) ) REPRESENTATION_CONTEXT ( 'NONE', 'WORKASPACE' ) );
#23416 = ORIENTED_EDGE ( 'NONE', *, *, #18118, .F. ) ;
#23417 = ORIENTED_EDGE ( 'NONE', *, *, #15690, .T. ) ;
#23418 = VECTOR ( 'NONE', #17193, 39.37007874015748143 ) ;
#23419 = CARTESIAN_POINT ( 'NONE',  ( 0.000000000000000000, 3.267716535433071279, 0.3149606299212576177 ) ) ;
#23420 = EDGE_LOOP ( 'NONE', ( #7743, #18343, #20940, #1086 ) ) ;
#23421 = CARTESIAN_POINT ( 'NONE',  ( -0.9052394800409759856, 1.701262340642498039, 2.552059238346994441 ) ) ;
#23422 = FACE_OUTER_BOUND ( 'NONE', #8416, .T. ) ;
#23423 = EDGE_CURVE ( 'NONE', #11433, #34446, #8740, .T. ) ;
#23424 = ORIENTED_EDGE ( 'NONE', *, *, #4177, .T. ) ;
#23425 = AXIS2_PLACEMENT_3D ( 'NONE', #38044, #26159, #6287 ) ;
#23426 = AXIS2_PLACEMENT_3D ( 'NONE', #12883, #8494, #17516 ) ;
#23427 = LINE ( 'NONE', #39180, #37166 ) ;
#23428 = ORIENTED_EDGE ( 'NONE', *, *, #28302, .F. ) ;
#23429 = LINE ( 'NONE', #50489, #50422 ) ;
#23430 = VECTOR ( 'NONE', #23099, 39.37007874015748143 ) ;
#23431 = ORIENTED_EDGE ( 'NONE', *, *, #26096, .F. ) ;
#23432 = ORIENTED_EDGE ( 'NONE', *, *, #50263, .T. ) ;
#23433 = CARTESIAN_POINT ( 'NONE',  ( -2.182111253630085290, 3.267716535433071279, 0.1181102362204704270 ) ) ;
#23434 = VERTEX_POINT ( 'NONE', #13640 ) ;
#23435 = CARTESIAN_POINT ( 'NONE',  ( -0.5455278134075208785, 3.267716535433071279, 1.889763779527550369 ) ) ;
#23436 = ORIENTED_EDGE ( 'NONE', *, *, #10050, .T. ) ;
#23437 = VERTEX_POINT ( 'NONE', #9509 ) ;
#23438 = DIRECTION ( 'NONE',  ( 1.000000000000000000, -0.000000000000000000, 0.000000000000000000 ) ) ;
#23439 = EDGE_CURVE ( 'NONE', #27824, #41536, #17509, .T. ) ;
#23440 = CARTESIAN_POINT ( 'NONE',  ( -1.985260859929297572, 3.346456692913386100, 0.8645800689071783118 ) ) ;
#23441 = VERTEX_POINT ( 'NONE', #5882 ) ;
#23442 = DIRECTION ( 'NONE',  ( -0.01601477604151182663, 0.9998717552508123996, -0.000000000000000000 ) ) ;
#23443 = EDGE_LOOP ( 'NONE', ( #17161, #39511, #10435, #2614 ) ) ;
#23444 = CARTESIAN_POINT ( 'NONE',  ( 2.145564543721536044, 1.465965819140030213, -2.028691429575976812 ) ) ;
#23445 = ADVANCED_FACE ( 'NONE', ( #33019 ), #21635, .F. ) ;
#23446 = DIRECTION ( 'NONE',  ( 0.000000000000000000, 0.000000000000000000, -1.000000000000000000 ) ) ;
#23447 = ADVANCED_FACE ( 'NONE', ( #994 ), #40245, .F. ) ;
#23448 = EDGE_CURVE ( 'NONE', #43946, #34116, #21133, .T. ) ;
#23449 = CARTESIAN_POINT ( 'NONE',  ( -0.3486774197067340486, 3.267716535433071279, -0.1968503937007883287 ) ) ;
#23450 = VERTEX_POINT ( 'NONE', #1506 ) ;
#23451 = VERTEX_POINT ( 'NONE', #21389 ) ;
#23452 = CARTESIAN_POINT ( 'NONE',  ( 0.4696143004045482683, 3.267716535433071279, -1.629301903132388739E-16 ) ) ;
#23453 = CARTESIAN_POINT ( 'NONE',  ( 1.363819533518803695, 0.000000000000000000, 1.535433070866133898 ) ) ;
#23454 = VECTOR ( 'NONE', #1690, 39.37007874015748143 ) ;
#23455 = DIRECTION ( 'NONE',  ( 0.000000000000000000, 0.000000000000000000, -1.000000000000000000 ) ) ;
#23456 = AXIS2_PLACEMENT_3D ( 'NONE', #46728, #27135, #35150 ) ;
#23457 = FACE_OUTER_BOUND ( 'NONE', #42575, .T. ) ;
#23458 = VECTOR ( 'NONE', #8447, 39.37007874015748143 ) ;
#23459 = LINE ( 'NONE', #10838, #5855 ) ;
#23460 = AXIS2_PLACEMENT_3D ( 'NONE', #41517, #30410, #2278 ) ;
#23461 = DIRECTION ( 'NONE',  ( -3.469446951953613696E-16, 0.000000000000000000, -1.000000000000000000 ) ) ;
#23462 = EDGE_CURVE ( 'NONE', #24015, #43876, #18888, .T. ) ;
#23463 = ORIENTED_EDGE ( 'NONE', *, *, #28004, .T. ) ;
#23464 = LINE ( 'NONE', #15478, #7767 ) ;
#23465 = VECTOR ( 'NONE', #4835, 39.37007874015748143 ) ;
#23466 = VERTEX_POINT ( 'NONE', #20870 ) ;
#23467 = DIRECTION ( 'NONE',  ( 0.000000000000000000, 1.000000000000000000, -0.000000000000000000 ) ) ;
#23468 = ADVANCED_FACE ( 'NONE', ( #37140 ), #28609, .F. ) ;
#23469 = ORIENTED_EDGE ( 'NONE', *, *, #48322, .F. ) ;
#23470 = ORIENTED_EDGE ( 'NONE', *, *, #36603, .F. ) ;
#23471 = CARTESIAN_POINT ( 'NONE',  ( -1.166969139818015977, 0.000000000000000000, 1.732283464566920950 ) ) ;
#23472 = CARTESIAN_POINT ( 'NONE',  ( -2.100190309385016274, 5.905511811023623991, 0.5298329251847222476 ) ) ;
#23473 = EDGE_LOOP ( 'NONE', ( #47981, #32314, #33159, #4936 ) ) ;
#23474 = EDGE_CURVE ( 'NONE', #19508, #37443, #33269, .T. ) ;
#23475 = B_SPLINE_CURVE_WITH_KNOTS ( 'NONE', 3,
 ( #12059, #27283, #3291, #31947 ),
 .UNSPECIFIED., .F., .F.,
 ( 4, 4 ),
 ( 0.001544765274254495443, 0.004044898643818962448 ),
 .UNSPECIFIED. ) ;
#23476 = PLANE ( 'NONE',  #50139 ) ;
#23477 = ORIENTED_EDGE ( 'NONE', *, *, #16125, .T. ) ;
#23478 = CARTESIAN_POINT ( 'NONE',  ( 0.000000000000000000, 1.574803149606302854, 0.000000000000000000 ) ) ;
#23479 = EDGE_CURVE ( 'NONE', #18853, #25196, #2013, .T. ) ;
#23480 = ORIENTED_EDGE ( 'NONE', *, *, #26777, .T. ) ;
#23481 = DIRECTION ( 'NONE',  ( -0.000000000000000000, 0.000000000000000000, 1.000000000000000000 ) ) ;
#23482 = LINE ( 'NONE', #3875, #10761 ) ;
#23483 = EDGE_LOOP ( 'NONE', ( #10863, #2757, #33310, #42841 ) ) ;
#23484 = LINE ( 'NONE', #15740, #44491 ) ;
#23485 = AXIS2_PLACEMENT_3D ( 'NONE', #25, #8543, #47488 ) ;
#23486 = VERTEX_POINT ( 'NONE', #9001 ) ;
#23487 = ORIENTED_EDGE ( 'NONE', *, *, #35226, .F. ) ;
#23488 = AXIS2_PLACEMENT_3D ( 'NONE', #12825, #39419, #20303 ) ;
#23489 = ADVANCED_FACE ( 'NONE', ( #40496 ), #1250, .F. ) ;
#23490 = CONICAL_SURFACE ( 'NONE', #1249, 1.850107469027523210, 0.6386652850508578450 ) ;
#23491 = FACE_OUTER_BOUND ( 'NONE', #6423, .T. ) ;
#23492 = DIRECTION ( 'NONE',  ( -3.986037398843765983E-20, -1.000000000000000000, -1.160734090543304660E-16 ) ) ;
#23493 = DIRECTION ( 'NONE',  ( 1.000000000000000000, 0.000000000000000000, 0.000000000000000000 ) ) ;
#23494 = AXIS2_PLACEMENT_3D ( 'NONE', #16387, #4764, #36267 ) ;
#23495 = EDGE_CURVE ( 'NONE', #26927, #35609, #38157, .T. ) ;
#23496 = ORIENTED_EDGE ( 'NONE', *, *, #19686, .T. ) ;
#23497 = CARTESIAN_POINT ( 'NONE',  ( 1.363819533518803029, 3.267716535433071279, -2.365849761790804994E-16 ) ) ;
#23498 = DIRECTION ( 'NONE',  ( 0.000000000000000000, -0.000000000000000000, 1.000000000000000000 ) ) ;
#23499 = ORIENTED_EDGE ( 'NONE', *, *, #42591, .T. ) ;
#23500 = CARTESIAN_POINT ( 'NONE',  ( 0.1067246931122726866, 0.02962905676920215767, 0.000000000000000000 ) ) ;
#23501 = VECTOR ( 'NONE', #5846, 39.37007874015748854 ) ;
#23502 = ORIENTED_EDGE ( 'NONE', *, *, #29010, .T. ) ;
#23503 = ORIENTED_EDGE ( 'NONE', *, *, #23439, .F. ) ;
#23504 = VERTEX_POINT ( 'NONE', #7163 ) ;
#23505 = LINE ( 'NONE', #39257, #12763 ) ;
#23506 = EDGE_CURVE ( 'NONE', #26706, #49094, #18265, .T. ) ;
#23507 = DIRECTION ( 'NONE',  ( 1.000000000000000000, 0.000000000000000000, -3.469446951953613696E-16 ) ) ;
#23508 = CARTESIAN_POINT ( 'NONE',  ( -0.8182917201112817063, 3.267716535433071279, 1.419509857074483046E-16 ) ) ;
#23509 = EDGE_CURVE ( 'NONE', #9566, #34698, #46578, .T. ) ;
#23510 = LINE ( 'NONE', #15017, #43643 ) ;
#23511 = ORIENTED_EDGE ( 'NONE', *, *, #37444, .F. ) ;
#23512 = ORIENTED_EDGE ( 'NONE', *, *, #14354, .F. ) ;
#23513 = CARTESIAN_POINT ( 'NONE',  ( -2.122091976112999490, 5.905511811023623991, 0.4338754535132827161 ) ) ;
#23514 = CARTESIAN_POINT ( 'NONE',  ( -2.689601439366095192, 1.673243075243657563, -0.07152793773621130002 ) ) ;
#23515 = ORIENTED_EDGE ( 'NONE', *, *, #2845, .T. ) ;
#23516 = PLANE ( 'NONE',  #10138 ) ;
#23517 = CARTESIAN_POINT ( 'NONE',  ( 0.000000000000000000, 3.267716535433071279, 0.000000000000000000 ) ) ;
#23518 = CARTESIAN_POINT ( 'NONE',  ( 0.08139965876239094178, 1.610780518492231694, 0.000000000000000000 ) ) ;
#23519 = DIRECTION ( 'NONE',  ( 0.000000000000000000, 1.000000000000000000, 0.000000000000000000 ) ) ;
#23520 = DIRECTION ( 'NONE',  ( 0.000000000000000000, 0.000000000000000000, 1.000000000000000000 ) ) ;
#23521 = CARTESIAN_POINT ( 'NONE',  ( -1.909347346926325129, 3.267716535433071279, 3.312189666507129161E-16 ) ) ;
#23522 = ORIENTED_EDGE ( 'NONE', *, *, #3518, .F. ) ;
#23523 = CARTESIAN_POINT ( 'NONE',  ( -1.091055626815042645, 3.346456692913386100, -0.9448818897637760728 ) ) ;
#23524 = CARTESIAN_POINT ( 'NONE',  ( -0.9836083787002329881, 5.905511811023623991, -1.929060376159713375 ) ) ;
#23525 = VECTOR ( 'NONE', #46071, 39.37007874015748143 ) ;
#23526 = ORIENTED_EDGE ( 'NONE', *, *, #22716, .T. ) ;
#23527 = AXIS2_PLACEMENT_3D ( 'NONE', #16058, #8310, #28432 ) ;
#23528 = ORIENTED_EDGE ( 'NONE', *, *, #2616, .T. ) ;
#23529 = CARTESIAN_POINT ( 'NONE',  ( 0.8182917201112817063, 0.000000000000000000, -1.929133858267711110 ) ) ;
#23530 = LINE ( 'NONE', #27914, #25339 ) ;
#23531 = CARTESIAN_POINT ( 'NONE',  ( 0.5114069481605333367, 0.000000000000000000, -1.915028406767218749 ) ) ;
#23532 = VECTOR ( 'NONE', #46458, 39.37007874015748143 ) ;
#23533 = ORIENTED_EDGE ( 'NONE', *, *, #40207, .T. ) ;
#23534 = ADVANCED_FACE ( 'NONE', ( #18528 ), #26015, .F. ) ;
#23535 = VECTOR ( 'NONE', #19411, 39.37007874015748143 ) ;
#23536 = ORIENTED_EDGE ( 'NONE', *, *, #44543, .T. ) ;
#23537 = DIRECTION ( 'NONE',  ( -3.986037398843765983E-20, -1.000000000000000000, -1.160734090543304660E-16 ) ) ;
#23538 = ORIENTED_EDGE ( 'NONE', *, *, #4846, .T. ) ;
#23539 = CARTESIAN_POINT ( 'NONE',  ( 0.5455278134075212115, 3.267716535433071279, 0.9448818897637746295 ) ) ;
#23540 = ADVANCED_FACE ( 'NONE', ( #21892 ), #22900, .F. ) ;
#23541 = VERTEX_POINT ( 'NONE', #3279 ) ;
#23542 = DIRECTION ( 'NONE',  ( -3.986037398843765983E-20, -1.000000000000000000, -1.160734090543304660E-16 ) ) ;
#23543 = CARTESIAN_POINT ( 'NONE',  ( -1.662320194739477452, 1.205361022782829114E-17, -1.388601395075575784 ) ) ;
#23544 = CARTESIAN_POINT ( 'NONE',  ( 1.598711713508005117, 1.574803149606302854, -1.460438370699377986 ) ) ;
#23545 = EDGE_CURVE ( 'NONE', #31120, #30710, #11025, .T. ) ;
#23546 = EDGE_CURVE ( 'NONE', #49534, #8198, #49715, .T. ) ;
#23547 = EDGE_LOOP ( 'NONE', ( #49939, #50531, #1944, #46407 ) ) ;
#23548 = ORIENTED_EDGE ( 'NONE', *, *, #5615, .F. ) ;
#23549 = ORIENTED_EDGE ( 'NONE', *, *, #3298, .T. ) ;
#23550 = DIRECTION ( 'NONE',  ( 0.000000000000000000, 1.000000000000000000, 0.000000000000000000 ) ) ;
#23551 = CARTESIAN_POINT ( 'NONE',  ( 0.2727639067037604947, 3.267716535433071279, -1.417322834645664331 ) ) ;
#23552 = ORIENTED_EDGE ( 'NONE', *, *, #9955, .T. ) ;
#23553 = VERTEX_POINT ( 'NONE', #14651 ) ;
#23554 = FACE_OUTER_BOUND ( 'NONE', #1485, .T. ) ;
#23555 = LINE ( 'NONE', #39310, #21973 ) ;
#23556 = CARTESIAN_POINT ( 'NONE',  ( -1.486187880958815377, 3.267716535433071279, -1.574803149606293307 ) ) ;
#23557 = VERTEX_POINT ( 'NONE', #42516 ) ;
#23558 = ORIENTED_EDGE ( 'NONE', *, *, #20400, .T. ) ;
#23559 = CARTESIAN_POINT ( 'NONE',  ( -2.491402175429631605, 1.567214198537667302, -1.585592796919542025 ) ) ;
#23560 = CARTESIAN_POINT ( 'NONE',  ( -1.636583440222564301, 0.000000000000000000, -0.6299212598425177889 ) ) ;
#23561 = DIRECTION ( 'NONE',  ( -0.000000000000000000, -1.000000000000000000, -0.000000000000000000 ) ) ;
#23562 = ORIENTED_EDGE ( 'NONE', *, *, #11258, .T. ) ;
#23563 =( CONVERSION_BASED_UNIT ( 'INCH', #5802 ) LENGTH_UNIT ( ) NAMED_UNIT ( #32082 ) );
#23564 = DIRECTION ( 'NONE',  ( 1.734723475976806848E-16, 0.000000000000000000, 1.000000000000000000 ) ) ;
#23565 = VECTOR ( 'NONE', #43904, 39.37007874015748143 ) ;
#23566 = EDGE_LOOP ( 'NONE', ( #36756, #44990, #37506, #23229 ) ) ;
#23567 = VECTOR ( 'NONE', #31719, 39.37007874015748143 ) ;
#23568 = CARTESIAN_POINT ( 'NONE',  ( -0.6214413264104939882, 3.346456692913386100, 0.9055118110236167750 ) ) ;
#23569 = VERTEX_POINT ( 'NONE', #6653 ) ;
#23570 = ORIENTED_EDGE ( 'NONE', *, *, #47454, .T. ) ;
#23571 = CARTESIAN_POINT ( 'NONE',  ( -1.971247363764855098, 6.692913385826772199, -0.8960709840011926719 ) ) ;
#23572 = CARTESIAN_POINT ( 'NONE',  ( 0.2727639067037602172, 0.000000000000000000, -1.929133858267710000 ) ) ;
#23573 = AXIS2_PLACEMENT_3D ( 'NONE', #40152, #32153, #12515 ) ;
#23574 = EDGE_CURVE ( 'NONE', #35899, #34255, #33781, .T. ) ;
#23575 = CARTESIAN_POINT ( 'NONE',  ( -0.5324620714980967673, 1.707112762236906667, 2.658494868336626737 ) ) ;
#23576 = CONICAL_SURFACE ( 'NONE', #8732, 2.246510896728926010, 0.01601546068027819014 ) ;
#23577 = FACE_OUTER_BOUND ( 'NONE', #32467, .T. ) ;
#23578 = EDGE_CURVE ( 'NONE', #23486, #27371, #17794, .T. ) ;
#23579 = DIRECTION ( 'NONE',  ( -3.469446951953613696E-16, 0.000000000000000000, -1.000000000000000000 ) ) ;
#23580 = EDGE_LOOP ( 'NONE', ( #38000, #310, #44586, #47962 ) ) ;
#23581 = B_SPLINE_CURVE_WITH_KNOTS ( 'NONE', 3,
 ( #36000, #39864, #1388, #4756 ),
 .UNSPECIFIED., .F., .F.,
 ( 4, 4 ),
 ( 2.559257443457554172E-07, 0.002500529213542272873 ),
 .UNSPECIFIED. ) ;
#23582 = VERTEX_POINT ( 'NONE', #34530 ) ;
#23583 = VECTOR ( 'NONE', #15872, 39.37007874015748143 ) ;
#23584 = EDGE_CURVE ( 'NONE', #18622, #31182, #10522, .T. ) ;
#23585 = PRODUCT_DEFINITION_SHAPE ( 'NONE', 'NONE',  #51055 ) ;
#23586 = EDGE_LOOP ( 'NONE', ( #49211, #46782, #5548, #38521 ) ) ;
#23587 = CARTESIAN_POINT ( 'NONE',  ( 2.951990591674675368, 1.765258879000601855, -0.08331184815398361143 ) ) ;
#23588 = DIRECTION ( 'NONE',  ( 0.000000000000000000, 1.000000000000000000, 0.000000000000000000 ) ) ;
#23589 = ADVANCED_FACE ( 'NONE', ( #46117 ), #8690, .T. ) ;
#23590 = LINE ( 'NONE', #24620, #32700 ) ;
#23591 = CARTESIAN_POINT ( 'NONE',  ( -2.121469926805683137, 1.574803149606302854, -0.4337334748181708721 ) ) ;
#23592 = VERTEX_POINT ( 'NONE', #25759 ) ;
#23593 = FACE_OUTER_BOUND ( 'NONE', #50007, .T. ) ;
#23594 = CARTESIAN_POINT ( 'NONE',  ( -1.486187880958816931, 3.267716535433071279, 1.574803149606291530 ) ) ;
#23595 = ORIENTED_EDGE ( 'NONE', *, *, #38774, .F. ) ;
#23596 = DIRECTION ( 'NONE',  ( 1.734723475976806848E-16, -0.000000000000000000, 1.000000000000000000 ) ) ;
#23597 = DIRECTION ( 'NONE',  ( 1.000000000000000000, 0.000000000000000000, 0.000000000000000000 ) ) ;
#23598 = LINE ( 'NONE', #50912, #33750 ) ;
#23599 = EDGE_LOOP ( 'NONE', ( #33492, #30201, #47372, #48623 ) ) ;
#23600 = PLANE ( 'NONE',  #24293 ) ;
#23601 = CARTESIAN_POINT ( 'NONE',  ( 0.5455278134075212115, 3.346456692913386100, -1.259842519685035134 ) ) ;
#23602 = DIRECTION ( 'NONE',  ( -0.000000000000000000, -1.000000000000000000, -0.000000000000000000 ) ) ;
#23603 = VECTOR ( 'NONE', #42589, 39.37007874015748143 ) ;
#23604 = VECTOR ( 'NONE', #1180, 39.37007874015748143 ) ;
#23605 = VERTEX_POINT ( 'NONE', #37651 ) ;
#23606 = DIRECTION ( 'NONE',  ( -1.000000000000000000, -0.000000000000000000, -0.000000000000000000 ) ) ;
#23607 = ORIENTED_EDGE ( 'NONE', *, *, #5836, .T. ) ;
#23608 = CARTESIAN_POINT ( 'NONE',  ( 1.560669927219590747, 3.267716535433071279, -5.414661521997677271E-16 ) ) ;
#23609 = VECTOR ( 'NONE', #2935, 39.37007874015748143 ) ;
#23610 = DIRECTION ( 'NONE',  ( 0.000000000000000000, 0.000000000000000000, 1.000000000000000000 ) ) ;
#23611 = CARTESIAN_POINT ( 'NONE',  ( 0.000000000000000000, 0.000000000000000000, -0.3937007874015748254 ) ) ;
#23612 = EDGE_CURVE ( 'NONE', #4851, #28481, #29641, .T. ) ;
#23613 = VECTOR ( 'NONE', #27766, 39.37007874015748143 ) ;
#23614 = B_SPLINE_CURVE_WITH_KNOTS ( 'NONE', 3,
 ( #44802, #9455, #25197, #38103 ),
 .UNSPECIFIED., .F., .F.,
 ( 4, 4 ),
 ( 0.01452380394872818808, 0.03074912581988934607 ),
 .UNSPECIFIED. ) ;
#23615 = EDGE_CURVE ( 'NONE', #18225, #17559, #29892, .T. ) ;
#23616 = EDGE_CURVE ( 'NONE', #29102, #5349, #42258, .T. ) ;
#23617 = CONICAL_SURFACE ( 'NONE', #7959, 3.033577403570480779, 1.554780866114618743 ) ;
#23618 = ORIENTED_EDGE ( 'NONE', *, *, #40647, .T. ) ;
#23619 = ORIENTED_EDGE ( 'NONE', *, *, #4328, .F. ) ;
#23620 = DIRECTION ( 'NONE',  ( -4.561975526775602830E-17, -1.000000000000000000, -1.067327232801823148E-16 ) ) ;
#23621 = CARTESIAN_POINT ( 'NONE',  ( -1.091055626815042201, 3.346456692913386100, 1.574803149606291974 ) ) ;
#23622 = VERTEX_POINT ( 'NONE', #46365 ) ;
#23623 = FACE_OUTER_BOUND ( 'NONE', #27722, .T. ) ;
#23624 = CARTESIAN_POINT ( 'NONE',  ( 1.772877181557974025, 1.670681026536232405, 1.476767650018351752 ) ) ;
#23625 = CARTESIAN_POINT ( 'NONE',  ( -1.405664884363581502, 1.586962458333645021, 1.683711065981816857 ) ) ;
#23626 = EDGE_CURVE ( 'NONE', #19859, #16076, #19598, .T. ) ;
#23627 = FACE_OUTER_BOUND ( 'NONE', #1404, .T. ) ;
#23628 = VERTEX_POINT ( 'NONE', #10017 ) ;
#23629 = EDGE_LOOP ( 'NONE', ( #28055, #40552, #33973, #981 ) ) ;
#23630 = DIRECTION ( 'NONE',  ( -3.469446951953613696E-16, 0.000000000000000000, -1.000000000000000000 ) ) ;
#23631 = CARTESIAN_POINT ( 'NONE',  ( -1.775400203342670347, 1.691590761327236958, -2.359903268218729089 ) ) ;
#23632 = ORIENTED_EDGE ( 'NONE', *, *, #14138, .F. ) ;
#23633 = CARTESIAN_POINT ( 'NONE',  ( -1.901641471869979894, -1.240704811463216626E-16, 1.079202499698820095 ) ) ;
#23634 = VERTEX_POINT ( 'NONE', #22150 ) ;
#23635 = ORIENTED_EDGE ( 'NONE', *, *, #47192, .F. ) ;
#23636 = EDGE_CURVE ( 'NONE', #35692, #18948, #23658, .T. ) ;
#23637 = CARTESIAN_POINT ( 'NONE',  ( 0.000000000000000000, 6.692913385826772199, -2.165354330708661568 ) ) ;
#23638 = EDGE_CURVE ( 'NONE', #25781, #43935, #6090, .T. ) ;
#23639 = AXIS2_PLACEMENT_3D ( 'NONE', #15418, #23403, #19781 ) ;
#23640 = ORIENTED_EDGE ( 'NONE', *, *, #50678, .T. ) ;
#23641 = EDGE_LOOP ( 'NONE', ( #20505, #28146, #18623, #15136 ) ) ;
#23642 = CARTESIAN_POINT ( 'NONE',  ( -1.591447364397243103, 0.002429723416550041374, -0.7337366736851151927 ) ) ;
#23643 = EDGE_CURVE ( 'NONE', #48864, #17840, #43263, .T. ) ;
#23644 = ORIENTED_EDGE ( 'NONE', *, *, #3076, .T. ) ;
#23645 = CIRCLE ( 'NONE', #7148, 2.106299212598425008 ) ;
#23646 = ADVANCED_FACE ( 'NONE', ( #12302 ), #3534, .F. ) ;
#23647 = CARTESIAN_POINT ( 'NONE',  ( -1.439733046521776583, 0.000000000000000000, -0.6299212598425177889 ) ) ;
#23648 = EDGE_CURVE ( 'NONE', #23094, #20677, #19271, .T. ) ;
#23649 = CARTESIAN_POINT ( 'NONE',  ( 1.091055626815042645, 0.000000000000000000, 1.259842519685033357 ) ) ;
#23650 = LINE ( 'NONE', #3782, #20096 ) ;
#23651 = AXIS2_PLACEMENT_3D ( 'NONE', #20724, #32882, #9877 ) ;
#23652 = DIRECTION ( 'NONE',  ( 1.734723475976806848E-16, 0.000000000000000000, 1.000000000000000000 ) ) ;
#23653 = AXIS2_PLACEMENT_3D ( 'NONE', #22998, #3372, #15746 ) ;
#23654 = CARTESIAN_POINT ( 'NONE',  ( 3.054013992583308121E-16, 3.346456692913386100, 2.493791675044291445 ) ) ;
#23655 = CARTESIAN_POINT ( 'NONE',  ( 1.956192433058983493, 0.05925166736471587647, -0.03859050128386512513 ) ) ;
#23656 = VERTEX_POINT ( 'NONE', #50709 ) ;
#23657 = LINE ( 'NONE', #15659, #32421 ) ;
#23658 = LINE ( 'NONE', #419, #36744 ) ;
#23659 = LINE ( 'NONE', #12044, #24869 ) ;
#23660 = VERTEX_POINT ( 'NONE', #15414 ) ;
#23661 = CARTESIAN_POINT ( 'NONE',  ( -1.439733046521776583, 3.267716535433071279, 4.995077429881868843E-16 ) ) ;
#23662 = CARTESIAN_POINT ( 'NONE',  ( 0.5455278134075212115, 0.000000000000000000, -0.6299212598425181220 ) ) ;
#23663 = ORIENTED_EDGE ( 'NONE', *, *, #30595, .F. ) ;
#23664 = PLANE ( 'NONE',  #13905 ) ;
#23665 = CARTESIAN_POINT ( 'NONE',  ( -0.6214413264104945434, 0.000000000000000000, -2.047244094488181343 ) ) ;
#23666 = DIRECTION ( 'NONE',  ( 1.734723475976806848E-16, -0.000000000000000000, 1.000000000000000000 ) ) ;
#23667 = PLANE ( 'NONE',  #24101 ) ;
#23668 = ORIENTED_EDGE ( 'NONE', *, *, #46384, .T. ) ;
#23669 = CARTESIAN_POINT ( 'NONE',  ( -0.07591351300297333182, 3.267716535433071279, -0.7874015748031470974 ) ) ;
#23670 = LINE ( 'NONE', #7674, #17696 ) ;
#23671 = B_SPLINE_CURVE_WITH_KNOTS ( 'NONE', 3,
 ( #37896, #10258, #11274, #7401 ),
 .UNSPECIFIED., .F., .F.,
 ( 4, 4 ),
 ( 0.1211873102087489551, 0.1625992483279400380 ),
 .UNSPECIFIED. ) ;
#23672 = DIRECTION ( 'NONE',  ( 0.2225209339563184452, 0.000000000000000000, -0.9749279121818227312 ) ) ;
#23673 = CARTESIAN_POINT ( 'NONE',  ( 0.2430652128771964016, 5.905511811023623991, -2.151668812760858085 ) ) ;
#23674 = VERTEX_POINT ( 'NONE', #31157 ) ;
#23675 = VECTOR ( 'NONE', #1860, 39.37007874015748143 ) ;
#23676 = AXIS2_PLACEMENT_3D ( 'NONE', #39859, #28487, #16376 ) ;
#23677 = EDGE_CURVE ( 'NONE', #18617, #14797, #50461, .T. ) ;
#23678 = AXIS2_PLACEMENT_3D ( 'NONE', #15150, #43259, #46608 ) ;
#23679 = ORIENTED_EDGE ( 'NONE', *, *, #11485, .T. ) ;
#23680 = ORIENTED_EDGE ( 'NONE', *, *, #47881, .T. ) ;
#23681 = EDGE_CURVE ( 'NONE', #27359, #50172, #43523, .T. ) ;
#23682 = CARTESIAN_POINT ( 'NONE',  ( 0.000000000000000000, 3.267716535433071279, -0.1574803149606301411 ) ) ;
#23683 = ORIENTED_EDGE ( 'NONE', *, *, #47192, .T. ) ;
#23684 = CARTESIAN_POINT ( 'NONE',  ( -0.7053729475263631477, 3.346456692913386100, 2.047244094488179567 ) ) ;
#23685 = LINE ( 'NONE', #35061, #16187 ) ;
#23686 = ORIENTED_EDGE ( 'NONE', *, *, #43956, .F. ) ;
#23687 = EDGE_CURVE ( 'NONE', #2040, #35748, #22731, .T. ) ;
#23688 = CARTESIAN_POINT ( 'NONE',  ( 1.905671854841463952, 1.472358791367697650, 2.256015092822682089 ) ) ;
#23689 = VERTEX_POINT ( 'NONE', #24177 ) ;
#23690 = CARTESIAN_POINT ( 'NONE',  ( 0.8329809839909855240, 5.905511811023623991, -2.833254665166554442 ) ) ;
#23691 = DIRECTION ( 'NONE',  ( -0.000000000000000000, 1.000000000000000000, -0.000000000000000000 ) ) ;
#23692 = EDGE_LOOP ( 'NONE', ( #7332, #158, #30740, #1983, #29389 ) ) ;
#23693 = VERTEX_POINT ( 'NONE', #15156 ) ;
#23694 = LINE ( 'NONE', #35578, #38913 ) ;
#23695 = ORIENTED_EDGE ( 'NONE', *, *, #35654, .T. ) ;
#23696 = VECTOR ( 'NONE', #26263, 39.37007874015748143 ) ;
#23697 = CARTESIAN_POINT ( 'NONE',  ( -0.07591351300297284610, 3.346456692913386100, 1.535433070866133898 ) ) ;
#23698 = EDGE_CURVE ( 'NONE', #11755, #33217, #39922, .T. ) ;
#23699 = ORIENTED_EDGE ( 'NONE', *, *, #22437, .T. ) ;
#23700 = EDGE_LOOP ( 'NONE', ( #14730, #37982, #13601, #16599 ) ) ;
#23701 = CARTESIAN_POINT ( 'NONE',  ( -1.909347346926324462, 3.346456692913386100, -0.03937007874015881204 ) ) ;
#23702 = EDGE_CURVE ( 'NONE', #17198, #18215, #32623, .T. ) ;
#23703 = DIRECTION ( 'NONE',  ( -0.000000000000000000, 1.000000000000000000, -0.000000000000000000 ) ) ;
#23704 = EDGE_CURVE ( 'NONE', #19800, #4856, #46615, .T. ) ;
#23705 = EDGE_LOOP ( 'NONE', ( #15935, #32533 ) ) ;
#23706 = DIRECTION ( 'NONE',  ( 0.000000000000000000, 0.000000000000000000, -1.000000000000000000 ) ) ;
#23707 = ORIENTED_EDGE ( 'NONE', *, *, #24265, .T. ) ;
#23708 = CARTESIAN_POINT ( 'NONE',  ( 1.287906020515829919, 3.267716535433071279, -4.468321617281354090E-16 ) ) ;
#23709 = DIRECTION ( 'NONE',  ( -1.000000000000000000, 0.000000000000000000, 1.734723475976806848E-16 ) ) ;
#23710 = VECTOR ( 'NONE', #24058, 39.37007874015748143 ) ;
#23711 = CIRCLE ( 'NONE', #1462, 2.106299212598425008 ) ;
#23712 = CARTESIAN_POINT ( 'NONE',  ( -2.464291103507775915, 0.000000000000000000, -1.626664315311338260 ) ) ;
#23713 = ORIENTED_EDGE ( 'NONE', *, *, #27487, .F. ) ;
#23714 = ORIENTED_EDGE ( 'NONE', *, *, #42644, .T. ) ;
#23715 = PLANE ( 'NONE',  #24469 ) ;
#23716 = DIRECTION ( 'NONE',  ( 1.000000000000000000, 0.000000000000000000, 0.000000000000000000 ) ) ;
#23717 = DIRECTION ( 'NONE',  ( -3.469446951953613696E-16, 0.000000000000000000, -1.000000000000000000 ) ) ;
#23718 = VECTOR ( 'NONE', #23244, 39.37007874015748143 ) ;
#23719 = CARTESIAN_POINT ( 'NONE',  ( 2.165460538733997353, 0.000000000000000000, 0.04798874274655835076 ) ) ;
#23720 = CARTESIAN_POINT ( 'NONE',  ( 1.091055626815042867, 3.267716535433071279, -1.892679809432645129E-16 ) ) ;
#23721 = CARTESIAN_POINT ( 'NONE',  ( 0.000000000000000000, 3.267716535433071279, -0.03937007874015868020 ) ) ;
#23722 = VERTEX_POINT ( 'NONE', #31409 ) ;
#23723 = DIRECTION ( 'NONE',  ( 0.7227948638273880011, 0.000000000000000000, 0.6910626489868685329 ) ) ;
#23724 = VECTOR ( 'NONE', #13313, 39.37007874015748143 ) ;
#23725 = ORIENTED_EDGE ( 'NONE', *, *, #45996, .F. ) ;
#23726 = CARTESIAN_POINT ( 'NONE',  ( 1.661821349926414726, 1.574803149606302854, 1.388203579611976268 ) ) ;
#23727 = VECTOR ( 'NONE', #8869, 39.37007874015748143 ) ;
#23728 = VERTEX_POINT ( 'NONE', #42765 ) ;
#23729 = DIRECTION ( 'NONE',  ( 0.2225209339563041788, 0.000000000000000000, 0.9749279121818259508 ) ) ;
#23730 = DIRECTION ( 'NONE',  ( -0.000000000000000000, 1.000000000000000000, -0.000000000000000000 ) ) ;
#23731 = ORIENTED_EDGE ( 'NONE', *, *, #49935, .F. ) ;
#23732 = EDGE_CURVE ( 'NONE', #40030, #32732, #47364, .T. ) ;
#23733 = DIRECTION ( 'NONE',  ( 1.734723475976806848E-16, 0.000000000000000000, 1.000000000000000000 ) ) ;
#23734 = ADVANCED_FACE ( 'NONE', ( #27522 ), #20024, .F. ) ;
#23735 = VERTEX_POINT ( 'NONE', #11780 ) ;
#23736 = LINE ( 'NONE', #15235, #49338 ) ;
#23737 = ORIENTED_EDGE ( 'NONE', *, *, #263, .T. ) ;
#23738 = EDGE_CURVE ( 'NONE', #13805, #41605, #27269, .T. ) ;
#23739 = PRODUCT_DEFINITION ( 'UNKNOWN', '', #35814, #24727 ) ;
#23740 = DIRECTION ( 'NONE',  ( -0.000000000000000000, 0.000000000000000000, 1.000000000000000000 ) ) ;
#23741 = CARTESIAN_POINT ( 'NONE',  ( 0.002207914879453961535, -5.712274067634378313E-18, 0.04916304461325374242 ) ) ;
#23742 = EDGE_CURVE ( 'NONE', #32550, #13413, #50967, .T. ) ;
#23743 = AXIS2_PLACEMENT_3D ( 'NONE', #11673, #23290, #31817 ) ;
#23744 = VECTOR ( 'NONE', #15168, 39.37007874015748143 ) ;
#23745 = EDGE_CURVE ( 'NONE', #3425, #36591, #8172, .T. ) ;
#23746 = EDGE_LOOP ( 'NONE', ( #14376, #28440, #17600, #34933 ) ) ;
#23747 = CARTESIAN_POINT ( 'NONE',  ( -0.8069532150559458605, 0.000000000000000000, -2.010061882867143268 ) ) ;
#23748 = ORIENTED_EDGE ( 'NONE', *, *, #49872, .T. ) ;
#23749 = ORIENTED_EDGE ( 'NONE', *, *, #42491, .T. ) ;
#23750 = CARTESIAN_POINT ( 'NONE',  ( 1.979793062125284830, 1.470624965921384364, 2.191257344206569257 ) ) ;
#23751 = CARTESIAN_POINT ( 'NONE',  ( -1.363819533518803473, 0.000000000000000000, -0.7874015748031470974 ) ) ;
#23752 = DIRECTION ( 'NONE',  ( 0.000000000000000000, -1.000000000000000000, 0.000000000000000000 ) ) ;
#23753 = VECTOR ( 'NONE', #5229, 39.37007874015748143 ) ;
#23754 = ORIENTED_EDGE ( 'NONE', *, *, #21265, .T. ) ;
#23755 = VECTOR ( 'NONE', #48529, 39.37007874015748143 ) ;
#23756 = DIRECTION ( 'NONE',  ( 0.000000000000000000, 0.000000000000000000, -1.000000000000000000 ) ) ;
#23757 = ADVANCED_FACE ( 'NONE', ( #35795 ), #16435, .F. ) ;
#23758 = CARTESIAN_POINT ( 'NONE',  ( -0.07591351300297316529, 3.267716535433071279, 2.633779063002562669E-17 ) ) ;
#23759 = ORIENTED_EDGE ( 'NONE', *, *, #33146, .F. ) ;
#23760 = AXIS2_PLACEMENT_3D ( 'NONE', #3268, #46104, #19257 ) ;
#23761 = CARTESIAN_POINT ( 'NONE',  ( 2.378961647330872786, 3.267716535433071279, -0.3149606299212596716 ) ) ;
#23762 = EDGE_CURVE ( 'NONE', #45153, #46201, #6015, .T. ) ;
#23763 = VERTEX_POINT ( 'NONE', #24435 ) ;
#23764 = EDGE_LOOP ( 'NONE', ( #46898, #27931, #2052, #8926 ) ) ;
#23765 = ITEM_DEFINED_TRANSFORMATION ( 'NONE', 'NONE', #32511,  #26741 ) ;
#23766 = VECTOR ( 'NONE', #28988, 39.37007874015748143 ) ;
#23767 = ORIENTED_EDGE ( 'NONE', *, *, #50916, .T. ) ;
#23768 = DIRECTION ( 'NONE',  ( -0.000000000000000000, 1.000000000000000000, -0.000000000000000000 ) ) ;
#23769 = DIRECTION ( 'NONE',  ( -3.469446951953613696E-16, 0.000000000000000000, -1.000000000000000000 ) ) ;
#23770 = EDGE_CURVE ( 'NONE', #17416, #47487, #1891, .T. ) ;
#23771 = DIRECTION ( 'NONE',  ( -0.000000000000000000, 1.000000000000000000, -0.000000000000000000 ) ) ;
#23772 = CARTESIAN_POINT ( 'NONE',  ( 1.636583440222563857, 0.000000000000000000, 0.1181102362204701633 ) ) ;
#23773 = ORIENTED_EDGE ( 'NONE', *, *, #18697, .T. ) ;
#23774 = VERTEX_POINT ( 'NONE', #37525 ) ;
#23775 = LINE ( 'NONE', #35401, #6532 ) ;
#23776 = LINE ( 'NONE', #19886, #31729 ) ;
#23777 = ORIENTED_EDGE ( 'NONE', *, *, #4640, .F. ) ;
#23778 = ADVANCED_FACE ( 'NONE', ( #36055 ), #935, .F. ) ;
#23779 = LINE ( 'NONE', #19638, #49840 ) ;
#23780 = CARTESIAN_POINT ( 'NONE',  ( -1.712496953225537633, 3.267716535433071279, 1.220472440944875059 ) ) ;
#23781 = VECTOR ( 'NONE', #34743, 39.37007874015748143 ) ;
#23782 = DIRECTION ( 'NONE',  ( -0.000000000000000000, 1.000000000000000000, -0.000000000000000000 ) ) ;
#23783 = DIRECTION ( 'NONE',  ( -3.469446951953613696E-16, 0.000000000000000000, -1.000000000000000000 ) ) ;
#23784 = FACE_OUTER_BOUND ( 'NONE', #9997, .T. ) ;
#23785 = EDGE_LOOP ( 'NONE', ( #36082, #19171, #9115, #27506 ) ) ;
#23786 = DIRECTION ( 'NONE',  ( -0.000000000000000000, 1.000000000000000000, -0.000000000000000000 ) ) ;
#23787 = CARTESIAN_POINT ( 'NONE',  ( -0.7874015748031493178, 0.000000000000000000, -1.968503937007874072 ) ) ;
#23788 = VECTOR ( 'NONE', #47187, 39.37007874015748143 ) ;
#23789 = ORIENTED_EDGE ( 'NONE', *, *, #26537, .F. ) ;
#23790 = ORIENTED_EDGE ( 'NONE', *, *, #32887, .T. ) ;
#23792 = DIRECTION ( 'NONE',  ( 0.000000000000000000, -1.000000000000000000, 0.000000000000000000 ) ) ;
#23791 = CIRCLE ( 'NONE', #1546, 2.165354330708661568 ) ;
#23793 = FACE_OUTER_BOUND ( 'NONE', #41997, .T. ) ;
#23794 = CARTESIAN_POINT ( 'NONE',  ( 2.576863348864710801, 0.000000000000000000, 1.442554885838449819 ) ) ;
#23795 = ORIENTED_EDGE ( 'NONE', *, *, #3013, .F. ) ;
#23796 = VECTOR ( 'NONE', #6962, 39.37007874015748143 ) ;
#23797 = ORIENTED_EDGE ( 'NONE', *, *, #35713, .F. ) ;
#23798 = CARTESIAN_POINT ( 'NONE',  ( 0.4696143004045484348, 3.267716535433071279, 1.220472440944875281 ) ) ;
#23799 = ORIENTED_EDGE ( 'NONE', *, *, #37248, .T. ) ;
#23800 = CIRCLE ( 'NONE', #11425, 2.106299212598425008 ) ;
#23801 = DIRECTION ( 'NONE',  ( -3.986037398843765983E-20, -1.000000000000000000, -1.160734090543304660E-16 ) ) ;
#23802 = ORIENTED_EDGE ( 'NONE', *, *, #113, .F. ) ;
#23803 = EDGE_CURVE ( 'NONE', #5523, #17338, #17638, .T. ) ;
#23804 = CARTESIAN_POINT ( 'NONE',  ( 0.5455278134075212115, 3.267716535433071279, -0.3149606299212593941 ) ) ;
#23805 = CARTESIAN_POINT ( 'NONE',  ( 0.5544985201248122664, 1.716783259433079856, -2.194164409418295048 ) ) ;
#23806 = CARTESIAN_POINT ( 'NONE',  ( 0.000000000000000000, 3.267716535433071279, -0.3543307086614174151 ) ) ;
#23807 = ADVANCED_FACE ( 'NONE', ( #17895 ), #40185, .T. ) ;
#23808 = EDGE_CURVE ( 'NONE', #33436, #24648, #2149, .T. ) ;
#23809 = EDGE_LOOP ( 'NONE', ( #16758, #555, #16583, #42520, #31112 ) ) ;
#23810 = VERTEX_POINT ( 'NONE', #28292 ) ;
#23811 = EDGE_LOOP ( 'NONE', ( #35090, #11050, #14341, #34565, #37955, #26264, #21497, #45028 ) ) ;
#23812 = DIRECTION ( 'NONE',  ( 1.734723475976806848E-16, -0.000000000000000000, 1.000000000000000000 ) ) ;
#23813 = CARTESIAN_POINT ( 'NONE',  ( -1.363819533518803473, 3.232777166330603524, 2.047244094488179567 ) ) ;
#23814 = ORIENTED_EDGE ( 'NONE', *, *, #50798, .F. ) ;
#23815 = ORIENTED_EDGE ( 'NONE', *, *, #41542, .T. ) ;
#23816 = DIRECTION ( 'NONE',  ( 1.606762707810401785E-15, -0.7071067811865483499, 0.7071067811865466846 ) ) ;
#23817 = DIRECTION ( 'NONE',  ( -1.000000000000000000, 0.000000000000000000, -0.000000000000000000 ) ) ;
#23818 = DIRECTION ( 'NONE',  ( -1.000000000000000000, -0.000000000000000000, -0.000000000000000000 ) ) ;
#23819 = ORIENTED_EDGE ( 'NONE', *, *, #45589, .F. ) ;
#23820 = DIRECTION ( 'NONE',  ( -0.8345732537213079727, -6.391122427287080193E-17, 0.5508969814520945363 ) ) ;
#23821 = CARTESIAN_POINT ( 'NONE',  ( 0.000000000000000000, 3.346456692913386100, 0.000000000000000000 ) ) ;
#23822 = CIRCLE ( 'NONE', #27944, 1.743387098533651480 ) ;
#23823 = CARTESIAN_POINT ( 'NONE',  ( 1.015142113812069313, 0.000000000000000000, -0.4724409448818889246 ) ) ;
#23824 = ORIENTED_EDGE ( 'NONE', *, *, #29200, .T. ) ;
#23825 = CARTESIAN_POINT ( 'NONE',  ( 1.363819533518803251, 0.000000000000000000, 0.9055118110236164419 ) ) ;
#23826 = PLANE ( 'NONE',  #32679 ) ;
#23827 = EDGE_LOOP ( 'NONE', ( #46956, #38738, #48243, #12828 ) ) ;
#23828 = CARTESIAN_POINT ( 'NONE',  ( -1.236813753895212642, 1.541669022091038732, -2.681693691597581974 ) ) ;
#23829 = ORIENTED_EDGE ( 'NONE', *, *, #48430, .T. ) ;
#23830 = ORIENTED_EDGE ( 'NONE', *, *, #49301, .T. ) ;
#23831 = CARTESIAN_POINT ( 'NONE',  ( 0.1968503937007872462, 0.000000000000000000, 0.4330708661417287386 ) ) ;
#23832 = CARTESIAN_POINT ( 'NONE',  ( -0.9106291036520693938, 1.598827635308956108, 2.286305300140973440 ) ) ;
#23833 = VECTOR ( 'NONE', #13739, 39.37007874015748143 ) ;
#23834 = AXIS2_PLACEMENT_3D ( 'NONE', #2201, #18454, #49644 ) ;
#23835 = CARTESIAN_POINT ( 'NONE',  ( 1.287906020515830141, 3.267716535433071279, -4.468321617281355077E-16 ) ) ;
#23836 = ADVANCED_FACE ( 'NONE', ( #5765 ), #44038, .F. ) ;
#23837 = CARTESIAN_POINT ( 'NONE',  ( -1.930378847043046964, 1.689166098830295892, 2.234429243796722808 ) ) ;
#23839 = AXIS2_PLACEMENT_3D ( 'NONE', #16642, #50919, #4503 ) ;
#23838 = CARTESIAN_POINT ( 'NONE',  ( 1.461363083917469829, 1.574803149606302854, 1.597866488315584865 ) ) ;
#23840 = ORIENTED_EDGE ( 'NONE', *, *, #33162, .T. ) ;
#23841 = VERTEX_POINT ( 'NONE', #13769 ) ;
#23842 = VECTOR ( 'NONE', #11230, 39.37007874015748143 ) ;
#23843 = ORIENTED_EDGE ( 'NONE', *, *, #8020, .T. ) ;
#23844 = DIRECTION ( 'NONE',  ( 0.000000000000000000, 0.000000000000000000, -1.000000000000000000 ) ) ;
#23845 = EDGE_CURVE ( 'NONE', #32006, #49770, #14271, .T. ) ;
#23846 = CARTESIAN_POINT ( 'NONE',  ( -1.252056778656947422, 1.687847970117562602, -1.807033786809818077 ) ) ;
#23847 = EDGE_CURVE ( 'NONE', #47727, #25120, #30020, .T. ) ;
#23848 = DIRECTION ( 'NONE',  ( 1.000000000000000000, 0.000000000000000000, 0.000000000000000000 ) ) ;
#23849 = DIRECTION ( 'NONE',  ( 1.160734090543304660E-16, -1.000000000000000000, -0.000000000000000000 ) ) ;
#23850 = VERTEX_POINT ( 'NONE', #20293 ) ;
#23851 = DIRECTION ( 'NONE',  ( 0.9998717552508121775, 0.01601477604151182663, 0.000000000000000000 ) ) ;
#23852 = EDGE_CURVE ( 'NONE', #28934, #44754, #21510, .T. ) ;
#23853 = PLANE ( 'NONE',  #50388 ) ;
#23854 = EDGE_CURVE ( 'NONE', #34255, #32050, #679, .T. ) ;
#23855 = EDGE_LOOP ( 'NONE', ( #3438, #24132, #27847, #16159 ) ) ;
#23856 = CARTESIAN_POINT ( 'NONE',  ( 2.932638728931774352, 1.764957438482779528, 0.3475908556738225297 ) ) ;
#23857 = CARTESIAN_POINT ( 'NONE',  ( -1.229551338856769371, 1.049866565067838264, -1.608606759830606858 ) ) ;
#23858 =( BOUNDED_CURVE ( )  B_SPLINE_CURVE ( 3, ( #17778, #25269, #41027, #25521 ),
 .UNSPECIFIED., .F., .F. ) 
 B_SPLINE_CURVE_WITH_KNOTS ( ( 4, 4 ),
 ( 2.000194674521101224, 2.051115727886003270 ),
 .UNSPECIFIED. ) 
 CURVE ( )  GEOMETRIC_REPRESENTATION_ITEM ( )  RATIONAL_B_SPLINE_CURVE ( ( 1.000000000000000000, 0.9997839321993498007, 0.9997839321993498007, 1.000000000000000000 ) ) 
 REPRESENTATION_ITEM ( '' )  );
#23859 = LINE ( 'NONE', #30282, #47685 ) ;
#23860 = VECTOR ( 'NONE', #16147, 39.37007874015748143 ) ;
#23861 = VERTEX_POINT ( 'NONE', #28548 ) ;
#23862 = CARTESIAN_POINT ( 'NONE',  ( -1.735432873265435161, 1.581680620477750931, 1.321016258651915409 ) ) ;
#23863 = LINE ( 'NONE', #4500, #11817 ) ;
#23864 = CARTESIAN_POINT ( 'NONE',  ( 2.623503965249849301, 1.455362298632098428, 1.355882097269874187 ) ) ;
#23865 = ORIENTED_EDGE ( 'NONE', *, *, #26200, .T. ) ;
#23866 = PLANE ( 'NONE',  #23839 ) ;
#23867 = DIRECTION ( 'NONE',  ( -0.000000000000000000, -1.000000000000000000, -0.000000000000000000 ) ) ;
#23868 = VERTEX_POINT ( 'NONE', #18149 ) ;
#23869 = DIRECTION ( 'NONE',  ( 1.042246309067994810E-16, 1.000000000000000000, 7.572362681945316160E-17 ) ) ;
#23870 = EDGE_CURVE ( 'NONE', #33556, #11186, #45737, .T. ) ;
#23871 = AXIS2_PLACEMENT_3D ( 'NONE', #4665, #40298, #20407 ) ;
#23872 = CARTESIAN_POINT ( 'NONE',  ( -1.145994540540797635, 0.003253507172150460220, 1.386494442623789070 ) ) ;
#23873 = DIRECTION ( 'NONE',  ( -1.000000000000000000, 0.000000000000000000, 0.000000000000000000 ) ) ;
#23874 = CARTESIAN_POINT ( 'NONE',  ( 1.909347346926324684, 3.346456692913386100, -0.1574803149606304187 ) ) ;
#23875 = EDGE_CURVE ( 'NONE', #31767, #44945, #45013, .T. ) ;
#23876 = MANIFOLD_SOLID_BREP ( 'Cut-Revolve2', #11415 ) ;
#23877 = ORIENTED_EDGE ( 'NONE', *, *, #38867, .F. ) ;
#23878 = VERTEX_POINT ( 'NONE', #49842 ) ;
#23879 = DIRECTION ( 'NONE',  ( -0.000000000000000000, -1.000000000000000000, -0.000000000000000000 ) ) ;
#23880 = CARTESIAN_POINT ( 'NONE',  ( 1.909347346926324684, 3.346456692913386100, -0.3543307086614178592 ) ) ;
#23881 = ORIENTED_EDGE ( 'NONE', *, *, #26822, .T. ) ;
#23882 = DIRECTION ( 'NONE',  ( -0.000000000000000000, 1.000000000000000000, -0.000000000000000000 ) ) ;
#23883 = CARTESIAN_POINT ( 'NONE',  ( 1.560669927219590747, 3.267716535433071279, 0.4724409448818871482 ) ) ;
#23884 = AXIS2_PLACEMENT_3D ( 'NONE', #8044, #43656, #44173 ) ;
#23885 = CARTESIAN_POINT ( 'NONE',  ( -0.8182917201112814842, 0.000000000000000000, 1.535433070866133898 ) ) ;
#23886 = CARTESIAN_POINT ( 'NONE',  ( 1.833433833923351353, 3.267716535433071279, -6.361001426713998480E-16 ) ) ;
#23887 = ORIENTED_EDGE ( 'NONE', *, *, #17622, .T. ) ;
#23888 = ORIENTED_EDGE ( 'NONE', *, *, #5928, .T. ) ;
#23889 = ORIENTED_EDGE ( 'NONE', *, *, #18084, .T. ) ;
#23890 = DIRECTION ( 'NONE',  ( 0.000000000000000000, -1.000000000000000000, 0.000000000000000000 ) ) ;
#23891 = LINE ( 'NONE', #28010, #38722 ) ;
#23892 = DIRECTION ( 'NONE',  ( -1.000000000000000000, 0.000000000000000000, 1.734723475976806848E-16 ) ) ;
#23893 = FACE_BOUND ( 'NONE', #41363, .T. ) ;
#23894 = ORIENTED_EDGE ( 'NONE', *, *, #28460, .T. ) ;
#23895 = CARTESIAN_POINT ( 'NONE',  ( -1.363819533518803473, 3.346456692913386100, 1.681890501046756192 ) ) ;
#23896 = ORIENTED_EDGE ( 'NONE', *, *, #49959, .T. ) ;
#23897 = VERTEX_POINT ( 'NONE', #37780 ) ;
#23898 = DIRECTION ( 'NONE',  ( -3.986037398843765983E-20, -1.000000000000000000, -1.160734090543304660E-16 ) ) ;
#23899 = VECTOR ( 'NONE', #34445, 39.37007874015748143 ) ;
#23900 = ORIENTED_EDGE ( 'NONE', *, *, #28651, .F. ) ;
#23902 = ORIENTED_EDGE ( 'NONE', *, *, #20404, .T. ) ;
#23901 = EDGE_CURVE ( 'NONE', #20171, #6948, #18403, .T. ) ;
#23903 = DIRECTION ( 'NONE',  ( 1.734723475976806848E-16, -0.000000000000000000, 1.000000000000000000 ) ) ;
#23904 = VERTEX_POINT ( 'NONE', #3155 ) ;
#23905 = CARTESIAN_POINT ( 'NONE',  ( -1.363819533518803029, 3.346456692913386100, 1.220472440944875281 ) ) ;
#23906 = LINE ( 'NONE', #4285, #21971 ) ;
#23907 = DIRECTION ( 'NONE',  ( 0.01601477604151182663, -0.9998717552508123996, 0.000000000000000000 ) ) ;
#23908 = VECTOR ( 'NONE', #2833, 39.37007874015748143 ) ;
#23909 = AXIS2_PLACEMENT_3D ( 'NONE', #23081, #38829, #17118 ) ;
#23910 = EDGE_CURVE ( 'NONE', #48435, #13777, #26893, .T. ) ;
#23911 = ADVANCED_FACE ( 'NONE', ( #14783 ), #42139, .F. ) ;
#23912 = PLANE ( 'NONE',  #38796 ) ;
#23913 = EDGE_CURVE ( 'NONE', #12429, #17233, #27691, .T. ) ;
#23914 = DIRECTION ( 'NONE',  ( 0.7071067811865483499, -0.000000000000000000, 0.7071067811865466846 ) ) ;
#23915 = LINE ( 'NONE', #32185, #2296 ) ;
#23916 = EDGE_LOOP ( 'NONE', ( #44530, #43648, #31266, #27057 ) ) ;
#23917 = FACE_OUTER_BOUND ( 'NONE', #38452, .T. ) ;
#23918 = VECTOR ( 'NONE', #20177, 39.37007874015748143 ) ;
#23919 = CARTESIAN_POINT ( 'NONE',  ( -3.073077335812187894, 5.118110236220475784, 0.6509316561051814443 ) ) ;
#23920 = DIRECTION ( 'NONE',  ( -3.469446951953613696E-16, 0.000000000000000000, -1.000000000000000000 ) ) ;
#23921 = ORIENTED_EDGE ( 'NONE', *, *, #43831, .F. ) ;
#23922 = CARTESIAN_POINT ( 'NONE',  ( -0.4350747367504783636, 0.000000000000000000, -2.121846421795421378 ) ) ;
#23923 = CARTESIAN_POINT ( 'NONE',  ( 1.062992125984251413, 0.4724409448818890911, -1.181102362204724754 ) ) ;
#23924 = ORIENTED_EDGE ( 'NONE', *, *, #28226, .F. ) ;
#23925 = CARTESIAN_POINT ( 'NONE',  ( 1.747029694980739345, 6.692913385826772199, 1.330264415365525421 ) ) ;
#23926 = CARTESIAN_POINT ( 'NONE',  ( 2.875072944275708586, 1.448522234753447657, -0.6730469799666056741 ) ) ;
#23927 = LINE ( 'NONE', #8689, #49843 ) ;
#23928 = CARTESIAN_POINT ( 'NONE',  ( 2.017818867441111497, 0.03950160972893088096, -0.04135814764324683562 ) ) ;
#23929 = EDGE_CURVE ( 'NONE', #12139, #50226, #31033, .T. ) ;
#23930 = ORIENTED_EDGE ( 'NONE', *, *, #40432, .T. ) ;
#23931 = CARTESIAN_POINT ( 'NONE',  ( 0.000000000000000000, 3.267716535433071279, -0.1968503937007881899 ) ) ;
#23932 = DIRECTION ( 'NONE',  ( -0.9998717552508122886, -0.01601477604151182316, 0.000000000000000000 ) ) ;
#23933 = EDGE_CURVE ( 'NONE', #49753, #34884, #3786, .T. ) ;
#23934 = LINE ( 'NONE', #16712, #28396 ) ;
#23935 = CARTESIAN_POINT ( 'NONE',  ( 1.560669927219590747, 3.346456692913386100, 0.7874015748031454320 ) ) ;
#23936 = ORIENTED_EDGE ( 'NONE', *, *, #6201, .F. ) ;
#23937 = EDGE_CURVE ( 'NONE', #27371, #48222, #11156, .T. ) ;
#23938 = ORIENTED_EDGE ( 'NONE', *, *, #18202, .T. ) ;
#23939 = EDGE_LOOP ( 'NONE', ( #4691, #29304, #25008, #37417 ) ) ;
#23940 = LINE ( 'NONE', #12578, #688 ) ;
#23941 = EDGE_CURVE ( 'NONE', #45425, #49792, #2652, .T. ) ;
#23942 = VERTEX_POINT ( 'NONE', #46242 ) ;
#23943 = DIRECTION ( 'NONE',  ( -0.000000000000000000, -1.000000000000000000, -0.000000000000000000 ) ) ;
#23944 = PLANE ( 'NONE',  #1327 ) ;
#23945 = ORIENTED_EDGE ( 'NONE', *, *, #14972, .T. ) ;
#23946 = VECTOR ( 'NONE', #48636, 39.37007874015748143 ) ;
#23947 = CARTESIAN_POINT ( 'NONE',  ( 1.282536922928985357, 3.255655746335629708, -2.086614173228339641 ) ) ;
#23948 = AXIS2_PLACEMENT_3D ( 'NONE', #38172, #22164, #18791 ) ;
#23949 = VERTEX_POINT ( 'NONE', #15032 ) ;
#23950 = CARTESIAN_POINT ( 'NONE',  ( -0.8182917201112819283, 0.000000000000000000, -0.9842519685039342603 ) ) ;
#23951 = DIRECTION ( 'NONE',  ( -1.000000000000000000, 0.000000000000000000, 0.000000000000000000 ) ) ;
#23952 = VERTEX_POINT ( 'NONE', #42887 ) ;
#23953 = DIRECTION ( 'NONE',  ( -1.000000000000000000, 0.000000000000000000, -0.000000000000000000 ) ) ;
#23954 = ORIENTED_EDGE ( 'NONE', *, *, #1185, .T. ) ;
#23955 = VECTOR ( 'NONE', #4895, 39.37007874015748143 ) ;
#23956 = CARTESIAN_POINT ( 'NONE',  ( -1.220415235146723676, 0.5160455853568218787, -0.4330136603435745246 ) ) ;
#23957 = VERTEX_POINT ( 'NONE', #10902 ) ;
#23958 = ORIENTED_EDGE ( 'NONE', *, *, #25856, .F. ) ;
#23959 = LINE ( 'NONE', #32228, #14950 ) ;
#23960 = LINE ( 'NONE', #4596, #32823 ) ;
#23961 = VERTEX_POINT ( 'NONE', #38289 ) ;
#23962 = CARTESIAN_POINT ( 'NONE',  ( -1.091055626815042645, 0.000000000000000000, -1.889763779527552146 ) ) ;
#23963 = ORIENTED_EDGE ( 'NONE', *, *, #34725, .F. ) ;
#23964 = CARTESIAN_POINT ( 'NONE',  ( 0.8182917201112824834, 3.346456692913386100, 2.047244094488179567 ) ) ;
#23965 = PLANE ( 'NONE',  #43129 ) ;
#23966 = ADVANCED_FACE ( 'NONE', ( #50587 ), #46610, .T. ) ;
#23967 = DIRECTION ( 'NONE',  ( -3.469446951953613696E-16, 0.000000000000000000, -1.000000000000000000 ) ) ;
#23968 = ORIENTED_EDGE ( 'NONE', *, *, #2265, .T. ) ;
#23969 = VERTEX_POINT ( 'NONE', #18661 ) ;
#23970 = EDGE_CURVE ( 'NONE', #216, #47008, #7535, .T. ) ;
#23971 = CARTESIAN_POINT ( 'NONE',  ( 0.4330136603435738585, 0.5160455853568214346, -1.535490276664301046 ) ) ;
#23972 = DIRECTION ( 'NONE',  ( -8.021399753802077430E-17, -1.000000000000000000, -8.389726389140663754E-17 ) ) ;
#23973 = EDGE_CURVE ( 'NONE', #50189, #14529, #30780, .T. ) ;
#23974 = CARTESIAN_POINT ( 'NONE',  ( 1.836043989102772445, 1.744310788554293890, 2.026723291277686467 ) ) ;
#23975 = CARTESIAN_POINT ( 'NONE',  ( -1.863748091109392879, 3.267716535433071279, 1.102362204724404160 ) ) ;
#23976 = EDGE_CURVE ( 'NONE', #34134, #16416, #50704, .T. ) ;
#23977 = CARTESIAN_POINT ( 'NONE',  ( -1.779568955232875060, 1.574803149606302854, -1.233650562797313555 ) ) ;
#23978 = VECTOR ( 'NONE', #33842, 39.37007874015748143 ) ;
#23979 = CONICAL_SURFACE ( 'NONE', #9131, 2.244934639244524632, 1.554780866114618743 ) ;
#23980 = CARTESIAN_POINT ( 'NONE',  ( 0.000000000000000000, 3.346456692913386100, 0.000000000000000000 ) ) ;
#23981 = VERTEX_POINT ( 'NONE', #39031 ) ;
#23982 = PLANE ( 'NONE',  #30850 ) ;
#23983 = ORIENTED_EDGE ( 'NONE', *, *, #13164, .F. ) ;
#23984 = DIRECTION ( 'NONE',  ( -0.000000000000000000, 1.000000000000000000, -0.000000000000000000 ) ) ;
#23985 = VECTOR ( 'NONE', #33498, 39.37007874015748143 ) ;
#23986 = EDGE_CURVE ( 'NONE', #43399, #32147, #3662, .T. ) ;
#23987 = ORIENTED_EDGE ( 'NONE', *, *, #46676, .T. ) ;
#23988 = CARTESIAN_POINT ( 'NONE',  ( -0.5286458662987743029, 0.000000000000000000, 2.100489422084707680 ) ) ;
#23989 = CARTESIAN_POINT ( 'NONE',  ( -0.5455278134075214336, 3.267716535433071279, 2.095509194042718182 ) ) ;
#23990 = EDGE_CURVE ( 'NONE', #13855, #23569, #8038, .T. ) ;
#23991 = DIRECTION ( 'NONE',  ( 1.000000000000000000, 0.000000000000000000, 0.000000000000000000 ) ) ;
#23992 = VERTEX_POINT ( 'NONE', #3918 ) ;
#23993 = CARTESIAN_POINT ( 'NONE',  ( 0.8454231601665999074, 1.623017753118757067, 2.112564685048140323 ) ) ;
#23994 = EDGE_CURVE ( 'NONE', #41081, #13698, #28416, .T. ) ;
#23995 = ORIENTED_EDGE ( 'NONE', *, *, #39029, .F. ) ;
#23996 = DIRECTION ( 'NONE',  ( -1.000000000000000000, 0.000000000000000000, -0.000000000000000000 ) ) ;
#23997 = ORIENTED_EDGE ( 'NONE', *, *, #18708, .F. ) ;
#23998 = CARTESIAN_POINT ( 'NONE',  ( 2.755905511811024056, 4.960629921259846142, 1.023622047244094446 ) ) ;
#23999 = DIRECTION ( 'NONE',  ( -7.460697193978162709E-14, 0.000000000000000000, 1.000000000000000000 ) ) ;
#24000 = LINE ( 'NONE', #4385, #17280 ) ;
#24001 = VERTEX_POINT ( 'NONE', #47750 ) ;
#24002 = ORIENTED_EDGE ( 'NONE', *, *, #38311, .T. ) ;
#24003 = CARTESIAN_POINT ( 'NONE',  ( 0.000000000000000000, 1.574803149606302854, 0.000000000000000000 ) ) ;
#24004 = LINE ( 'NONE', #20388, #42154 ) ;
#24005 = DIRECTION ( 'NONE',  ( 1.000000000000000000, -0.000000000000000000, 0.000000000000000000 ) ) ;
#24006 = VECTOR ( 'NONE', #32489, 39.37007874015748143 ) ;
#24007 = AXIS2_PLACEMENT_3D ( 'NONE', #31934, #19777, #23920 ) ;
#24008 = ORIENTED_EDGE ( 'NONE', *, *, #18560, .T. ) ;
#24009 = VECTOR ( 'NONE', #41240, 39.37007874015748143 ) ;
#24010 = DIRECTION ( 'NONE',  ( -1.000000000000000000, 0.000000000000000000, 1.734723475976806848E-16 ) ) ;
#24011 = CARTESIAN_POINT ( 'NONE',  ( -1.636583440222564301, 3.267716535433071279, -0.8267716535433052849 ) ) ;
#24012 = ORIENTED_EDGE ( 'NONE', *, *, #19309, .T. ) ;
#24013 = CARTESIAN_POINT ( 'NONE',  ( 2.164971648505046975, 6.332733149760729319, -0.04070796836118365652 ) ) ;
#24014 = CIRCLE ( 'NONE', #42257, 2.443628662382284489 ) ;
#24015 = VERTEX_POINT ( 'NONE', #288 ) ;
#24016 = VERTEX_POINT ( 'NONE', #47238 ) ;
#24017 = VECTOR ( 'NONE', #49557, 39.37007874015748143 ) ;
#24018 = ITEM_DEFINED_TRANSFORMATION ( 'NONE', 'NONE', #348,  #26741 ) ;
#24019 = VERTEX_POINT ( 'NONE', #40048 ) ;
#24020 = CARTESIAN_POINT ( 'NONE',  ( -0.8942052331142552601, 3.346456692913386100, -1.972094414217999914 ) ) ;
#24021 = AXIS2_PLACEMENT_3D ( 'NONE', #45053, #29585, #41457 ) ;
#24022 = DIRECTION ( 'NONE',  ( -0.01601477604151182663, 0.9998717552508123996, -0.000000000000000000 ) ) ;
#24023 = DIRECTION ( 'NONE',  ( -1.000000000000000000, 0.000000000000000000, 1.734723475976806848E-16 ) ) ;
#24024 = FACE_OUTER_BOUND ( 'NONE', #35754, .T. ) ;
#24025 = VERTEX_POINT ( 'NONE', #15779 ) ;
#24026 = EDGE_LOOP ( 'NONE', ( #15723, #32999, #48284, #33074 ) ) ;
#24027 = EDGE_CURVE ( 'NONE', #22069, #47632, #12167, .T. ) ;
#24028 = CARTESIAN_POINT ( 'NONE',  ( -1.525880051666119286, 0.002351180378572883568, 0.8769966569942660994 ) ) ;
#24029 = SURFACE_STYLE_FILL_AREA ( #12411 ) ;
#24030 = EDGE_CURVE ( 'NONE', #14938, #46382, #11910, .T. ) ;
#24031 = DIRECTION ( 'NONE',  ( -0.000000000000000000, 1.000000000000000000, -0.000000000000000000 ) ) ;
#24032 = ORIENTED_EDGE ( 'NONE', *, *, #41954, .F. ) ;
#24033 = CARTESIAN_POINT ( 'NONE',  ( 0.7423782071083085965, 3.346456692913386100, 0.4330708661417287386 ) ) ;
#24034 = EDGE_CURVE ( 'NONE', #47245, #49325, #16042, .T. ) ;
#24035 = CARTESIAN_POINT ( 'NONE',  ( 1.287906020515830363, 3.267716535433071279, -4.468321617281356063E-16 ) ) ;
#24036 = DIRECTION ( 'NONE',  ( 1.000000000000000000, 0.000000000000000000, 0.000000000000000000 ) ) ;
#24037 = EDGE_CURVE ( 'NONE', #16050, #1443, #31798, .T. ) ;
#24038 = DIRECTION ( 'NONE',  ( 1.734723475976806848E-16, -0.000000000000000000, 1.000000000000000000 ) ) ;
#24039 = CARTESIAN_POINT ( 'NONE',  ( 2.339241080213585899, 1.657243480315735873, 1.802537235681917815 ) ) ;
#24040 = MANIFOLD_SOLID_BREP ( 'Extrude-Thin1', #8098 ) ;
#24041 = ORIENTED_EDGE ( 'NONE', *, *, #40733, .F. ) ;
#24042 = DIRECTION ( 'NONE',  ( -0.04261736568783053986, 0.000000000000000000, -0.9990914673551313241 ) ) ;
#24043 = FILL_AREA_STYLE_COLOUR ( '', #12039 ) ;
#24044 = ORIENTED_EDGE ( 'NONE', *, *, #24999, .F. ) ;
#24045 = VECTOR ( 'NONE', #4231, 39.37007874015748854 ) ;
#24046 = VERTEX_POINT ( 'NONE', #16301 ) ;
#24047 = CARTESIAN_POINT ( 'NONE',  ( 1.636583440222563857, 0.000000000000000000, 1.259842519685033135 ) ) ;
#24048 = CARTESIAN_POINT ( 'NONE',  ( -0.8942052331142552601, 0.000000000000000000, -1.574803149606293529 ) ) ;
#24049 = EDGE_CURVE ( 'NONE', #4787, #30956, #39281, .T. ) ;
#24050 = PLANE ( 'NONE',  #10702 ) ;
#24051 = ORIENTED_EDGE ( 'NONE', *, *, #14138, .T. ) ;
#24052 = AXIS2_PLACEMENT_3D ( 'NONE', #17667, #21796, #41169 ) ;
#24053 = EDGE_CURVE ( 'NONE', #30992, #20081, #36184, .T. ) ;
#24054 = ORIENTED_EDGE ( 'NONE', *, *, #13841, .T. ) ;
#24055 = CARTESIAN_POINT ( 'NONE',  ( -1.636583440222564301, 0.000000000000000000, -0.5118110236220466680 ) ) ;
#24056 = CONICAL_SURFACE ( 'NONE', #44648, 2.244934639244524632, 1.554780866114618743 ) ;
#24057 = ORIENTED_EDGE ( 'NONE', *, *, #15804, .F. ) ;
#24058 = DIRECTION ( 'NONE',  ( -0.000000000000000000, 1.000000000000000000, -0.000000000000000000 ) ) ;
#24059 = EDGE_LOOP ( 'NONE', ( #7385, #9340, #754, #19599, #5613, #12133, #816, #46255, #1898, #35892, #19040 ) ) ;
#24060 = VECTOR ( 'NONE', #32904, 39.37007874015748143 ) ;
#24061 = CARTESIAN_POINT ( 'NONE',  ( 0.6507993007407579800, 1.619900495825837838, -2.173134161263437392 ) ) ;
#24062 = DIRECTION ( 'NONE',  ( -1.000000000000000000, 0.000000000000000000, 1.734723475976806848E-16 ) ) ;
#24063 = CARTESIAN_POINT ( 'NONE',  ( -1.159317824364283211, 0.5241370646666094757, 1.844421372722656161 ) ) ;
#24064 = ORIENTED_EDGE ( 'NONE', *, *, #6091, .T. ) ;
#24065 = ORIENTED_EDGE ( 'NONE', *, *, #35845, .T. ) ;
#24066 = VERTEX_POINT ( 'NONE', #12683 ) ;
#24067 = DIRECTION ( 'NONE',  ( -0.000000000000000000, 1.000000000000000000, -0.000000000000000000 ) ) ;
#24068 = FACE_OUTER_BOUND ( 'NONE', #25622, .T. ) ;
#24069 = ORIENTED_EDGE ( 'NONE', *, *, #16779, .F. ) ;
#24070 = ORIENTED_EDGE ( 'NONE', *, *, #21545, .F. ) ;
#24071 = CARTESIAN_POINT ( 'NONE',  ( 0.8182917201112824834, 0.000000000000000000, 2.047244094488179567 ) ) ;
#24072 = FACE_OUTER_BOUND ( 'NONE', #31324, .T. ) ;
#24073 = CARTESIAN_POINT ( 'NONE',  ( 0.000000000000000000, 0.000000000000000000, 0.000000000000000000 ) ) ;
#24074 = EDGE_CURVE ( 'NONE', #9880, #11936, #20676, .T. ) ;
#24075 = ORIENTED_EDGE ( 'NONE', *, *, #25968, .T. ) ;
#24076 = VERTEX_POINT ( 'NONE', #27394 ) ;
#24077 = DIRECTION ( 'NONE',  ( -0.000000000000000000, -1.000000000000000000, -0.000000000000000000 ) ) ;
#24078 = CARTESIAN_POINT ( 'NONE',  ( -0.6584127755596833609, 0.000000000000000000, 1.614277297217976859 ) ) ;
#24079 = CARTESIAN_POINT ( 'NONE',  ( 0.000000000000000000, 3.267716535433071279, 1.732283464566920950 ) ) ;
#24080 = ORIENTED_EDGE ( 'NONE', *, *, #39996, .T. ) ;
#24081 = FACE_OUTER_BOUND ( 'NONE', #3201, .T. ) ;
#24082 = LINE ( 'NONE', #5224, #45025 ) ;
#24083 = EDGE_LOOP ( 'NONE', ( #29100, #22809, #44283, #49930 ) ) ;
#24084 = CARTESIAN_POINT ( 'NONE',  ( -2.947574761915765063, 5.905511811023623991, -0.1816379373805338815 ) ) ;
#24085 = ORIENTED_EDGE ( 'NONE', *, *, #15972, .T. ) ;
#24086 = VERTEX_POINT ( 'NONE', #23524 ) ;
#24087 = CARTESIAN_POINT ( 'NONE',  ( 0.000000000000000000, 3.267716535433071279, -0.1968503937007880511 ) ) ;
#24088 = LENGTH_MEASURE_WITH_UNIT ( LENGTH_MEASURE( 0.02539999999999999897 ), #12465 );
#24090 = CIRCLE ( 'NONE', #1834, 2.165354330708661568 ) ;
#24089 = DIRECTION ( 'NONE',  ( -1.000000000000000000, 0.000000000000000000, -0.000000000000000000 ) ) ;
#24091 = DIRECTION ( 'NONE',  ( 0.000000000000000000, 1.000000000000000000, -0.000000000000000000 ) ) ;
#24092 = CARTESIAN_POINT ( 'NONE',  ( -0.8942052331142552601, 3.346456692913386100, -0.3149606299212593941 ) ) ;
#24093 = ORIENTED_EDGE ( 'NONE', *, *, #48615, .F. ) ;
#24094 = ORIENTED_EDGE ( 'NONE', *, *, #11138, .T. ) ;
#24095 = CIRCLE ( 'NONE', #36447, 2.165354330708661568 ) ;
#24096 = EDGE_CURVE ( 'NONE', #16446, #45550, #19646, .T. ) ;
#24097 = ORIENTED_EDGE ( 'NONE', *, *, #46295, .T. ) ;
#24098 = DIRECTION ( 'NONE',  ( -0.6427876096865403621, -0.7660444431189770143, 0.000000000000000000 ) ) ;
#24099 = LINE ( 'NONE', #31861, #42400 ) ;
#24100 = EDGE_CURVE ( 'NONE', #3033, #45153, #1316, .T. ) ;
#24101 = AXIS2_PLACEMENT_3D ( 'NONE', #4569, #19787, #20308 ) ;
#24102 = ADVANCED_FACE ( 'NONE', ( #37471 ), #18646, .T. ) ;
#24103 = EDGE_CURVE ( 'NONE', #44707, #2087, #44424, .T. ) ;
#24104 = CARTESIAN_POINT ( 'NONE',  ( -1.936609506549060722, 1.676883605369557051, 0.9862484270667263297 ) ) ;
#24105 = CARTESIAN_POINT ( 'NONE',  ( -2.152441353505195387, 0.000000000000000000, -0.2419059403265113872 ) ) ;
#24106 = LINE ( 'NONE', #39852, #33674 ) ;
#24107 = ORIENTED_EDGE ( 'NONE', *, *, #40215, .F. ) ;
#24108 = CARTESIAN_POINT ( 'NONE',  ( 0.000000000000000000, 6.692913385826772199, 0.000000000000000000 ) ) ;
#24109 = CARTESIAN_POINT ( 'NONE',  ( -0.3486774197067340486, 3.346456692913386100, -0.8267716535433049518 ) ) ;
#24110 = ORIENTED_EDGE ( 'NONE', *, *, #4527, .T. ) ;
#24111 = FACE_OUTER_BOUND ( 'NONE', #17790, .T. ) ;
#24112 = CARTESIAN_POINT ( 'NONE',  ( 1.909347346926324462, 0.000000000000000000, -1.102362204724406602 ) ) ;
#24113 = EDGE_CURVE ( 'NONE', #35899, #39562, #48772, .T. ) ;
#24114 = CARTESIAN_POINT ( 'NONE',  ( 0.4696143004045476022, 0.000000000000000000, -2.244094488188969727 ) ) ;
#24115 = ORIENTED_EDGE ( 'NONE', *, *, #8624, .T. ) ;
#24116 = FACE_OUTER_BOUND ( 'NONE', #49235, .T. ) ;
#24117 = CARTESIAN_POINT ( 'NONE',  ( 0.5455278134075212115, 3.346456692913386100, -6.146657985744592735E-16 ) ) ;
#24118 = DIRECTION ( 'NONE',  ( -3.469446951953613696E-16, 0.000000000000000000, -1.000000000000000000 ) ) ;
#24119 = EDGE_CURVE ( 'NONE', #14632, #27097, #33850, .T. ) ;
#24120 = ORIENTED_EDGE ( 'NONE', *, *, #27176, .F. ) ;
#24121 = FACE_BOUND ( 'NONE', #19950, .T. ) ;
#24122 = LINE ( 'NONE', #32392, #18356 ) ;
#24123 = VERTEX_POINT ( 'NONE', #28933 ) ;
#24124 = PLANE ( 'NONE',  #31165 ) ;
#24125 = VECTOR ( 'NONE', #29162, 39.37007874015748143 ) ;
#24126 = CARTESIAN_POINT ( 'NONE',  ( -1.909347346926324462, 0.000000000000000000, -0.3543307086614171930 ) ) ;
#24127 = CARTESIAN_POINT ( 'NONE',  ( -0.3486774197067340486, 3.346456692913386100, -2.077238655036873549 ) ) ;
#24128 = CARTESIAN_POINT ( 'NONE',  ( -1.166969139818016199, 0.000000000000000000, -0.3543307086614174151 ) ) ;
#24129 = EDGE_CURVE ( 'NONE', #4890, #27417, #44670, .T. ) ;
#24130 = VECTOR ( 'NONE', #26740, 39.37007874015748143 ) ;
#24131 = ORIENTED_EDGE ( 'NONE', *, *, #7596, .T. ) ;
#24132 = ORIENTED_EDGE ( 'NONE', *, *, #12810, .T. ) ;
#24133 = DIRECTION ( 'NONE',  ( -1.000000000000000000, 0.000000000000000000, -0.000000000000000000 ) ) ;
#24134 = DIRECTION ( 'NONE',  ( -0.000000000000000000, -1.000000000000000000, -0.000000000000000000 ) ) ;
#24135 = ORIENTED_EDGE ( 'NONE', *, *, #14673, .F. ) ;
#24136 = VECTOR ( 'NONE', #45718, 39.37007874015748143 ) ;
#24137 = PLANE ( 'NONE',  #16850 ) ;
#24138 = LINE ( 'NONE', #28770, #27698 ) ;
#24139 = DIRECTION ( 'NONE',  ( -0.000000000000000000, 1.000000000000000000, -0.000000000000000000 ) ) ;
#24140 = EDGE_CURVE ( 'NONE', #39237, #16898, #5188, .T. ) ;
#24141 = AXIS2_PLACEMENT_3D ( 'NONE', #3909, #742, #5375 ) ;
#24142 = DIRECTION ( 'NONE',  ( 3.586865599282426309E-17, -1.000000000000000000, -1.103923720497134591E-16 ) ) ;
#24143 = VECTOR ( 'NONE', #48254, 39.37007874015748143 ) ;
#24144 = VERTEX_POINT ( 'NONE', #2345 ) ;
#24145 = ORIENTED_EDGE ( 'NONE', *, *, #2591, .T. ) ;
#24146 = LINE ( 'NONE', #21296, #35340 ) ;
#24147 = DIRECTION ( 'NONE',  ( -0.000000000000000000, 1.000000000000000000, -0.000000000000000000 ) ) ;
#24148 = CARTESIAN_POINT ( 'NONE',  ( -0.8942052331142552601, 0.000000000000000000, -2.086614173228339641 ) ) ;
#24149 = LINE ( 'NONE', #4528, #49547 ) ;
#24150 = FACE_BOUND ( 'NONE', #41336, .T. ) ;
#24151 = CIRCLE ( 'NONE', #15089, 2.165354330708661568 ) ;
#24152 = EDGE_LOOP ( 'NONE', ( #11197, #33801, #27971, #14577 ) ) ;
#24153 = ADVANCED_FACE ( 'NONE', ( #49025 ), #13455, .T. ) ;
#24154 = CARTESIAN_POINT ( 'NONE',  ( 1.940248144014060205, 1.742434946120271055, 1.610241538648720105 ) ) ;
#24155 = ORIENTED_EDGE ( 'NONE', *, *, #22376, .T. ) ;
#24156 = ORIENTED_EDGE ( 'NONE', *, *, #26926, .F. ) ;
#24157 = FACE_OUTER_BOUND ( 'NONE', #29091, .T. ) ;
#24158 = EDGE_CURVE ( 'NONE', #24016, #16727, #1829, .T. ) ;
#24159 = ORIENTED_EDGE ( 'NONE', *, *, #17903, .F. ) ;
#24160 = ORIENTED_EDGE ( 'NONE', *, *, #10915, .T. ) ;
#24161 = CARTESIAN_POINT ( 'NONE',  ( -4.268512490100411402E-16, 3.346456692913386100, -2.086614173228339641 ) ) ;
#24162 = UNCERTAINTY_MEASURE_WITH_UNIT (LENGTH_MEASURE( 1.000000000000000082E-05 ), #23563, 'distance_accuracy_value', 'NONE');
#24163 = VERTEX_POINT ( 'NONE', #5709 ) ;
#24164 = DIRECTION ( 'NONE',  ( 0.6910626489868580968, 0.000000000000000000, 0.7227948638273978821 ) ) ;
#24165 = CARTESIAN_POINT ( 'NONE',  ( -1.909347346926324462, 0.000000000000000000, -0.1574803149606297248 ) ) ;
#24166 = CARTESIAN_POINT ( 'NONE',  ( 2.339241080213585899, 1.462148010760873307, 1.802537235681917815 ) ) ;
#24167 = EDGE_CURVE ( 'NONE', #25499, #26189, #21968, .T. ) ;
#24168 =( BOUNDED_CURVE ( )  B_SPLINE_CURVE ( 3, ( #35732, #47567, #27979, #8371 ),
 .UNSPECIFIED., .F., .F. ) 
 B_SPLINE_CURVE_WITH_KNOTS ( ( 4, 4 ),
 ( 4.318880402357613946, 4.369812334041601964 ),
 .UNSPECIFIED. ) 
 CURVE ( )  GEOMETRIC_REPRESENTATION_ITEM ( )  RATIONAL_B_SPLINE_CURVE ( ( 1.000000000000000000, 0.9997838398768879031, 0.9997838398768879031, 1.000000000000000000 ) ) 
 REPRESENTATION_ITEM ( '' )  );
#24169 = DIRECTION ( 'NONE',  ( 0.5128992774059071280, 0.000000000000000000, -0.8584487936018655452 ) ) ;
#24170 = ADVANCED_FACE ( 'NONE', ( #17079 ), #45172, .F. ) ;
#24171 = EDGE_CURVE ( 'NONE', #28641, #16479, #48517, .T. ) ;
#24172 = VECTOR ( 'NONE', #14566, 39.37007874015748143 ) ;
#24173 = LINE ( 'NONE', #12037, #22037 ) ;
#24174 = CARTESIAN_POINT ( 'NONE',  ( -1.723188456408593527, 1.574803149606302854, 1.311251662046200694 ) ) ;
#24175 = ORIENTED_EDGE ( 'NONE', *, *, #39965, .T. ) ;
#24176 = DIRECTION ( 'NONE',  ( 1.734723475976806848E-16, 0.000000000000000000, 1.000000000000000000 ) ) ;
#24177 = CARTESIAN_POINT ( 'NONE',  ( -0.6214413264104945434, 3.267716535433071279, -2.244094488188968395 ) ) ;
#24178 = CARTESIAN_POINT ( 'NONE',  ( 1.833433833923350909, 3.346456692913386100, -1.456692913385823296 ) ) ;
#24179 = AXIS2_PLACEMENT_3D ( 'NONE', #2832, #9563, #33324 ) ;
#24180 = VECTOR ( 'NONE', #49213, 39.37007874015748143 ) ;
#24181 = ORIENTED_EDGE ( 'NONE', *, *, #23626, .T. ) ;
#24182 = FACE_OUTER_BOUND ( 'NONE', #46096, .T. ) ;
#24183 = DIRECTION ( 'NONE',  ( -0.8584487936018728726, -1.160734090543304907E-16, 0.5128992774058949156 ) ) ;
#24184 = VERTEX_POINT ( 'NONE', #18092 ) ;
#24185 = CARTESIAN_POINT ( 'NONE',  ( -0.7053729475263578186, 3.267716535433071279, -2.047244094488181343 ) ) ;
#24186 = CARTESIAN_POINT ( 'NONE',  ( 2.182111253630085290, 3.346456692913386100, -1.161035397307311917E-15 ) ) ;
#24187 = DIRECTION ( 'NONE',  ( 0.9998717552508121775, 0.01601477604151182663, 0.000000000000000000 ) ) ;
#24188 = AXIS2_PLACEMENT_3D ( 'NONE', #20811, #8171, #4811 ) ;
#24189 = DIRECTION ( 'NONE',  ( 1.734723475976806848E-16, -0.000000000000000000, 1.000000000000000000 ) ) ;
#24190 = ORIENTED_EDGE ( 'NONE', *, *, #8137, .T. ) ;
#24191 = LINE ( 'NONE', #4571, #41279 ) ;
#24192 = CARTESIAN_POINT ( 'NONE',  ( 0.1155636338427008941, -0.5222242541845523167, 0.000000000000000000 ) ) ;
#24193 = CARTESIAN_POINT ( 'NONE',  ( -0.07591351300297415061, 3.267716535433071279, 2.633779063002596873E-17 ) ) ;
#24194 = CARTESIAN_POINT ( 'NONE',  ( 1.531154912952772396, 1.205361022782829114E-17, 1.532020527533857646 ) ) ;
#24195 = EDGE_CURVE ( 'NONE', #31800, #16772, #40821, .T. ) ;
#24196 = ORIENTED_EDGE ( 'NONE', *, *, #12345, .T. ) ;
#24197 = ORIENTED_EDGE ( 'NONE', *, *, #1012, .T. ) ;
#24198 = LINE ( 'NONE', #43034, #48437 ) ;
#24199 = EDGE_LOOP ( 'NONE', ( #37413, #21918, #21742, #28035, #12726, #41771, #5788, #44231, #16275, #1121, #42162 ) ) ;
#24200 = DIRECTION ( 'NONE',  ( 0.000000000000000000, 0.000000000000000000, 1.000000000000000000 ) ) ;
#24201 = ORIENTED_EDGE ( 'NONE', *, *, #7473, .T. ) ;
#24202 = EDGE_CURVE ( 'NONE', #33287, #34811, #40089, .T. ) ;
#24203 = DIRECTION ( 'NONE',  ( 1.000000000000000000, 0.000000000000000000, 0.000000000000000000 ) ) ;
#24204 = ADVANCED_FACE ( 'NONE', ( #41585 ), #25576, .T. ) ;
#24205 = ORIENTED_EDGE ( 'NONE', *, *, #44063, .T. ) ;
#24206 = CARTESIAN_POINT ( 'NONE',  ( 1.636583440222563857, 3.346456692913386100, 0.6299212598425164567 ) ) ;
#24207 = EDGE_CURVE ( 'NONE', #40266, #29332, #46648, .T. ) ;
#24208 = VECTOR ( 'NONE', #5678, 39.37007874015748143 ) ;
#24209 = CARTESIAN_POINT ( 'NONE',  ( 1.636583440222563857, 0.000000000000000000, 0.9448818897637746295 ) ) ;
#24210 = ORIENTED_EDGE ( 'NONE', *, *, #4905, .T. ) ;
#24211 = B_SPLINE_CURVE_WITH_KNOTS ( 'NONE', 3,
 ( #31339, #36232, #4474, #43444 ),
 .UNSPECIFIED., .F., .F.,
 ( 4, 4 ),
 ( 0.0007442978046650536566, 0.04837702953537185296 ),
 .UNSPECIFIED. ) ;
#24212 = CARTESIAN_POINT ( 'NONE',  ( 0.2727639067037604392, 0.000000000000000000, -0.3543307086614173040 ) ) ;
#24213 = AXIS2_PLACEMENT_3D ( 'NONE', #13272, #33416, #34604 ) ;
#24214 = ORIENTED_EDGE ( 'NONE', *, *, #22132, .T. ) ;
#24215 = VECTOR ( 'NONE', #3245, 39.37007874015748143 ) ;
#24216 = VECTOR ( 'NONE', #22397, 39.37007874015748143 ) ;
#24217 = DIRECTION ( 'NONE',  ( 0.000000000000000000, 1.000000000000000000, 0.000000000000000000 ) ) ;
#24218 = ORIENTED_EDGE ( 'NONE', *, *, #41888, .T. ) ;
#24219 = ORIENTED_EDGE ( 'NONE', *, *, #25329, .T. ) ;
#24220 = EDGE_CURVE ( 'NONE', #36796, #18547, #17330, .T. ) ;
#24221 = FACE_OUTER_BOUND ( 'NONE', #46172, .T. ) ;
#24222 = AXIS2_PLACEMENT_3D ( 'NONE', #31602, #43199, #35476 ) ;
#24223 = DIRECTION ( 'NONE',  ( -1.206139481778036182E-16, 1.000000000000000000, -4.526717189434842013E-17 ) ) ;
#24224 = ORIENTED_EDGE ( 'NONE', *, *, #2481, .F. ) ;
#24225 = CARTESIAN_POINT ( 'NONE',  ( 1.780101451746606722, 1.205361022782829114E-17, 1.234002060668519585 ) ) ;
#24226 = ORIENTED_EDGE ( 'NONE', *, *, #17418, .F. ) ;
#24227 = CARTESIAN_POINT ( 'NONE',  ( 2.017116292511733633, 3.346456692913386100, 0.7874015748031456541 ) ) ;
#24228 = EDGE_CURVE ( 'NONE', #5661, #11518, #9579, .T. ) ;
#24229 = DIRECTION ( 'NONE',  ( -1.000000000000000000, 0.000000000000000000, 1.734723475976806848E-16 ) ) ;
#24231 = EDGE_CURVE ( 'NONE', #37886, #47515, #38727, .T. ) ;
#24230 = DIRECTION ( 'NONE',  ( -1.000000000000000000, 0.000000000000000000, -0.000000000000000000 ) ) ;
#24232 = ADVANCED_FACE ( 'NONE', ( #6977 ), #37975, .F. ) ;
#24233 = ORIENTED_EDGE ( 'NONE', *, *, #32860, .T. ) ;
#24234 = EDGE_LOOP ( 'NONE', ( #10079, #4147, #4280, #2623 ) ) ;
#24235 = DIRECTION ( 'NONE',  ( 0.000000000000000000, 0.000000000000000000, -1.000000000000000000 ) ) ;
#24236 = CARTESIAN_POINT ( 'NONE',  ( -2.168245791271168343, 1.587034731952809752, -2.004968704497279930 ) ) ;
#24237 = EDGE_CURVE ( 'NONE', #15224, #22568, #29963, .T. ) ;
#24238 = LINE ( 'NONE', #20355, #13459 ) ;
#24239 = CARTESIAN_POINT ( 'NONE',  ( 2.875073879017507217, 1.665576751341341089, -0.6730428845952017847 ) ) ;
#24240 = CARTESIAN_POINT ( 'NONE',  ( 1.909347346926324684, 0.000000000000000000, -0.03937007874015936021 ) ) ;
#24241 = CARTESIAN_POINT ( 'NONE',  ( -0.3486774197067332715, 3.267716535433071279, 1.209717811016576613E-16 ) ) ;
#24242 = ORIENTED_EDGE ( 'NONE', *, *, #5150, .F. ) ;
#24243 = LINE ( 'NONE', #9516, #26750 ) ;
#24244 = VECTOR ( 'NONE', #45648, 39.37007874015748143 ) ;
#24245 = ORIENTED_EDGE ( 'NONE', *, *, #25050, .F. ) ;
#24246 = DIRECTION ( 'NONE',  ( 0.000000000000000000, -1.000000000000000000, 0.000000000000000000 ) ) ;
#24247 = CIRCLE ( 'NONE', #12706, 2.164630168518208109 ) ;
#24248 = AXIS2_PLACEMENT_3D ( 'NONE', #17275, #47953, #28365 ) ;
#24249 = ORIENTED_EDGE ( 'NONE', *, *, #1016, .T. ) ;
#24250 = VECTOR ( 'NONE', #6022, 39.37007874015748143 ) ;
#24252 = CIRCLE ( 'NONE', #25911, 2.106299212598425008 ) ;
#24251 = FACE_OUTER_BOUND ( 'NONE', #2787, .T. ) ;
#24253 = CARTESIAN_POINT ( 'NONE',  ( -0.8182917201112819283, 3.346456692913386100, -0.7874015748031467643 ) ) ;
#24254 = PLANE ( 'NONE',  #34175 ) ;
#24255 = ORIENTED_EDGE ( 'NONE', *, *, #6212, .F. ) ;
#24256 = LINE ( 'NONE', #41033, #11748 ) ;
#24257 = VECTOR ( 'NONE', #17579, 39.37007874015748143 ) ;
#24258 = FACE_BOUND ( 'NONE', #21688, .T. ) ;
#24259 = ORIENTED_EDGE ( 'NONE', *, *, #5359, .T. ) ;
#24260 = CARTESIAN_POINT ( 'NONE',  ( 1.833433833923351353, 3.346456692913386100, -0.8267716535433055070 ) ) ;
#24261 = EDGE_LOOP ( 'NONE', ( #7146, #9838, #29843, #37739 ) ) ;
#24262 = CARTESIAN_POINT ( 'NONE',  ( -1.057143431661240696, 3.346456692913386100, 1.889763779527550147 ) ) ;
#24263 = DIRECTION ( 'NONE',  ( -3.469446951953613696E-16, 0.000000000000000000, -1.000000000000000000 ) ) ;
#24264 = EDGE_CURVE ( 'NONE', #37147, #6991, #38479, .T. ) ;
#24265 = EDGE_CURVE ( 'NONE', #27692, #5918, #34600, .T. ) ;
#24266 = CARTESIAN_POINT ( 'NONE',  ( 0.1067246931122726866, 0.02962905676920215767, 0.000000000000000000 ) ) ;
#24267 = ORIENTED_EDGE ( 'NONE', *, *, #35951, .T. ) ;
#24268 = ORIENTED_EDGE ( 'NONE', *, *, #48835, .F. ) ;
#24269 = LINE ( 'NONE', #15744, #7840 ) ;
#24270 = CARTESIAN_POINT ( 'NONE',  ( -0.5455278134075214336, 3.346456692913386100, -1.259842519685035134 ) ) ;
#24271 = CARTESIAN_POINT ( 'NONE',  ( -1.636583440222563635, 0.000000000000000000, 0.9448818897637749625 ) ) ;
#24272 = EDGE_CURVE ( 'NONE', #31774, #41036, #38167, .T. ) ;
#24273 = DIRECTION ( 'NONE',  ( -0.01601477604151182663, 0.9998717552508123996, -0.000000000000000000 ) ) ;
#24274 = CARTESIAN_POINT ( 'NONE',  ( 0.4696143004045479352, 0.000000000000000000, 0.7874015748031454320 ) ) ;
#24275 = ORIENTED_EDGE ( 'NONE', *, *, #42920, .T. ) ;
#24276 = DIRECTION ( 'NONE',  ( -8.881784197001252323E-16, 0.000000000000000000, 1.000000000000000000 ) ) ;
#24277 = AXIS2_PLACEMENT_3D ( 'NONE', #10137, #9117, #28982 ) ;
#24278 = ORIENTED_EDGE ( 'NONE', *, *, #11699, .T. ) ;
#24279 = ORIENTED_EDGE ( 'NONE', *, *, #29537, .T. ) ;
#24280 = EDGE_CURVE ( 'NONE', #26280, #22951, #6723, .T. ) ;
#24281 = B_SPLINE_CURVE_WITH_KNOTS ( 'NONE', 3,
 ( #11578, #38455, #42812, #38703 ),
 .UNSPECIFIED., .F., .F.,
 ( 4, 4 ),
 ( 0.05135061866764987354, 0.05233018460755119172 ),
 .UNSPECIFIED. ) ;
#24282 = VECTOR ( 'NONE', #23991, 39.37007874015748143 ) ;
#24283 = ORIENTED_EDGE ( 'NONE', *, *, #8055, .T. ) ;
#24284 = CARTESIAN_POINT ( 'NONE',  ( 2.755905511811024056, 4.960629921259846142, 1.023622047244094446 ) ) ;
#24285 = CIRCLE ( 'NONE', #30037, 2.164630168518208109 ) ;
#24286 = LINE ( 'NONE', #16542, #40658 ) ;
#24287 = EDGE_CURVE ( 'NONE', #41806, #24641, #22469, .T. ) ;
#24288 = DIRECTION ( 'NONE',  ( -0.5773502691896252870, -0.5773502691896267303, 0.5773502691896252870 ) ) ;
#24289 = CARTESIAN_POINT ( 'NONE',  ( -0.8942052331142552601, 3.346456692913386100, -1.574803149606293529 ) ) ;
#24290 = EDGE_CURVE ( 'NONE', #37439, #14063, #19090, .T. ) ;
#24291 = VERTEX_POINT ( 'NONE', #14976 ) ;
#24292 = VERTEX_POINT ( 'NONE', #15226 ) ;
#24293 = AXIS2_PLACEMENT_3D ( 'NONE', #34981, #3484, #15358 ) ;
#24294 = DIRECTION ( 'NONE',  ( 0.000000000000000000, 0.000000000000000000, 1.000000000000000000 ) ) ;
#24295 = DIRECTION ( 'NONE',  ( 0.9749279121818227312, 0.000000000000000000, 0.2225209339563184452 ) ) ;
#24296 = EDGE_CURVE ( 'NONE', #6941, #17122, #36876, .T. ) ;
#24297 = CARTESIAN_POINT ( 'NONE',  ( 1.833433833923351353, 0.000000000000000000, 0.3149606299212576177 ) ) ;
#24298 = ORIENTED_EDGE ( 'NONE', *, *, #26732, .F. ) ;
#24299 = CARTESIAN_POINT ( 'NONE',  ( -0.8429824507881226170, 1.205361022782829114E-17, -1.637047627937372241 ) ) ;
#24300 = DIRECTION ( 'NONE',  ( -1.000000000000000000, 0.000000000000000000, 1.734723475976806848E-16 ) ) ;
#24301 = DIRECTION ( 'NONE',  ( -0.000000000000000000, 0.000000000000000000, 1.000000000000000000 ) ) ;
#24302 = CARTESIAN_POINT ( 'NONE',  ( -1.905671854841497481, 5.905511811023623991, 2.256015092822653667 ) ) ;
#24303 = DIRECTION ( 'NONE',  ( 1.000000000000000000, 0.000000000000000000, 0.000000000000000000 ) ) ;
#24304 = ORIENTED_EDGE ( 'NONE', *, *, #3133, .F. ) ;
#24305 = DIRECTION ( 'NONE',  ( -0.000000000000000000, 0.000000000000000000, 1.000000000000000000 ) ) ;
#24306 = ORIENTED_EDGE ( 'NONE', *, *, #17306, .T. ) ;
#24307 = ORIENTED_EDGE ( 'NONE', *, *, #6413, .F. ) ;
#24308 = CARTESIAN_POINT ( 'NONE',  ( -0.4462886659516242527, 1.602328624241157851, 2.183640264916793861 ) ) ;
#24309 = CARTESIAN_POINT ( 'NONE',  ( 1.909347346926324684, 0.000000000000000000, -0.1574803149606304187 ) ) ;
#24310 = CARTESIAN_POINT ( 'NONE',  ( 1.709950266952970921, 0.000000000000000000, -0.3398067978735070382 ) ) ;
#24311 = EDGE_LOOP ( 'NONE', ( #12434, #39719, #6559, #6784 ) ) ;
#24312 = AXIS2_PLACEMENT_3D ( 'NONE', #31281, #3911, #35657 ) ;
#24313 = VERTEX_POINT ( 'NONE', #18341 ) ;
#24314 = VECTOR ( 'NONE', #50329, 39.37007874015748143 ) ;
#24315 = CARTESIAN_POINT ( 'NONE',  ( 1.833433833923351353, 3.267716535433071279, 0.9448818897637746295 ) ) ;
#24316 = ORIENTED_EDGE ( 'NONE', *, *, #17111, .F. ) ;
#24317 = DIRECTION ( 'NONE',  ( 0.000000000000000000, 0.000000000000000000, 1.000000000000000000 ) ) ;
#24318 = VECTOR ( 'NONE', #28758, 39.37007874015748143 ) ;
#24319 = VERTEX_POINT ( 'NONE', #7234 ) ;
#24320 = DIRECTION ( 'NONE',  ( 0.000000000000000000, 0.000000000000000000, 1.000000000000000000 ) ) ;
#24321 = CARTESIAN_POINT ( 'NONE',  ( 0.2727639067037602172, 0.000000000000000000, -1.929133858267710000 ) ) ;
#24322 = CARTESIAN_POINT ( 'NONE',  ( 1.833433833923351353, 3.346456692913386100, -1.259842519685035800 ) ) ;
#24323 = ORIENTED_EDGE ( 'NONE', *, *, #37346, .F. ) ;
#24324 = EDGE_CURVE ( 'NONE', #10381, #47342, #14210, .T. ) ;
#24325 = ORIENTED_EDGE ( 'NONE', *, *, #27689, .F. ) ;
#24326 = ORIENTED_EDGE ( 'NONE', *, *, #33271, .T. ) ;
#24327 = VECTOR ( 'NONE', #4069, 39.37007874015748143 ) ;
#24328 = CARTESIAN_POINT ( 'NONE',  ( 0.4696143004045478797, 0.000000000000000000, -1.614173228346451605 ) ) ;
#24329 = EDGE_CURVE ( 'NONE', #16368, #35037, #14723, .T. ) ;
#24330 = ORIENTED_EDGE ( 'NONE', *, *, #19155, .T. ) ;
#24331 = EDGE_LOOP ( 'NONE', ( #11953, #50382, #9420, #464 ) ) ;
#24332 = CARTESIAN_POINT ( 'NONE',  ( -2.182111253630085290, 0.000000000000000000, -6.146657985744592735E-16 ) ) ;
#24333 = FACE_OUTER_BOUND ( 'NONE', #23058, .T. ) ;
#24334 = CARTESIAN_POINT ( 'NONE',  ( 1.773598097765477277, 1.637884173412089250, 1.477342561509449759 ) ) ;
#24335 = EDGE_CURVE ( 'NONE', #41856, #29553, #28544, .T. ) ;
#24336 = ORIENTED_EDGE ( 'NONE', *, *, #43107, .F. ) ;
#24337 = CYLINDRICAL_SURFACE ( 'NONE', #32932, 2.164630168518208109 ) ;
#24338 = CARTESIAN_POINT ( 'NONE',  ( -0.3486774197067340486, 0.000000000000000000, 2.007874015748021268 ) ) ;
#24339 = DIRECTION ( 'NONE',  ( -1.000000000000000000, 0.000000000000000000, -0.000000000000000000 ) ) ;
#24340 = ORIENTED_EDGE ( 'NONE', *, *, #28978, .T. ) ;
#24341 = CARTESIAN_POINT ( 'NONE',  ( -1.088998432874329403, -2.184998798188223135E-16, 1.918626195649137278 ) ) ;
#24342 = CARTESIAN_POINT ( 'NONE',  ( -0.04921259842519706829, 1.707113721008201024, 2.241222193722145484 ) ) ;
#24343 = ORIENTED_EDGE ( 'NONE', *, *, #24843, .T. ) ;
#24344 = CARTESIAN_POINT ( 'NONE',  ( 4.268512490100411402E-16, 3.267716535433071279, 2.204724409448808764 ) ) ;
#24345 = ORIENTED_EDGE ( 'NONE', *, *, #43319, .T. ) ;
#24346 = ORIENTED_EDGE ( 'NONE', *, *, #24991, .T. ) ;
#24347 = DIRECTION ( 'NONE',  ( 1.000000000000000000, 0.000000000000000000, -3.469446951953613696E-16 ) ) ;
#24348 = CARTESIAN_POINT ( 'NONE',  ( 0.000000000000000000, 5.905511811023623991, 0.000000000000000000 ) ) ;
#24349 = EDGE_CURVE ( 'NONE', #45498, #34106, #49788, .T. ) ;
#24350 = DIRECTION ( 'NONE',  ( -3.469446951953613696E-16, 0.000000000000000000, -1.000000000000000000 ) ) ;
#24351 = LINE ( 'NONE', #8858, #20558 ) ;
#24352 = ORIENTED_EDGE ( 'NONE', *, *, #12283, .F. ) ;
#24353 = ORIENTED_EDGE ( 'NONE', *, *, #28499, .F. ) ;
#24354 = AXIS2_PLACEMENT_3D ( 'NONE', #26610, #7501, #27111 ) ;
#24355 = EDGE_CURVE ( 'NONE', #5323, #47624, #10845, .T. ) ;
#24356 = DIRECTION ( 'NONE',  ( -0.000000000000000000, 0.000000000000000000, 1.000000000000000000 ) ) ;
#24357 = EDGE_LOOP ( 'NONE', ( #4262, #4407, #18946, #15541 ) ) ;
#24358 = CARTESIAN_POINT ( 'NONE',  ( 0.000000000000000000, 1.574803149606302854, 0.000000000000000000 ) ) ;
#24359 = CARTESIAN_POINT ( 'NONE',  ( -2.437180031585919782, 5.905511811023623991, -1.667735833703135162 ) ) ;
#24360 = AXIS2_PLACEMENT_3D ( 'NONE', #15795, #40334, #32331 ) ;
#24361 = B_SPLINE_CURVE_WITH_KNOTS ( 'NONE', 3,
 ( #11347, #3854, #46925, #50773 ),
 .UNSPECIFIED., .F., .F.,
 ( 4, 4 ),
 ( 2.008334170439436058E-07, 0.002500502013016788969 ),
 .UNSPECIFIED. ) ;
#24362 = PLANE ( 'NONE',  #49706 ) ;
#24363 = CARTESIAN_POINT ( 'NONE',  ( 0.000000000000000000, 2.755905511811023612, -2.066929133858268042 ) ) ;
#24364 = CARTESIAN_POINT ( 'NONE',  ( 0.8182917201112819283, 3.267716535433071279, 0.4724409448818868706 ) ) ;
#24365 = CIRCLE ( 'NONE', #35054, 2.165354330708661568 ) ;
#24366 = ORIENTED_EDGE ( 'NONE', *, *, #43620, .T. ) ;
#24367 = FACE_OUTER_BOUND ( 'NONE', #50883, .T. ) ;
#24368 = EDGE_CURVE ( 'NONE', #17591, #4242, #40997, .T. ) ;
#24369 = FACE_OUTER_BOUND ( 'NONE', #48843, .T. ) ;
#24370 = ORIENTED_EDGE ( 'NONE', *, *, #25550, .F. ) ;
#24371 = PLANE ( 'NONE',  #33152 ) ;
#24372 = CARTESIAN_POINT ( 'NONE',  ( -0.8013547812368906342, 1.706765689785105788, -2.841982942531803502 ) ) ;
#24373 = LINE ( 'NONE', #20231, #22203 ) ;
#24374 = VERTEX_POINT ( 'NONE', #21878 ) ;
#24375 = CARTESIAN_POINT ( 'NONE',  ( -1.091055626815042645, 3.267716535433071279, 2.007874015748021268 ) ) ;
#24376 = CARTESIAN_POINT ( 'NONE',  ( 1.062992125984251635, 0.000000000000000000, 1.181102362204724088 ) ) ;
#24377 = LINE ( 'NONE', #15853, #50566 ) ;
#24378 = ORIENTED_EDGE ( 'NONE', *, *, #26336, .T. ) ;
#24379 = CARTESIAN_POINT ( 'NONE',  ( -1.439733046521776583, 3.346456692913386100, -1.574803149606293307 ) ) ;
#24380 = FACE_OUTER_BOUND ( 'NONE', #41241, .T. ) ;
#24381 = ORIENTED_EDGE ( 'NONE', *, *, #14574, .T. ) ;
#24382 = LINE ( 'NONE', #40137, #15495 ) ;
#24383 = FACE_OUTER_BOUND ( 'NONE', #4072, .T. ) ;
#24384 = DIRECTION ( 'NONE',  ( -0.000000000000000000, 1.000000000000000000, -0.000000000000000000 ) ) ;
#24385 = CARTESIAN_POINT ( 'NONE',  ( -0.8987785766980536106, 1.205361022782829114E-17, 1.600251783270283390 ) ) ;
#24386 = ORIENTED_EDGE ( 'NONE', *, *, #13321, .F. ) ;
#24387 = ORIENTED_EDGE ( 'NONE', *, *, #30848, .T. ) ;
#24388 = CARTESIAN_POINT ( 'NONE',  ( 0.7423782071083085965, 3.267716535433071279, -0.8267716535433055070 ) ) ;
#24389 = VECTOR ( 'NONE', #36313, 39.37007874015748143 ) ;
#24390 = CARTESIAN_POINT ( 'NONE',  ( -2.932023289724621673, 1.575122962489508449, 0.3475074887687388259 ) ) ;
#24391 = EDGE_CURVE ( 'NONE', #36871, #4582, #40737, .T. ) ;
#24392 = VECTOR ( 'NONE', #50663, 39.37007874015748143 ) ;
#24393 = VERTEX_POINT ( 'NONE', #29363 ) ;
#24394 = DIRECTION ( 'NONE',  ( -0.000000000000000000, 1.000000000000000000, -0.000000000000000000 ) ) ;
#24395 = DIRECTION ( 'NONE',  ( -1.000000000000000000, 0.000000000000000000, -0.000000000000000000 ) ) ;
#24396 = DIRECTION ( 'NONE',  ( 0.000000000000000000, -1.000000000000000000, 0.000000000000000000 ) ) ;
#24397 = AXIS2_PLACEMENT_3D ( 'NONE', #47451, #8512, #16519 ) ;
#24398 = EDGE_CURVE ( 'NONE', #13922, #22651, #18252, .T. ) ;
#24399 = LINE ( 'NONE', #28005, #3349 ) ;
#24400 = VERTEX_POINT ( 'NONE', #34013 ) ;
#24401 = ORIENTED_EDGE ( 'NONE', *, *, #24171, .F. ) ;
#24402 = EDGE_CURVE ( 'NONE', #9083, #44588, #10254, .T. ) ;
#24403 = DIRECTION ( 'NONE',  ( -0.000000000000000000, -1.000000000000000000, -0.000000000000000000 ) ) ;
#24404 = CARTESIAN_POINT ( 'NONE',  ( -1.712496953225537633, 0.000000000000000000, 1.220472440944875059 ) ) ;
#24405 = VECTOR ( 'NONE', #17868, 39.37007874015748143 ) ;
#24406 = CARTESIAN_POINT ( 'NONE',  ( -2.182111253630085290, 3.267716535433071279, 0.7480314960629874665 ) ) ;
#24407 = ADVANCED_FACE ( 'NONE', ( #33252 ), #18001, .F. ) ;
#24408 = DIRECTION ( 'NONE',  ( -1.000000000000000000, 0.000000000000000000, 0.000000000000000000 ) ) ;
#24409 = FACE_BOUND ( 'NONE', #44573, .T. ) ;
#24410 = VERTEX_POINT ( 'NONE', #2515 ) ;
#24411 = CARTESIAN_POINT ( 'NONE',  ( 1.560669927219590303, 3.346456692913386100, -1.732283464566923170 ) ) ;
#24412 = ORIENTED_EDGE ( 'NONE', *, *, #45810, .F. ) ;
#24413 = VERTEX_POINT ( 'NONE', #5362 ) ;
#24414 = DIRECTION ( 'NONE',  ( -3.986037398843765983E-20, -1.000000000000000000, -1.160734090543304660E-16 ) ) ;
#24415 = EDGE_CURVE ( 'NONE', #37842, #26630, #26086, .T. ) ;
#24416 = VERTEX_POINT ( 'NONE', #49447 ) ;
#24417 = ORIENTED_EDGE ( 'NONE', *, *, #35349, .T. ) ;
#24418 = CARTESIAN_POINT ( 'NONE',  ( 1.287906020515830141, 3.346456692913386100, 1.062992125984246083 ) ) ;
#24419 = ORIENTED_EDGE ( 'NONE', *, *, #38179, .T. ) ;
#24420 = EDGE_CURVE ( 'NONE', #29695, #17626, #3822, .T. ) ;
#24421 = PLANE ( 'NONE',  #2361 ) ;
#24422 = CARTESIAN_POINT ( 'NONE',  ( 0.5455278134075211005, 0.000000000000000000, -0.1968503937007880511 ) ) ;
#24423 = CARTESIAN_POINT ( 'NONE',  ( 1.636583440222563857, 3.267716535433071279, 0.3149606299212576177 ) ) ;
#24424 = B_SPLINE_CURVE_WITH_KNOTS ( 'NONE', 3,
 ( #34337, #19069, #34582, #38952 ),
 .UNSPECIFIED., .F., .F.,
 ( 4, 4 ),
 ( 2.766470520694630865E-07, 0.002500519372013545929 ),
 .UNSPECIFIED. ) ;
#24425 = B_SPLINE_CURVE_WITH_KNOTS ( 'NONE', 3,
 ( #38344, #42198, #39272, #19639 ),
 .UNSPECIFIED., .F., .F.,
 ( 4, 4 ),
 ( 2.330000271410587266E-07, 0.002500456604366177622 ),
 .UNSPECIFIED. ) ;
#24426 = EDGE_CURVE ( 'NONE', #4117, #27908, #22135, .T. ) ;
#24427 = AXIS2_PLACEMENT_3D ( 'NONE', #18145, #4681, #23520 ) ;
#24428 = DIRECTION ( 'NONE',  ( -1.000000000000000000, 0.000000000000000000, -0.000000000000000000 ) ) ;
#24429 = DIRECTION ( 'NONE',  ( -0.01601477604151182663, 0.9998717552508123996, -0.000000000000000000 ) ) ;
#24430 = DIRECTION ( 'NONE',  ( 0.000000000000000000, -1.000000000000000000, 0.000000000000000000 ) ) ;
#24431 = VECTOR ( 'NONE', #14468, 39.37007874015748143 ) ;
#24432 = ORIENTED_EDGE ( 'NONE', *, *, #41077, .F. ) ;
#24433 = CARTESIAN_POINT ( 'NONE',  ( 0.000000000000000000, 3.267716535433071279, 0.000000000000000000 ) ) ;
#24434 = AXIS2_PLACEMENT_3D ( 'NONE', #23649, #19767, #35530 ) ;
#24435 = CARTESIAN_POINT ( 'NONE',  ( -1.909347346926324906, 3.267716535433071279, -0.7874015748031470974 ) ) ;
#24436 = EDGE_CURVE ( 'NONE', #34370, #36292, #29876, .T. ) ;
#24437 = DIRECTION ( 'NONE',  ( -3.469446951953613696E-16, 0.000000000000000000, -1.000000000000000000 ) ) ;
#24438 = VERTEX_POINT ( 'NONE', #49698 ) ;
#24439 = DIRECTION ( 'NONE',  ( 1.000000000000000000, -0.000000000000000000, 0.000000000000000000 ) ) ;
#24440 = DIRECTION ( 'NONE',  ( 1.734723475976806848E-16, 0.000000000000000000, 1.000000000000000000 ) ) ;
#24441 = ORIENTED_EDGE ( 'NONE', *, *, #22909, .F. ) ;
#24442 = DIRECTION ( 'NONE',  ( 0.000000000000000000, 0.000000000000000000, 1.000000000000000000 ) ) ;
#24443 = VECTOR ( 'NONE', #26033, 39.37007874015748143 ) ;
#24444 = CARTESIAN_POINT ( 'NONE',  ( 1.215401739843891216, 1.661752038239891593, 1.938290036035023034 ) ) ;
#24445 = CARTESIAN_POINT ( 'NONE',  ( 0.000000000000000000, 3.267716535433071279, -0.5118110236220465570 ) ) ;
#24446 = VECTOR ( 'NONE', #34746, 39.37007874015748143 ) ;
#24447 = EDGE_CURVE ( 'NONE', #11420, #40469, #26002, .T. ) ;
#24448 = ORIENTED_EDGE ( 'NONE', *, *, #35626, .T. ) ;
#24449 = DIRECTION ( 'NONE',  ( -0.000000000000000000, -1.000000000000000000, -0.000000000000000000 ) ) ;
#24450 = ORIENTED_EDGE ( 'NONE', *, *, #3198, .T. ) ;
#24451 = DIRECTION ( 'NONE',  ( -0.01601477604151182663, 0.9998717552508123996, -0.000000000000000000 ) ) ;
#24452 = DIRECTION ( 'NONE',  ( 0.01601477604151182663, -0.9998717552508123996, 0.000000000000000000 ) ) ;
#24453 = B_SPLINE_CURVE_WITH_KNOTS ( 'NONE', 3,
 ( #24078, #47785, #3953, #35699 ),
 .UNSPECIFIED., .F., .F.,
 ( 4, 4 ),
 ( 0.1211873102087489551, 0.1625992483279400380 ),
 .UNSPECIFIED. ) ;
#24454 = CARTESIAN_POINT ( 'NONE',  ( -1.091055626815042645, 0.000000000000000000, -7.512581982576723358E-16 ) ) ;
#24455 = LINE ( 'NONE', #953, #1227 ) ;
#24456 = VERTEX_POINT ( 'NONE', #9750 ) ;
#24457 = VERTEX_POINT ( 'NONE', #14382 ) ;
#24458 = DIRECTION ( 'NONE',  ( 1.734723475976806848E-16, -0.000000000000000000, 1.000000000000000000 ) ) ;
#24459 = ORIENTED_EDGE ( 'NONE', *, *, #41088, .T. ) ;
#24460 = CARTESIAN_POINT ( 'NONE',  ( -2.074049943651441019, 6.692913385826772199, 0.6221544894623932676 ) ) ;
#24461 = ORIENTED_EDGE ( 'NONE', *, *, #20476, .F. ) ;
#24462 = EDGE_CURVE ( 'NONE', #16283, #25223, #45047, .T. ) ;
#24463 = CARTESIAN_POINT ( 'NONE',  ( -0.07591351300297340121, 3.346456692913386100, -1.614173228346451605 ) ) ;
#24464 = ORIENTED_EDGE ( 'NONE', *, *, #40019, .T. ) ;
#24465 = PLANE ( 'NONE',  #49630 ) ;
#24466 = VECTOR ( 'NONE', #1196, 39.37007874015748143 ) ;
#24467 = EDGE_CURVE ( 'NONE', #28095, #41852, #37892, .T. ) ;
#24468 = CARTESIAN_POINT ( 'NONE',  ( -1.363819533518803473, 0.000000000000000000, -0.7874015748031470974 ) ) ;
#24469 = AXIS2_PLACEMENT_3D ( 'NONE', #15714, #19576, #11087 ) ;
#24470 = ORIENTED_EDGE ( 'NONE', *, *, #7393, .T. ) ;
#24471 = AXIS2_PLACEMENT_3D ( 'NONE', #24358, #31597, #27708 ) ;
#24472 = CARTESIAN_POINT ( 'NONE',  ( -1.057143431661237143, 3.346456692913386100, -1.889763779527552146 ) ) ;
#24473 = ORIENTED_EDGE ( 'NONE', *, *, #21321, .T. ) ;
#24474 = CARTESIAN_POINT ( 'NONE',  ( 1.560669927219590303, 3.186757942779276043, -1.929133858267710666 ) ) ;
#24475 = AXIS2_PLACEMENT_3D ( 'NONE', #50571, #10127, #2636 ) ;
#24476 = EDGE_LOOP ( 'NONE', ( #44691, #4621, #25117, #25969 ) ) ;
#24477 = VERTEX_POINT ( 'NONE', #37124 ) ;
#24478 = FACE_OUTER_BOUND ( 'NONE', #36658, .T. ) ;
#24479 = VECTOR ( 'NONE', #23818, 39.37007874015748143 ) ;
#24480 = ORIENTED_EDGE ( 'NONE', *, *, #43477, .F. ) ;
#24481 = PLANE ( 'NONE',  #50106 ) ;
#24482 = EDGE_LOOP ( 'NONE', ( #20133, #30623, #36714, #6978 ) ) ;
#24483 = CARTESIAN_POINT ( 'NONE',  ( 0.04921259842519669359, 1.610264983814881479, 2.246280244424690320 ) ) ;
#24484 = CARTESIAN_POINT ( 'NONE',  ( 0.000000000000000000, 3.267716535433071279, 0.2755905511810994302 ) ) ;
#24485 = EDGE_CURVE ( 'NONE', #41751, #30226, #45342, .T. ) ;
#24486 = DIRECTION ( 'NONE',  ( -0.9998717552508122886, -0.01601477604151181275, 0.000000000000000000 ) ) ;
#24487 = ORIENTED_EDGE ( 'NONE', *, *, #44790, .T. ) ;
#24488 = B_SPLINE_CURVE_WITH_KNOTS ( 'NONE', 3,
 ( #29394, #20882, #33543, #40513 ),
 .UNSPECIFIED., .F., .F.,
 ( 4, 4 ),
 ( 2.655981437406432628E-07, 0.002500437702427189216 ),
 .UNSPECIFIED. ) ;
#24489 = CARTESIAN_POINT ( 'NONE',  ( -1.477903774005060233, 1.618613820676564341, 1.616798831468284625 ) ) ;
#24490 = LINE ( 'NONE', #8996, #2257 ) ;
#24491 = LINE ( 'NONE', #32503, #9291 ) ;
#24492 = CARTESIAN_POINT ( 'NONE',  ( -1.062992125984250968, 0.000000000000000000, 1.181102362204724088 ) ) ;
#24493 = CARTESIAN_POINT ( 'NONE',  ( 1.091055626815042423, 0.000000000000000000, -1.889763779527552368 ) ) ;
#24494 = EDGE_CURVE ( 'NONE', #43929, #11186, #17245, .T. ) ;
#24495 = CARTESIAN_POINT ( 'NONE',  ( -2.932023289724621673, 1.575122962489508449, 0.3475074887687388259 ) ) ;
#24496 = ADVANCED_FACE ( 'NONE', ( #1739 ), #27727, .F. ) ;
#24497 = LINE ( 'NONE', #20872, #12796 ) ;
#24498 = ORIENTED_EDGE ( 'NONE', *, *, #47676, .T. ) ;
#24499 = EDGE_CURVE ( 'NONE', #48342, #26667, #10989, .T. ) ;
#24500 = DIRECTION ( 'NONE',  ( -3.469446951953613696E-16, 0.000000000000000000, -1.000000000000000000 ) ) ;
#24501 = ORIENTED_EDGE ( 'NONE', *, *, #4840, .T. ) ;
#24502 = AXIS2_PLACEMENT_3D ( 'NONE', #37847, #41448, #33206 ) ;
#24503 = LINE ( 'NONE', #5647, #27559 ) ;
#24504 = EDGE_CURVE ( 'NONE', #34423, #4372, #25710, .T. ) ;
#24505 = ORIENTED_EDGE ( 'NONE', *, *, #31235, .T. ) ;
#24506 = EDGE_CURVE ( 'NONE', #49034, #39073, #49199, .T. ) ;
#24507 = CARTESIAN_POINT ( 'NONE',  ( -1.439733046521777027, 3.267716535433071279, -0.8267716535433052849 ) ) ;
#24508 = FACE_OUTER_BOUND ( 'NONE', #35170, .T. ) ;
#24509 = DIRECTION ( 'NONE',  ( -0.000000000000000000, -1.000000000000000000, -0.000000000000000000 ) ) ;
#24510 = CARTESIAN_POINT ( 'NONE',  ( -1.971247363764854876, 5.905511811023623991, -0.8960709840011923388 ) ) ;
#24511 = VERTEX_POINT ( 'NONE', #30387 ) ;
#24512 = CARTESIAN_POINT ( 'NONE',  ( 1.560669927219591191, 0.000000000000000000, 1.535433070866133898 ) ) ;
#24513 = CARTESIAN_POINT ( 'NONE',  ( -2.104388748321702529, 0.5252928353968839836, -0.4298348072943085629 ) ) ;
#24514 = EDGE_LOOP ( 'NONE', ( #40086, #445, #42790, #44939 ) ) ;
#24515 = FACE_OUTER_BOUND ( 'NONE', #34122, .T. ) ;
#24516 = VECTOR ( 'NONE', #35599, 39.37007874015748143 ) ;
#24517 = ORIENTED_EDGE ( 'NONE', *, *, #47048, .F. ) ;
#24518 = EDGE_CURVE ( 'NONE', #29198, #10488, #15138, .T. ) ;
#24519 = CARTESIAN_POINT ( 'NONE',  ( -1.536664496436148184E-16, 0.000000000000000000, -0.5118110236220465570 ) ) ;
#24520 = CARTESIAN_POINT ( 'NONE',  ( 0.000000000000000000, 3.267716535433071279, -2.086614173228339641 ) ) ;
#24521 = EDGE_CURVE ( 'NONE', #23541, #30890, #49951, .T. ) ;
#24522 = LINE ( 'NONE', #1022, #18120 ) ;
#24523 = ORIENTED_EDGE ( 'NONE', *, *, #29468, .F. ) ;
#24524 = ORIENTED_EDGE ( 'NONE', *, *, #24231, .F. ) ;
#24525 = DIRECTION ( 'NONE',  ( 0.000000000000000000, 0.000000000000000000, -1.000000000000000000 ) ) ;
#24526 = CARTESIAN_POINT ( 'NONE',  ( -0.7874015748031495399, 0.000000000000000000, -1.220472440944881942 ) ) ;
#24527 = FACE_BOUND ( 'NONE', #23692, .T. ) ;
#24528 = LINE ( 'NONE', #11876, #45152 ) ;
#24529 = DIRECTION ( 'NONE',  ( -0.4738686624730094055, -1.021948367985145802E-16, 0.8805955318567321166 ) ) ;
#24530 = VECTOR ( 'NONE', #20712, 39.37007874015748143 ) ;
#24531 = VECTOR ( 'NONE', #37728, 39.37007874015748143 ) ;
#24532 = VERTEX_POINT ( 'NONE', #38141 ) ;
#24533 = DIRECTION ( 'NONE',  ( 0.000000000000000000, 0.000000000000000000, -1.000000000000000000 ) ) ;
#24534 = ORIENTED_EDGE ( 'NONE', *, *, #14625, .F. ) ;
#24535 = VERTEX_POINT ( 'NONE', #42245 ) ;
#24536 = ORIENTED_EDGE ( 'NONE', *, *, #37744, .F. ) ;
#24537 = CARTESIAN_POINT ( 'NONE',  ( 2.002746723317192057, 1.743427769888226786, 1.534191940547938060 ) ) ;
#24538 = DIRECTION ( 'NONE',  ( 0.000000000000000000, -0.000000000000000000, -1.000000000000000000 ) ) ;
#24539 = CARTESIAN_POINT ( 'NONE',  ( 0.000000000000000000, 0.000000000000000000, 0.000000000000000000 ) ) ;
#24540 = FACE_OUTER_BOUND ( 'NONE', #36196, .T. ) ;
#24541 = ORIENTED_EDGE ( 'NONE', *, *, #3358, .F. ) ;
#24542 = EDGE_LOOP ( 'NONE', ( #48450, #42117, #12049, #49929 ) ) ;
#24543 = CARTESIAN_POINT ( 'NONE',  ( -1.030301126714985971, 0.000000000000000000, -1.501813316714599500 ) ) ;
#24544 = FACE_OUTER_BOUND ( 'NONE', #26967, .T. ) ;
#24545 = DIRECTION ( 'NONE',  ( 0.5877852522924685852, 0.000000000000000000, 0.8090169943749507819 ) ) ;
#24546 = VECTOR ( 'NONE', #50158, 39.37007874015748143 ) ;
#24547 = CARTESIAN_POINT ( 'NONE',  ( 0.8182917201112819283, 0.000000000000000000, 0.1574803149606286423 ) ) ;
#24548 = DIRECTION ( 'NONE',  ( 1.734723475976806848E-16, 0.000000000000000000, 1.000000000000000000 ) ) ;
#24549 = EDGE_CURVE ( 'NONE', #25449, #7908, #7147, .T. ) ;
#24550 = CARTESIAN_POINT ( 'NONE',  ( 1.091055626815042645, 3.346456692913386100, -0.5118110236220471121 ) ) ;
#24551 = EDGE_CURVE ( 'NONE', #7984, #18957, #15395, .T. ) ;
#24552 = B_SPLINE_CURVE_WITH_KNOTS ( 'NONE', 3,
 ( #38550, #2925, #38797, #18673 ),
 .UNSPECIFIED., .F., .F.,
 ( 4, 4 ),
 ( 0.01248276987548075333, 0.03073907100476382798 ),
 .UNSPECIFIED. ) ;
#24553 = CARTESIAN_POINT ( 'NONE',  ( 1.091055626815042645, 0.000000000000000000, -0.3149606299212596716 ) ) ;
#24554 = EDGE_CURVE ( 'NONE', #34698, #26534, #3775, .T. ) ;
#24555 = DIRECTION ( 'NONE',  ( 0.5773502691896268413, -0.5773502691896258421, 0.5773502691896243988 ) ) ;
#24556 = VERTEX_POINT ( 'NONE', #14640 ) ;
#24557 = PLANE ( 'NONE',  #45639 ) ;
#24558 = ORIENTED_EDGE ( 'NONE', *, *, #10913, .T. ) ;
#24559 = ORIENTED_EDGE ( 'NONE', *, *, #43600, .F. ) ;
#24560 = DIRECTION ( 'NONE',  ( 1.000000000000000000, 0.000000000000000000, 0.000000000000000000 ) ) ;
#24561 = LINE ( 'NONE', #43401, #8866 ) ;
#24562 = CARTESIAN_POINT ( 'NONE',  ( 1.879299076413774250, 0.5249316475426859530, -0.1336616210247123793 ) ) ;
#24563 = AXIS2_PLACEMENT_3D ( 'NONE', #12769, #40896, #8634 ) ;
#24564 = ORIENTED_EDGE ( 'NONE', *, *, #21707, .T. ) ;
#24565 = VECTOR ( 'NONE', #50229, 39.37007874015748143 ) ;
#24566 = ORIENTED_EDGE ( 'NONE', *, *, #27329, .T. ) ;
#24567 = DIRECTION ( 'NONE',  ( -1.000000000000000000, 0.000000000000000000, 0.000000000000000000 ) ) ;
#24568 = VECTOR ( 'NONE', #38941, 39.37007874015748143 ) ;
#24570 = ORIENTED_EDGE ( 'NONE', *, *, #45117, .F. ) ;
#24569 = ADVANCED_FACE ( 'NONE', ( #39140 ), #30895, .T. ) ;
#24571 = CARTESIAN_POINT ( 'NONE',  ( -0.8182917201112814842, 3.346456692913386100, 1.417322834645662777 ) ) ;
#24572 = ORIENTED_EDGE ( 'NONE', *, *, #12812, .F. ) ;
#24573 = VECTOR ( 'NONE', #15994, 39.37007874015748143 ) ;
#24574 = CARTESIAN_POINT ( 'NONE',  ( -1.794796351285541602, 3.346456692913386100, -1.102362204724405492 ) ) ;
#24575 = EDGE_CURVE ( 'NONE', #24669, #47335, #50202, .T. ) ;
#24576 = PLANE ( 'NONE',  #37127 ) ;
#24577 = CARTESIAN_POINT ( 'NONE',  ( 0.000000000000000000, 3.267716535433071279, 2.007874015748021268 ) ) ;
#24578 = ADVANCED_FACE ( 'NONE', ( #6884 ), #50955, .F. ) ;
#24579 = VECTOR ( 'NONE', #37951, 39.37007874015748143 ) ;
#24580 = ORIENTED_EDGE ( 'NONE', *, *, #17903, .T. ) ;
#24581 = ORIENTED_EDGE ( 'NONE', *, *, #3123, .T. ) ;
#24582 = ORIENTED_EDGE ( 'NONE', *, *, #13224, .T. ) ;
#24583 = DIRECTION ( 'NONE',  ( -3.469446951953613696E-16, 0.000000000000000000, -1.000000000000000000 ) ) ;
#24584 = EDGE_CURVE ( 'NONE', #337, #30787, #18514, .T. ) ;
#24586 = ORIENTED_EDGE ( 'NONE', *, *, #43404, .F. ) ;
#24585 = EDGE_CURVE ( 'NONE', #5165, #47515, #3017, .T. ) ;
#24587 = VERTEX_POINT ( 'NONE', #11520 ) ;
#24588 = DIRECTION ( 'NONE',  ( -0.000000000000000000, 1.000000000000000000, -0.000000000000000000 ) ) ;
#24589 = LINE ( 'NONE', #319, #2991 ) ;
#24590 = CARTESIAN_POINT ( 'NONE',  ( -0.8182917201112819283, 3.346456692913386100, 2.004783788421104163 ) ) ;
#24591 = VECTOR ( 'NONE', #39531, 39.37007874015748143 ) ;
#24592 = EDGE_LOOP ( 'NONE', ( #23090, #25230, #2886, #1963 ) ) ;
#24593 = CARTESIAN_POINT ( 'NONE',  ( -1.712496953225537411, 3.267716535433071279, 5.941417334598190051E-16 ) ) ;
#24594 = LINE ( 'NONE', #12206, #21708 ) ;
#24595 = CARTESIAN_POINT ( 'NONE',  ( -1.439733046521776361, 3.267716535433071279, 4.995077429881866871E-16 ) ) ;
#24596 = VERTEX_POINT ( 'NONE', #26500 ) ;
#24597 = CARTESIAN_POINT ( 'NONE',  ( 2.182111253630085290, 3.346456692913386100, 0.3149606299212573401 ) ) ;
#24598 = CARTESIAN_POINT ( 'NONE',  ( -0.7582255214199161708, 0.000000000000000000, -1.687894986714875811 ) ) ;
#24599 = VERTEX_POINT ( 'NONE', #18764 ) ;
#24600 = LINE ( 'NONE', #4975, #30627 ) ;
#24601 = ORIENTED_EDGE ( 'NONE', *, *, #4347, .T. ) ;
#24602 = ORIENTED_EDGE ( 'NONE', *, *, #12623, .F. ) ;
#24603 = FACE_OUTER_BOUND ( 'NONE', #31635, .T. ) ;
#24604 = LINE ( 'NONE', #32357, #6150 ) ;
#24605 = DIRECTION ( 'NONE',  ( 1.000000000000000000, 0.000000000000000000, -3.469446951953613696E-16 ) ) ;
#24606 = AXIS2_PLACEMENT_3D ( 'NONE', #35939, #568, #16315 ) ;
#24607 = CARTESIAN_POINT ( 'NONE',  ( 1.062992125984251413, 0.4724409448818890911, -1.181102362204724754 ) ) ;
#24608 = CARTESIAN_POINT ( 'NONE',  ( 1.062992125984251413, 0.5905511811023621549, -1.181102362204724754 ) ) ;
#24609 = ORIENTED_EDGE ( 'NONE', *, *, #15467, .T. ) ;
#24610 = ORIENTED_EDGE ( 'NONE', *, *, #39443, .F. ) ;
#24611 = LINE ( 'NONE', #37005, #32515 ) ;
#24612 = AXIS2_PLACEMENT_3D ( 'NONE', #42184, #26438, #22570 ) ;
#24613 = EDGE_LOOP ( 'NONE', ( #41664, #34475, #11476, #13605 ) ) ;
#24614 = FACE_OUTER_BOUND ( 'NONE', #10810, .T. ) ;
#24615 = CARTESIAN_POINT ( 'NONE',  ( 0.5284761224300885685, 1.574803149606302854, -2.099874368989729234 ) ) ;
#24616 = VECTOR ( 'NONE', #19546, 39.37007874015748143 ) ;
#24617 = VECTOR ( 'NONE', #30388, 39.37007874015748143 ) ;
#24618 = CARTESIAN_POINT ( 'NONE',  ( 2.535292374475893951, 1.653425583089147111, -0.06459790964117027856 ) ) ;
#24619 = EDGE_CURVE ( 'NONE', #47691, #22113, #50446, .T. ) ;
#24620 = CARTESIAN_POINT ( 'NONE',  ( 0.000000000000000000, 3.267716535433071279, -1.102362204724405492 ) ) ;
#24621 = CARTESIAN_POINT ( 'NONE',  ( 1.556712866041120247, 5.905511811023623991, 2.509548638715870084 ) ) ;
#24622 = ORIENTED_EDGE ( 'NONE', *, *, #14913, .T. ) ;
#24623 = ADVANCED_FACE ( 'NONE', ( #34519 ), #3265, .F. ) ;
#24624 = DIRECTION ( 'NONE',  ( 0.000000000000000000, -1.000000000000000000, -1.156482317317871478E-16 ) ) ;
#24625 = VECTOR ( 'NONE', #37597, 39.37007874015748143 ) ;
#24626 = CARTESIAN_POINT ( 'NONE',  ( 1.472219874544873131, 1.482402307789154161, 2.560030851058970214 ) ) ;
#24627 = EDGE_CURVE ( 'NONE', #34259, #8195, #22889, .T. ) ;
#24628 = VERTEX_POINT ( 'NONE', #11270 ) ;
#24629 = CARTESIAN_POINT ( 'NONE',  ( -1.636583440222564301, 0.000000000000000000, -1.259842519685034468 ) ) ;
#24630 = VECTOR ( 'NONE', #30136, 39.37007874015748143 ) ;
#24631 = CARTESIAN_POINT ( 'NONE',  ( -1.439733046521777027, 3.267716535433071279, -1.141732283464563791 ) ) ;
#24632 = LINE ( 'NONE', #44738, #50186 ) ;
#24633 = VERTEX_POINT ( 'NONE', #23136 ) ;
#24634 = PLANE ( 'NONE',  #35830 ) ;
#24635 = CARTESIAN_POINT ( 'NONE',  ( -1.355031041518317325, 0.004193974497218569755, 1.143546472689453530 ) ) ;
#24636 = CARTESIAN_POINT ( 'NONE',  ( 2.308203157375244152E-16, 0.07874015748031502893, -1.682967650661292502 ) ) ;
#24637 = ORIENTED_EDGE ( 'NONE', *, *, #46121, .F. ) ;
#24638 = CARTESIAN_POINT ( 'NONE',  ( 0.2727639067037609943, 3.346456692913386100, 0.9055118110236167750 ) ) ;
#24640 = LINE ( 'NONE', #36516, #34863 ) ;
#24639 = B_SPLINE_CURVE_WITH_KNOTS ( 'NONE', 3,
 ( #6897, #31406, #34526, #27517 ),
 .UNSPECIFIED., .F., .F.,
 ( 4, 4 ),
 ( 0.1211775127643062860, 0.1625894504277921315 ),
 .UNSPECIFIED. ) ;
#24641 = VERTEX_POINT ( 'NONE', #38888 ) ;
#24642 = FACE_OUTER_BOUND ( 'NONE', #7580, .T. ) ;
#24643 = LINE ( 'NONE', #20511, #32590 ) ;
#24644 = EDGE_CURVE ( 'NONE', #23774, #12300, #35020, .T. ) ;
#24645 = DIRECTION ( 'NONE',  ( -0.000000000000000000, 1.000000000000000000, -0.000000000000000000 ) ) ;
#24646 = CARTESIAN_POINT ( 'NONE',  ( -1.062992125984250968, 0.5905511811023621549, 1.181102362204724088 ) ) ;
#24647 = AXIS2_PLACEMENT_3D ( 'NONE', #9923, #13797, #48098 ) ;
#24648 = VERTEX_POINT ( 'NONE', #46851 ) ;
#24649 = ORIENTED_EDGE ( 'NONE', *, *, #26104, .F. ) ;
#24650 = CARTESIAN_POINT ( 'NONE',  ( 1.363819533518803029, 3.346456692913386100, -1.929133858267710666 ) ) ;
#24651 = CARTESIAN_POINT ( 'NONE',  ( 0.000000000000000000, 3.346456692913386100, 0.000000000000000000 ) ) ;
#24652 = EDGE_CURVE ( 'NONE', #4557, #33393, #22710, .T. ) ;
#24653 = VERTEX_POINT ( 'NONE', #31469 ) ;
#24654 = CARTESIAN_POINT ( 'NONE',  ( 2.951990591674675368, 0.000000000000000000, -0.08331184815398383348 ) ) ;
#24655 = PLANE ( 'NONE',  #40051 ) ;
#24656 = CARTESIAN_POINT ( 'NONE',  ( 1.015142113812069091, 0.000000000000000000, -1.732283464566923614 ) ) ;
#24657 = CARTESIAN_POINT ( 'NONE',  ( -1.712067434724807269, 0.0003367829894146713294, -0.3402900276016438963 ) ) ;
#24658 = VECTOR ( 'NONE', #20456, 39.37007874015748143 ) ;
#24659 = AXIS2_PLACEMENT_3D ( 'NONE', #45536, #25431, #30074 ) ;
#24660 = VERTEX_POINT ( 'NONE', #27074 ) ;
#24661 = VERTEX_POINT ( 'NONE', #26824 ) ;
#24662 = DIRECTION ( 'NONE',  ( -3.469446951953613696E-16, 0.000000000000000000, -1.000000000000000000 ) ) ;
#24663 = DIRECTION ( 'NONE',  ( 1.000000000000000000, -0.000000000000000000, 0.000000000000000000 ) ) ;
#24664 = LINE ( 'NONE', #40419, #8235 ) ;
#24665 = ORIENTED_EDGE ( 'NONE', *, *, #36834, .F. ) ;
#24666 = AXIS2_PLACEMENT_3D ( 'NONE', #6712, #2333, #22711 ) ;
#24667 = DIRECTION ( 'NONE',  ( -1.729310098865080642E-17, 1.000000000000000000, 1.276627980444840260E-16 ) ) ;
#24668 = FACE_BOUND ( 'NONE', #3621, .T. ) ;
#24669 = VERTEX_POINT ( 'NONE', #39210 ) ;
#24670 = CARTESIAN_POINT ( 'NONE',  ( 0.1828395243478885546, 1.016784016014155245, -2.580520392578918187 ) ) ;
#24671 = EDGE_LOOP ( 'NONE', ( #20584, #32087, #11551 ) ) ;
#24672 = ORIENTED_EDGE ( 'NONE', *, *, #41077, .T. ) ;
#24673 = VECTOR ( 'NONE', #13521, 39.37007874015748143 ) ;
#24674 = CARTESIAN_POINT ( 'NONE',  ( -0.8182917201112819283, 3.346456692913386100, -1.929133858267710000 ) ) ;
#24675 = EDGE_LOOP ( 'NONE', ( #46896, #32300, #24432, #6650 ) ) ;
#24676 = VERTEX_POINT ( 'NONE', #42576 ) ;
#24677 = DIRECTION ( 'NONE',  ( -3.469446951953613696E-16, 0.000000000000000000, -1.000000000000000000 ) ) ;
#24678 = UNCERTAINTY_MEASURE_WITH_UNIT (LENGTH_MEASURE( 1.000000000000000082E-05 ), #5490, 'distance_accuracy_value', 'NONE');
#24679 = ORIENTED_EDGE ( 'NONE', *, *, #12405, .T. ) ;
#24680 = FACE_OUTER_BOUND ( 'NONE', #26816, .T. ) ;
#24681 = DIRECTION ( 'NONE',  ( 0.9797780297642104674, 0.000000000000000000, 0.2000875118326022606 ) ) ;
#24682 = CARTESIAN_POINT ( 'NONE',  ( -2.949782676795219771, 0.000000000000000000, -0.1324748927672794452 ) ) ;
#24683 = VECTOR ( 'NONE', #28439, 39.37007874015748143 ) ;
#24684 = FACE_OUTER_BOUND ( 'NONE', #40429, .T. ) ;
#24685 = B_SPLINE_CURVE_WITH_KNOTS ( 'NONE', 3,
 ( #18058, #14174, #38445, #29678 ),
 .UNSPECIFIED., .F., .F.,
 ( 4, 4 ),
 ( 0.0009431515978678377396, 0.003443434775124777723 ),
 .UNSPECIFIED. ) ;
#24686 = EDGE_CURVE ( 'NONE', #41228, #36899, #33513, .T. ) ;
#24687 = DIRECTION ( 'NONE',  ( -0.000000000000000000, 1.000000000000000000, -0.000000000000000000 ) ) ;
#24688 = DIRECTION ( 'NONE',  ( -3.469446951953613696E-16, 0.000000000000000000, -1.000000000000000000 ) ) ;
#24689 = ORIENTED_EDGE ( 'NONE', *, *, #35570, .F. ) ;
#24690 = EDGE_CURVE ( 'NONE', #14887, #30087, #32743, .T. ) ;
#24691 = DIRECTION ( 'NONE',  ( -1.000000000000000000, 0.000000000000000000, 1.734723475976806848E-16 ) ) ;
#24692 = DIRECTION ( 'NONE',  ( 1.734723475976806848E-16, -0.000000000000000000, 1.000000000000000000 ) ) ;
#24693 = EDGE_CURVE ( 'NONE', #22293, #15466, #33773, .T. ) ;
#24694 = PRODUCT_DEFINITION ( 'UNKNOWN', '', #6959, #6117 ) ;
#24695 = VECTOR ( 'NONE', #31784, 39.37007874015748143 ) ;
#24696 = VERTEX_POINT ( 'NONE', #15468 ) ;
#24697 = PLANE ( 'NONE',  #11640 ) ;
#24698 = CARTESIAN_POINT ( 'NONE',  ( 1.015142113812069091, 3.267716535433071279, -1.845530509571139399 ) ) ;
#24699 = ORIENTED_EDGE ( 'NONE', *, *, #34991, .F. ) ;
#24700 = CARTESIAN_POINT ( 'NONE',  ( -1.181102362204724310, 0.5905511811023621549, -1.062992125984252079 ) ) ;
#24701 = EDGE_CURVE ( 'NONE', #40553, #33305, #14964, .T. ) ;
#24702 = CARTESIAN_POINT ( 'NONE',  ( 2.738124037479889417, 1.758476085681704326, -0.1722314944998213082 ) ) ;
#24703 = VECTOR ( 'NONE', #8378, 39.37007874015748143 ) ;
#24704 = CARTESIAN_POINT ( 'NONE',  ( 0.000000000000000000, 2.755905511811023612, -2.066929133858268042 ) ) ;
#24705 = ORIENTED_EDGE ( 'NONE', *, *, #2436, .F. ) ;
#24706 = DIRECTION ( 'NONE',  ( 1.000000000000000000, -0.000000000000000000, 0.000000000000000000 ) ) ;
#24707 = AXIS2_PLACEMENT_3D ( 'NONE', #8383, #47323, #3299 ) ;
#24708 = ORIENTED_EDGE ( 'NONE', *, *, #44934, .T. ) ;
#24709 = FACE_BOUND ( 'NONE', #5725, .T. ) ;
#24710 = LINE ( 'NONE', #33228, #26746 ) ;
#24711 = CARTESIAN_POINT ( 'NONE',  ( -1.062992125984250968, 0.4724409448818890911, 1.181102362204724088 ) ) ;
#24712 = EDGE_CURVE ( 'NONE', #12127, #3016, #19828, .T. ) ;
#24713 = CARTESIAN_POINT ( 'NONE',  ( 1.833433833923351353, 3.267716535433071279, -0.8267716535433055070 ) ) ;
#24714 = EDGE_LOOP ( 'NONE', ( #30202, #48304, #7892, #19104 ) ) ;
#24715 = VERTEX_POINT ( 'NONE', #3849 ) ;
#24716 = DIRECTION ( 'NONE',  ( 1.000000000000000000, 0.000000000000000000, 0.000000000000000000 ) ) ;
#24717 = VERTEX_POINT ( 'NONE', #30712 ) ;
#24718 = ADVANCED_FACE ( 'NONE', ( #50518 ), #27324, .F. ) ;
#24719 = FACE_OUTER_BOUND ( 'NONE', #47906, .T. ) ;
#24720 = EDGE_LOOP ( 'NONE', ( #29342, #46221, #39857, #28198 ) ) ;
#24721 = FACE_OUTER_BOUND ( 'NONE', #25015, .T. ) ;
#24722 = AXIS2_PLACEMENT_3D ( 'NONE', #41801, #6687, #33814 ) ;
#24723 = ORIENTED_EDGE ( 'NONE', *, *, #19147, .T. ) ;
#24724 = DIRECTION ( 'NONE',  ( 1.000000000000000000, 0.000000000000000000, 0.000000000000000000 ) ) ;
#24725 = LINE ( 'NONE', #5860, #8313 ) ;
#24726 = ORIENTED_EDGE ( 'NONE', *, *, #46607, .F. ) ;
#24727 = PRODUCT_DEFINITION_CONTEXT ( 'detailed design', #18712, 'design' ) ;
#24728 = DIRECTION ( 'NONE',  ( -0.000000000000000000, 1.000000000000000000, -0.000000000000000000 ) ) ;
#24729 = ORIENTED_EDGE ( 'NONE', *, *, #38457, .F. ) ;
#24730 = ADVANCED_FACE ( 'NONE', ( #27579 ), #23715, .F. ) ;
#24731 = VECTOR ( 'NONE', #40807, 39.37007874015748143 ) ;
#24732 = ORIENTED_EDGE ( 'NONE', *, *, #18900, .F. ) ;
#24733 = ORIENTED_EDGE ( 'NONE', *, *, #19139, .F. ) ;
#24734 = CARTESIAN_POINT ( 'NONE',  ( -1.428275480578807599, 1.594612651218729749, 2.294580664572506645 ) ) ;
#24735 = ORIENTED_EDGE ( 'NONE', *, *, #45061, .F. ) ;
#24736 = VECTOR ( 'NONE', #38309, 39.37007874015748143 ) ;
#24737 = LINE ( 'NONE', #32756, #41099 ) ;
#24738 = ORIENTED_EDGE ( 'NONE', *, *, #36865, .T. ) ;
#24739 = CARTESIAN_POINT ( 'NONE',  ( 1.091055626815042423, 3.267716535433071279, -1.771653543307081691 ) ) ;
#24740 = FACE_OUTER_BOUND ( 'NONE', #15995, .T. ) ;
#24741 = DIRECTION ( 'NONE',  ( -3.469446951953613696E-16, 0.000000000000000000, -1.000000000000000000 ) ) ;
#24742 = VERTEX_POINT ( 'NONE', #22962 ) ;
#24743 = LINE ( 'NONE', #44347, #2212 ) ;
#24744 = LINE ( 'NONE', #28861, #13911 ) ;
#24745 = LINE ( 'NONE', #43127, #5157 ) ;
#24746 = DIRECTION ( 'NONE',  ( 1.734723475976806848E-16, -0.000000000000000000, 1.000000000000000000 ) ) ;
#24747 = CARTESIAN_POINT ( 'NONE',  ( -0.07591351300297284610, 0.000000000000000000, 0.9055118110236167750 ) ) ;
#24748 = DIRECTION ( 'NONE',  ( -3.469446951953613696E-16, 0.000000000000000000, -1.000000000000000000 ) ) ;
#24749 = EDGE_CURVE ( 'NONE', #24066, #45331, #7465, .T. ) ;
#24750 = DIRECTION ( 'NONE',  ( -1.000000000000000000, 0.000000000000000000, 0.000000000000000000 ) ) ;
#24751 = EDGE_CURVE ( 'NONE', #38194, #36441, #11837, .T. ) ;
#24752 = VERTEX_POINT ( 'NONE', #3089 ) ;
#24753 = CARTESIAN_POINT ( 'NONE',  ( 0.4696143004045476577, 3.267716535433071279, -2.047244094488182231 ) ) ;
#24754 = EDGE_CURVE ( 'NONE', #33477, #10560, #35598, .T. ) ;
#24755 = CARTESIAN_POINT ( 'NONE',  ( 2.061875708210571201, 1.740926663775191674, 1.053657044629532802 ) ) ;
#24756 = ORIENTED_EDGE ( 'NONE', *, *, #17354, .T. ) ;
#24757 = DIRECTION ( 'NONE',  ( -0.6234898018587318180, 9.077469801274542449E-17, -0.7818314824680309139 ) ) ;
#24758 = B_SPLINE_CURVE_WITH_KNOTS ( 'NONE', 3,
 ( #10458, #38091, #10712, #42450 ),
 .UNSPECIFIED., .F., .F.,
 ( 4, 4 ),
 ( 2.558210376252241617E-07, 0.002500373932690979316 ),
 .UNSPECIFIED. ) ;
#24759 = ORIENTED_EDGE ( 'NONE', *, *, #26447, .F. ) ;
#24760 = DIRECTION ( 'NONE',  ( 1.000000000000000000, 0.000000000000000000, 0.000000000000000000 ) ) ;
#24761 = LINE ( 'NONE', #28623, #14337 ) ;
#24762 = VECTOR ( 'NONE', #10583, 39.37007874015748143 ) ;
#24763 = CARTESIAN_POINT ( 'NONE',  ( -1.166969139818015755, 3.346456692913386100, 0.2755905511810996522 ) ) ;
#24764 = VECTOR ( 'NONE', #17247, 39.37007874015748143 ) ;
#24765 = DIRECTION ( 'NONE',  ( 1.734723475976806848E-16, -0.000000000000000000, 1.000000000000000000 ) ) ;
#24766 = DIRECTION ( 'NONE',  ( 1.000000000000000000, 0.000000000000000000, -3.469446951953613696E-16 ) ) ;
#24767 = ORIENTED_EDGE ( 'NONE', *, *, #43048, .T. ) ;
#24768 = CARTESIAN_POINT ( 'NONE',  ( 0.000000000000000000, 3.346456692913386100, 0.000000000000000000 ) ) ;
#24769 = CYLINDRICAL_SURFACE ( 'NONE', #34466, 2.165354330708661568 ) ;
#24770 = VERTEX_POINT ( 'NONE', #50768 ) ;
#24771 = DIRECTION ( 'NONE',  ( 1.000000000000000000, 0.000000000000000000, -3.469446951953613696E-16 ) ) ;
#24772 = AXIS2_PLACEMENT_3D ( 'NONE', #12643, #45133, #5146 ) ;
#24773 = ORIENTED_EDGE ( 'NONE', *, *, #21156, .F. ) ;
#24774 = LINE ( 'NONE', #24519, #22735 ) ;
#24775 = CARTESIAN_POINT ( 'NONE',  ( 2.164658444855302122, 5.905511811023623991, -0.04795272066889885720 ) ) ;
#24776 = EDGE_CURVE ( 'NONE', #8443, #42166, #15966, .T. ) ;
#24777 = B_SPLINE_CURVE_WITH_KNOTS ( 'NONE', 3,
 ( #42129, #6002, #15021, #21758 ),
 .UNSPECIFIED., .F., .F.,
 ( 4, 4 ),
 ( 2.074911753762320913E-07, 0.01858314050568160916 ),
 .UNSPECIFIED. ) ;
#24778 = CARTESIAN_POINT ( 'NONE',  ( -2.150611651783668865, 1.640647882934381574, -0.2522489660909295051 ) ) ;
#24779 = ORIENTED_EDGE ( 'NONE', *, *, #40092, .T. ) ;
#24780 = VERTEX_POINT ( 'NONE', #217 ) ;
#24781 = CARTESIAN_POINT ( 'NONE',  ( 1.091055626815042645, 3.267716535433071279, 1.062992125984246083 ) ) ;
#24782 = DIRECTION ( 'NONE',  ( -1.000000000000000000, 0.000000000000000000, -0.000000000000000000 ) ) ;
#24783 = CARTESIAN_POINT ( 'NONE',  ( 3.937007874015748143, 5.118110236220475784, 1.181102362204724310 ) ) ;
#24784 = EDGE_CURVE ( 'NONE', #22488, #25289, #7970, .T. ) ;
#24785 = FACE_OUTER_BOUND ( 'NONE', #34869, .T. ) ;
#24786 = CARTESIAN_POINT ( 'NONE',  ( 0.000000000000000000, 3.267716535433071279, -1.614173228346451605 ) ) ;
#24787 = ORIENTED_EDGE ( 'NONE', *, *, #31750, .T. ) ;
#24788 = DIRECTION ( 'NONE',  ( 0.000000000000000000, 1.000000000000000000, 0.000000000000000000 ) ) ;
#24789 = ADVANCED_FACE ( 'NONE', ( #7714 ), #15211, .F. ) ;
#24790 = ORIENTED_EDGE ( 'NONE', *, *, #49081, .F. ) ;
#24791 = ORIENTED_EDGE ( 'NONE', *, *, #42108, .T. ) ;
#24793 = EDGE_CURVE ( 'NONE', #43930, #35527, #11340, .T. ) ;
#24792 = VERTEX_POINT ( 'NONE', #10832 ) ;
#24794 = CARTESIAN_POINT ( 'NONE',  ( 2.390031926231672710, 1.654552468068580806, 1.342016610150888134 ) ) ;
#24795 = VECTOR ( 'NONE', #7779, 39.37007874015748143 ) ;
#24796 = CARTESIAN_POINT ( 'NONE',  ( 0.2212097921902143327, 0.01045795994330635768, -1.908835200420839984 ) ) ;
#24797 = VECTOR ( 'NONE', #11298, 39.37007874015748143 ) ;
#24798 = FACE_OUTER_BOUND ( 'NONE', #43847, .T. ) ;
#24799 = DIRECTION ( 'NONE',  ( 1.000000000000000000, 0.000000000000000000, -3.469446951953613696E-16 ) ) ;
#24800 = ORIENTED_EDGE ( 'NONE', *, *, #33174, .F. ) ;
#24801 = ORIENTED_EDGE ( 'NONE', *, *, #34331, .F. ) ;
#24802 = CYLINDRICAL_SURFACE ( 'NONE', #3505, 2.165354330708661568 ) ;
#24803 = CARTESIAN_POINT ( 'NONE',  ( 0.4696143004045479352, 0.000000000000000000, -0.1574803149606298636 ) ) ;
#24804 = LINE ( 'NONE', #1307, #4348 ) ;
#24805 = VECTOR ( 'NONE', #7938, 39.37007874015748143 ) ;
#24806 = B_SPLINE_CURVE_WITH_KNOTS ( 'NONE', 3,
 ( #40125, #8116, #20751, #23862 ),
 .UNSPECIFIED., .F., .F.,
 ( 4, 4 ),
 ( 0.001651792006055582919, 0.004151899744057469845 ),
 .UNSPECIFIED. ) ;
#24807 = CARTESIAN_POINT ( 'NONE',  ( 1.636583440222563857, 0.000000000000000000, 1.574803149606291974 ) ) ;
#24808 = LINE ( 'NONE', #47489, #3342 ) ;
#24809 = EDGE_CURVE ( 'NONE', #24660, #16416, #30644, .T. ) ;
#24810 = FACE_OUTER_BOUND ( 'NONE', #30130, .T. ) ;
#24811 = EDGE_CURVE ( 'NONE', #27417, #34340, #740, .T. ) ;
#24812 = EDGE_CURVE ( 'NONE', #30339, #13697, #27836, .T. ) ;
#24813 = DIRECTION ( 'NONE',  ( -0.000000000000000000, 1.000000000000000000, -0.000000000000000000 ) ) ;
#24814 = ORIENTED_EDGE ( 'NONE', *, *, #30774, .F. ) ;
#24815 = EDGE_CURVE ( 'NONE', #4171, #24715, #44093, .T. ) ;
#24816 = CARTESIAN_POINT ( 'NONE',  ( 1.015142113812069313, 3.346456692913386100, 0.9055118110236164419 ) ) ;
#24817 = CARTESIAN_POINT ( 'NONE',  ( 0.002207914879453961535, -5.712274067634378313E-18, 0.04916304461325374242 ) ) ;
#24818 = ORIENTED_EDGE ( 'NONE', *, *, #50439, .T. ) ;
#24819 = ORIENTED_EDGE ( 'NONE', *, *, #13449, .F. ) ;
#24820 = CARTESIAN_POINT ( 'NONE',  ( 2.684779361005118048, 1.757638757588847911, -0.5623051772365603718 ) ) ;
#24821 = DIRECTION ( 'NONE',  ( 1.000000000000000000, 0.000000000000000000, 0.000000000000000000 ) ) ;
#24822 = ORIENTED_EDGE ( 'NONE', *, *, #26760, .T. ) ;
#24823 = EDGE_LOOP ( 'NONE', ( #31970, #8523, #22202, #41422 ) ) ;
#24824 = CARTESIAN_POINT ( 'NONE',  ( 1.833433833923351353, 0.000000000000000000, -0.5118110236220471121 ) ) ;
#24825 = VERTEX_POINT ( 'NONE', #5117 ) ;
#24826 = B_SPLINE_CURVE_WITH_KNOTS ( 'NONE', 3,
 ( #51012, #205, #15956, #43819 ),
 .UNSPECIFIED., .F., .F.,
 ( 4, 4 ),
 ( 0.1211873102087489551, 0.1625992483279400380 ),
 .UNSPECIFIED. ) ;
#24827 = ORIENTED_EDGE ( 'NONE', *, *, #38094, .F. ) ;
#24828 = VECTOR ( 'NONE', #42825, 39.37007874015748143 ) ;
#24829 = CARTESIAN_POINT ( 'NONE',  ( 0.5756566573088583993, 1.502670515430445386, 2.896516654582643291 ) ) ;
#24830 = LINE ( 'NONE', #17595, #11533 ) ;
#24831 = CIRCLE ( 'NONE', #46248, 2.106299212598425008 ) ;
#24832 = EDGE_CURVE ( 'NONE', #7771, #32210, #24743, .T. ) ;
#24833 = ORIENTED_EDGE ( 'NONE', *, *, #29860, .T. ) ;
#24834 = DIMENSIONAL_EXPONENTS ( 1.000000000000000000, 0.000000000000000000, 0.000000000000000000, 0.000000000000000000, 0.000000000000000000, 0.000000000000000000, 0.000000000000000000 ) ;
#24835 = ORIENTED_EDGE ( 'NONE', *, *, #16986, .F. ) ;
#24836 = ORIENTED_EDGE ( 'NONE', *, *, #9550, .T. ) ;
#24837 = DIRECTION ( 'NONE',  ( 0.000000000000000000, 1.000000000000000000, 0.000000000000000000 ) ) ;
#24838 = ORIENTED_EDGE ( 'NONE', *, *, #3391, .F. ) ;
#24839 = ORIENTED_EDGE ( 'NONE', *, *, #30041, .T. ) ;
#24840 = CARTESIAN_POINT ( 'NONE',  ( -0.9225641150147850800, 1.049866565067838264, -1.802300656478875052 ) ) ;
#24841 = CARTESIAN_POINT ( 'NONE',  ( 0.4350747367505088947, 1.205361022782829114E-17, -2.121846421795415161 ) ) ;
#24842 = LINE ( 'NONE', #8837, #32719 ) ;
#24843 = EDGE_CURVE ( 'NONE', #1626, #26463, #23645, .T. ) ;
#24844 = AXIS2_PLACEMENT_3D ( 'NONE', #21073, #29060, #36828 ) ;
#24845 = VERTEX_POINT ( 'NONE', #20865 ) ;
#24846 = EDGE_CURVE ( 'NONE', #29348, #18296, #9717, .T. ) ;
#24847 = DIRECTION ( 'NONE',  ( 0.4348526007323283427, 0.000000000000000000, 0.9005016466594218949 ) ) ;
#24848 = DIRECTION ( 'NONE',  ( -0.000000000000000000, 1.000000000000000000, -0.000000000000000000 ) ) ;
#24849 = CARTESIAN_POINT ( 'NONE',  ( 0.8182917201112819283, 3.346456692913386100, -0.6692913385826764205 ) ) ;
#24850 = EDGE_CURVE ( 'NONE', #15713, #4024, #36878, .T. ) ;
#24851 = VERTEX_POINT ( 'NONE', #40747 ) ;
#24852 = FACE_OUTER_BOUND ( 'NONE', #25442, .T. ) ;
#24853 = LINE ( 'NONE', #36733, #6270 ) ;
#24854 = LINE ( 'NONE', #20716, #15869 ) ;
#24855 = ORIENTED_EDGE ( 'NONE', *, *, #34924, .T. ) ;
#24856 = VERTEX_POINT ( 'NONE', #1499 ) ;
#24857 = DIRECTION ( 'NONE',  ( -3.986037398843765983E-20, -1.000000000000000000, -1.160734090543304660E-16 ) ) ;
#24858 = CARTESIAN_POINT ( 'NONE',  ( -1.195183497228115035E-16, 3.346456692913386100, -1.574803149606293529 ) ) ;
#24859 = CARTESIAN_POINT ( 'NONE',  ( -1.979793062125317471, 1.556934451446513545, 2.191257344206539504 ) ) ;
#24860 = EDGE_CURVE ( 'NONE', #4326, #28186, #39722, .T. ) ;
#24861 = DIRECTION ( 'NONE',  ( -1.000000000000000000, 0.000000000000000000, 1.734723475976806848E-16 ) ) ;
#24862 = VERTEX_POINT ( 'NONE', #4356 ) ;
#24863 = VERTEX_POINT ( 'NONE', #4867 ) ;
#24864 = DIRECTION ( 'NONE',  ( 1.347303628949392478E-32, -1.160734090543304660E-16, 1.000000000000000000 ) ) ;
#24865 = EDGE_CURVE ( 'NONE', #33261, #17939, #27768, .T. ) ;
#24866 = VERTEX_POINT ( 'NONE', #31724 ) ;
#24867 = LINE ( 'NONE', #33644, #26598 ) ;
#24868 = DIRECTION ( 'NONE',  ( -1.000000000000000000, 0.000000000000000000, 0.000000000000000000 ) ) ;
#24869 = VECTOR ( 'NONE', #27523, 39.37007874015748143 ) ;
#24870 = ADVANCED_FACE ( 'NONE', ( #36109 ), #16489, .F. ) ;
#24871 = EDGE_CURVE ( 'NONE', #30098, #42285, #32240, .T. ) ;
#24872 = B_SPLINE_CURVE_WITH_KNOTS ( 'NONE', 3,
 ( #13666, #36913, #16778, #48474 ),
 .UNSPECIFIED., .F., .F.,
 ( 4, 4 ),
 ( 2.396516866961895415E-07, 0.002500331606968418403 ),
 .UNSPECIFIED. ) ;
#24873 = CARTESIAN_POINT ( 'NONE',  ( 2.743641484424565569, 1.660104339391717643, -0.07395487895817318136 ) ) ;
#24874 = DIRECTION ( 'NONE',  ( 1.000000000000000000, 0.000000000000000000, 0.000000000000000000 ) ) ;
#24876 = DIRECTION ( 'NONE',  ( 0.6579387259397138088, 0.000000000000000000, -0.7530714660036099684 ) ) ;
#24875 = VECTOR ( 'NONE', #7622, 39.37007874015748143 ) ;
#24877 = ORIENTED_EDGE ( 'NONE', *, *, #369, .T. ) ;
#24878 = LINE ( 'NONE', #40627, #10187 ) ;
#24879 = EDGE_CURVE ( 'NONE', #37287, #43799, #42969, .T. ) ;
#24880 = AXIS2_PLACEMENT_3D ( 'NONE', #50008, #14434, #6943 ) ;
#24881 = CARTESIAN_POINT ( 'NONE',  ( -0.6214413264104945434, 0.000000000000000000, -1.614173228346451605 ) ) ;
#24882 = ORIENTED_EDGE ( 'NONE', *, *, #25629, .F. ) ;
#24883 = VECTOR ( 'NONE', #42392, 39.37007874015748143 ) ;
#24884 = DIRECTION ( 'NONE',  ( -1.000000000000000000, 0.000000000000000000, 1.734723475976806848E-16 ) ) ;
#24885 = FACE_OUTER_BOUND ( 'NONE', #28806, .T. ) ;
#24886 = DIRECTION ( 'NONE',  ( -1.000000000000000000, -0.000000000000000000, -0.000000000000000000 ) ) ;
#24887 = EDGE_LOOP ( 'NONE', ( #23888, #5993, #24249, #47036 ) ) ;
#24888 = DIRECTION ( 'NONE',  ( -3.469446951953613696E-16, 0.000000000000000000, -1.000000000000000000 ) ) ;
#24889 = DIRECTION ( 'NONE',  ( -3.469446951953613696E-16, 0.000000000000000000, -1.000000000000000000 ) ) ;
#24890 = VERTEX_POINT ( 'NONE', #23971 ) ;
#24891 = CARTESIAN_POINT ( 'NONE',  ( -0.9914495361339011881, 1.536537968533926657, 2.781765111341808705 ) ) ;
#24892 = DIRECTION ( 'NONE',  ( -3.469446951953613696E-16, 0.000000000000000000, -1.000000000000000000 ) ) ;
#24893 = ORIENTED_EDGE ( 'NONE', *, *, #35762, .F. ) ;
#24894 = CARTESIAN_POINT ( 'NONE',  ( 1.091055626815042645, 3.267716535433071279, -1.141732283464564013 ) ) ;
#24895 = CARTESIAN_POINT ( 'NONE',  ( -1.891551709140807169, 1.611988491233848908, 1.073772966847271526 ) ) ;
#24896 = DIRECTION ( 'NONE',  ( 1.734723475976806848E-16, -0.000000000000000000, 1.000000000000000000 ) ) ;
#24897 = DIRECTION ( 'NONE',  ( -0.000000000000000000, -1.000000000000000000, -0.000000000000000000 ) ) ;
#24898 = DIRECTION ( 'NONE',  ( -1.000000000000000000, 0.000000000000000000, -0.000000000000000000 ) ) ;
#24899 = ORIENTED_EDGE ( 'NONE', *, *, #6485, .T. ) ;
#24900 = EDGE_LOOP ( 'NONE', ( #49943, #32913, #22373, #43160, #29357, #49252, #41629, #17124 ) ) ;
#24901 = DIRECTION ( 'NONE',  ( -3.469446951953613696E-16, 0.000000000000000000, -1.000000000000000000 ) ) ;
#24902 = CARTESIAN_POINT ( 'NONE',  ( -1.439733046521776583, 3.346456692913386100, -1.259842519685034468 ) ) ;
#24903 = VERTEX_POINT ( 'NONE', #28345 ) ;
#24904 = CARTESIAN_POINT ( 'NONE',  ( -0.8182917201112814842, 0.000000000000000000, 1.102362204724404160 ) ) ;
#24905 = CARTESIAN_POINT ( 'NONE',  ( 1.560669927219590747, 0.000000000000000000, -0.7874015748031473194 ) ) ;
#24906 = CARTESIAN_POINT ( 'NONE',  ( -1.252433315296644256, 1.589416742343778610, -1.807552045033091082 ) ) ;
#24907 = CARTESIAN_POINT ( 'NONE',  ( 0.08119777152254364916, 1.623385212329073957, 0.000000000000000000 ) ) ;
#24908 = EDGE_LOOP ( 'NONE', ( #6920, #6299, #7186, #31904 ) ) ;
#24909 = VECTOR ( 'NONE', #36475, 39.37007874015748143 ) ;
#24910 = VERTEX_POINT ( 'NONE', #20611 ) ;
#24911 = EDGE_CURVE ( 'NONE', #24416, #27748, #35183, .T. ) ;
#24912 = CARTESIAN_POINT ( 'NONE',  ( -1.472219874544909768, 1.597879704547665369, 2.560030851058948898 ) ) ;
#24913 = LINE ( 'NONE', #48107, #29923 ) ;
#24914 = CARTESIAN_POINT ( 'NONE',  ( -2.438548951736695170, 3.267716535433071279, 0.1574803149606286423 ) ) ;
#24915 = ORIENTED_EDGE ( 'NONE', *, *, #45468, .F. ) ;
#24916 = FACE_OUTER_BOUND ( 'NONE', #1930, .T. ) ;
#24917 = EDGE_CURVE ( 'NONE', #9804, #49369, #1244, .T. ) ;
#24918 = FACE_BOUND ( 'NONE', #32114, .T. ) ;
#24919 = EDGE_LOOP ( 'NONE', ( #11814, #9044, #47218, #27380 ) ) ;
#24920 = CARTESIAN_POINT ( 'NONE',  ( 0.000000000000000000, 3.267716535433071279, 0.000000000000000000 ) ) ;
#24921 = ORIENTED_EDGE ( 'NONE', *, *, #46211, .F. ) ;
#24922 = VECTOR ( 'NONE', #25419, 39.37007874015748143 ) ;
#24923 = ORIENTED_EDGE ( 'NONE', *, *, #23225, .T. ) ;
#24924 = CARTESIAN_POINT ( 'NONE',  ( -2.612312576780101647, 1.576028912971601192, -0.6467214908075719082 ) ) ;
#24925 = VECTOR ( 'NONE', #27024, 39.37007874015748143 ) ;
#24926 = VERTEX_POINT ( 'NONE', #48441 ) ;
#24927 = CARTESIAN_POINT ( 'NONE',  ( 1.971247363764867977, 1.574803149606302854, -0.8960709840011636951 ) ) ;
#24928 = ORIENTED_EDGE ( 'NONE', *, *, #45299, .F. ) ;
#24929 = EDGE_CURVE ( 'NONE', #49628, #9931, #28860, .T. ) ;
#24930 = LINE ( 'NONE', #4800, #47645 ) ;
#24931 = CARTESIAN_POINT ( 'NONE',  ( 0.3664524127070866721, 0.000000000000000000, 0.07483588040983164824 ) ) ;
#24932 = PLANE ( 'NONE',  #35817 ) ;
#24933 = ADVANCED_FACE ( 'NONE', ( #2007 ), #13376, .F. ) ;
#24934 = LINE ( 'NONE', #25190, #42081 ) ;
#24935 = ADVANCED_FACE ( 'NONE', ( #37135 ), #29635, .F. ) ;
#24936 = CARTESIAN_POINT ( 'NONE',  ( 2.105931235793975009, 3.346456692913386100, -0.03937007874015936021 ) ) ;
#24937 = CARTESIAN_POINT ( 'NONE',  ( 0.000000000000000000, 2.755905511811024056, 0.000000000000000000 ) ) ;
#24938 = ORIENTED_EDGE ( 'NONE', *, *, #42275, .T. ) ;
#24939 = CYLINDRICAL_SURFACE ( 'NONE', #10993, 2.164630168518208109 ) ;
#24940 = EDGE_CURVE ( 'NONE', #33320, #42214, #7982, .T. ) ;
#24941 = DIRECTION ( 'NONE',  ( -3.469446951953613696E-16, 0.000000000000000000, -1.000000000000000000 ) ) ;
#24942 = ORIENTED_EDGE ( 'NONE', *, *, #39021, .F. ) ;
#24943 = VECTOR ( 'NONE', #35896, 39.37007874015748143 ) ;
#24944 = DIRECTION ( 'NONE',  ( -3.469446951953613696E-16, 0.000000000000000000, -1.000000000000000000 ) ) ;
#24945 = LINE ( 'NONE', #4818, #5518 ) ;
#24946 = VERTEX_POINT ( 'NONE', #48948 ) ;
#24947 = PLANE ( 'NONE',  #34515 ) ;
#24948 = DIRECTION ( 'NONE',  ( -0.000000000000000000, 0.000000000000000000, 1.000000000000000000 ) ) ;
#24949 = LINE ( 'NONE', #17966, #34278 ) ;
#24950 = VECTOR ( 'NONE', #46646, 39.37007874015748143 ) ;
#24951 = VERTEX_POINT ( 'NONE', #38151 ) ;
#24952 = AXIS2_PLACEMENT_3D ( 'NONE', #14419, #2797, #9788 ) ;
#24953 = CARTESIAN_POINT ( 'NONE',  ( 0.8182917201112824834, 3.346456692913386100, 2.047244094488179567 ) ) ;
#24954 = ORIENTED_EDGE ( 'NONE', *, *, #23910, .F. ) ;
#24955 = FACE_BOUND ( 'NONE', #19649, .T. ) ;
#24956 = DIRECTION ( 'NONE',  ( 0.01601477604151182663, -0.9998717552508123996, 0.000000000000000000 ) ) ;
#24957 = AXIS2_PLACEMENT_3D ( 'NONE', #34401, #42380, #22773 ) ;
#24958 = CONICAL_SURFACE ( 'NONE', #5158, 3.483074324928249421, 1.244861948955335196 ) ;
#24959 = CARTESIAN_POINT ( 'NONE',  ( -1.363819533518803029, 0.000000000000000000, -0.03937007874015868020 ) ) ;
#24960 = CARTESIAN_POINT ( 'NONE',  ( 0.1968503937007870241, 3.346456692913386100, -1.889763779527552146 ) ) ;
#24961 = ORIENTED_EDGE ( 'NONE', *, *, #46061, .T. ) ;
#24962 = ORIENTED_EDGE ( 'NONE', *, *, #48491, .T. ) ;
#24963 = DIRECTION ( 'NONE',  ( -1.000000000000000000, -0.000000000000000000, -0.000000000000000000 ) ) ;
#24964 = ORIENTED_EDGE ( 'NONE', *, *, #11187, .T. ) ;
#24965 = DIRECTION ( 'NONE',  ( -1.000000000000000000, 0.000000000000000000, 1.734723475976806848E-16 ) ) ;
#24966 = ORIENTED_EDGE ( 'NONE', *, *, #27877, .T. ) ;
#24967 = PLANE ( 'NONE',  #43762 ) ;
#24968 = ORIENTED_EDGE ( 'NONE', *, *, #11098, .F. ) ;
#24969 = CARTESIAN_POINT ( 'NONE',  ( -1.942732458483407365, 0.000000000000000000, 2.223636218514596585 ) ) ;
#24970 = LINE ( 'NONE', #17235, #11626 ) ;
#24971 = EDGE_CURVE ( 'NONE', #47888, #7882, #34388, .T. ) ;
#24972 = ORIENTED_EDGE ( 'NONE', *, *, #41510, .T. ) ;
#24973 = ADVANCED_FACE ( 'NONE', ( #10011 ), #41503, .F. ) ;
#24974 = DIRECTION ( 'NONE',  ( -0.000000000000000000, 1.000000000000000000, -0.000000000000000000 ) ) ;
#24975 = ORIENTED_EDGE ( 'NONE', *, *, #15879, .F. ) ;
#24976 = VERTEX_POINT ( 'NONE', #10261 ) ;
#24977 = EDGE_CURVE ( 'NONE', #33927, #10658, #17257, .T. ) ;
#24979 = ORIENTED_EDGE ( 'NONE', *, *, #33050, .F. ) ;
#24978 = ADVANCED_FACE ( 'NONE', ( #37390 ), #31921, .T. ) ;
#24980 = ORIENTED_EDGE ( 'NONE', *, *, #31199, .T. ) ;
#24981 = CARTESIAN_POINT ( 'NONE',  ( 0.000000000000000000, 3.267716535433071279, 0.000000000000000000 ) ) ;
#24982 = DIRECTION ( 'NONE',  ( 0.000000000000000000, 0.000000000000000000, -1.000000000000000000 ) ) ;
#24983 = AXIS2_PLACEMENT_3D ( 'NONE', #12014, #20781, #29288 ) ;
#24984 = ORIENTED_EDGE ( 'NONE', *, *, #12138, .T. ) ;
#24985 = DIRECTION ( 'NONE',  ( 1.734723475976806848E-16, 0.000000000000000000, 1.000000000000000000 ) ) ;
#24986 = ORIENTED_EDGE ( 'NONE', *, *, #17751, .T. ) ;
#24987 = DIRECTION ( 'NONE',  ( -3.469446951953613696E-16, 0.000000000000000000, -1.000000000000000000 ) ) ;
#24988 = VECTOR ( 'NONE', #19629, 39.37007874015748143 ) ;
#24989 = B_SPLINE_CURVE_WITH_KNOTS ( 'NONE', 3,
 ( #25545, #33313, #2058, #36666 ),
 .UNSPECIFIED., .F., .F.,
 ( 4, 4 ),
 ( 0.1211775127643062860, 0.1625894504277921315 ),
 .UNSPECIFIED. ) ;
#24990 = VECTOR ( 'NONE', #28149, 39.37007874015748143 ) ;
#24991 = EDGE_CURVE ( 'NONE', #45444, #46840, #50876, .T. ) ;
#24992 = CARTESIAN_POINT ( 'NONE',  ( 0.6363476328836782381, 3.346456692913386100, 2.007874015748021268 ) ) ;
#24993 = ORIENTED_EDGE ( 'NONE', *, *, #3811, .T. ) ;
#24994 = CARTESIAN_POINT ( 'NONE',  ( 1.497019771146616662, 1.049866565877818347, -1.363210918505332714 ) ) ;
#24995 = CARTESIAN_POINT ( 'NONE',  ( 1.287906020515830585, 3.346456692913386100, 1.574803149606291974 ) ) ;
#24996 = VECTOR ( 'NONE', #45861, 39.37007874015748143 ) ;
#24997 = DIRECTION ( 'NONE',  ( -3.469446951953613696E-16, 0.000000000000000000, -1.000000000000000000 ) ) ;
#24998 = CARTESIAN_POINT ( 'NONE',  ( 1.548545842648739956, 1.732704746525083772, 1.697655184951773810 ) ) ;
#24999 = EDGE_CURVE ( 'NONE', #22693, #39559, #14389, .T. ) ;
#25000 = DIRECTION ( 'NONE',  ( -0.000000000000000000, 1.000000000000000000, -0.000000000000000000 ) ) ;
#25001 = DIRECTION ( 'NONE',  ( -0.000000000000000000, 1.000000000000000000, -0.000000000000000000 ) ) ;
#25002 = FACE_OUTER_BOUND ( 'NONE', #10188, .T. ) ;
#25003 = VERTEX_POINT ( 'NONE', #14133 ) ;
#25004 = CARTESIAN_POINT ( 'NONE',  ( -1.236813753895212642, 5.905511811023623991, -2.681693691597581974 ) ) ;
#25005 = CARTESIAN_POINT ( 'NONE',  ( 0.002207914879453961969, 6.692913385826772199, 0.04916304461325451958 ) ) ;
#25006 = VERTEX_POINT ( 'NONE', #44849 ) ;
#25007 = CARTESIAN_POINT ( 'NONE',  ( -0.5455278134075214336, 0.000000000000000000, -0.6299212598425175669 ) ) ;
#25008 = ORIENTED_EDGE ( 'NONE', *, *, #12964, .F. ) ;
#25009 = EDGE_CURVE ( 'NONE', #41613, #19132, #30005, .T. ) ;
#25010 = DIRECTION ( 'NONE',  ( 0.000000000000000000, 1.000000000000000000, 0.000000000000000000 ) ) ;
#25011 = DIRECTION ( 'NONE',  ( -1.000000000000000000, 0.000000000000000000, 1.734723475976806848E-16 ) ) ;
#25012 = CARTESIAN_POINT ( 'NONE',  ( 0.5455278134075213226, 3.267716535433071279, -9.463399047163224412E-17 ) ) ;
#25013 = LINE ( 'NONE', #40514, #48166 ) ;
#25014 = DIRECTION ( 'NONE',  ( 0.000000000000000000, 0.000000000000000000, 1.000000000000000000 ) ) ;
#25015 = EDGE_LOOP ( 'NONE', ( #45872, #10097, #463, #50664 ) ) ;
#25016 = DIRECTION ( 'NONE',  ( 1.734723475976806848E-16, -0.000000000000000000, 1.000000000000000000 ) ) ;
#25017 = VECTOR ( 'NONE', #19365, 39.37007874015748143 ) ;
#25018 = FACE_BOUND ( 'NONE', #12353, .T. ) ;
#25019 = ORIENTED_EDGE ( 'NONE', *, *, #24119, .T. ) ;
#25020 = DIRECTION ( 'NONE',  ( -0.9998717552508121775, -0.01601477604151182316, 0.000000000000000000 ) ) ;
#25021 = VECTOR ( 'NONE', #14727, 39.37007874015748143 ) ;
#25022 = ORIENTED_EDGE ( 'NONE', *, *, #36929, .F. ) ;
#25023 = VECTOR ( 'NONE', #18991, 39.37007874015748143 ) ;
#25024 = AXIS2_PLACEMENT_3D ( 'NONE', #34024, #2012, #29639 ) ;
#25025 = LINE ( 'NONE', #36653, #46616 ) ;
#25026 = DIRECTION ( 'NONE',  ( -1.000000000000000000, 0.000000000000000000, -0.000000000000000000 ) ) ;
#25027 = DIRECTION ( 'NONE',  ( -0.000000000000000000, 1.000000000000000000, -0.000000000000000000 ) ) ;
#25028 = CONICAL_SURFACE ( 'NONE', #17628, 3.483074324928249421, 1.244861948955335196 ) ;
#25029 = CARTESIAN_POINT ( 'NONE',  ( 1.051609096396380227, 0.4349011127721513215, -1.025452293874513865 ) ) ;
#25030 = VERTEX_POINT ( 'NONE', #48693 ) ;
#25032 = ORIENTED_EDGE ( 'NONE', *, *, #6286, .F. ) ;
#25031 = EDGE_CURVE ( 'NONE', #21218, #25699, #39226, .T. ) ;
#25033 = DIRECTION ( 'NONE',  ( -0.9998717552508122886, -0.01601477604151181275, 0.000000000000000000 ) ) ;
#25034 = DIRECTION ( 'NONE',  ( -0.01601477604151182663, 0.9998717552508123996, -0.000000000000000000 ) ) ;
#25035 = FACE_BOUND ( 'NONE', #25529, .T. ) ;
#25036 = ORIENTED_EDGE ( 'NONE', *, *, #34610, .T. ) ;
#25037 = EDGE_CURVE ( 'NONE', #21877, #24313, #45599, .T. ) ;
#25038 = CARTESIAN_POINT ( 'NONE',  ( -2.277873973731453283, 1.205361022782829114E-17, 1.879489153247635214 ) ) ;
#25039 = LINE ( 'NONE', #33060, #11812 ) ;
#25040 = EDGE_CURVE ( 'NONE', #35668, #10852, #22393, .T. ) ;
#25041 = EDGE_CURVE ( 'NONE', #8712, #7499, #45099, .T. ) ;
#25042 = ORIENTED_EDGE ( 'NONE', *, *, #29651, .T. ) ;
#25043 = LINE ( 'NONE', #29686, #6810 ) ;
#25044 = CARTESIAN_POINT ( 'NONE',  ( 0.002207914879453961969, 5.905511811023623991, 0.04916304461325442243 ) ) ;
#25045 = ORIENTED_EDGE ( 'NONE', *, *, #35937, .T. ) ;
#25046 = EDGE_LOOP ( 'NONE', ( #50543, #14816, #38178, #39039 ) ) ;
#25047 = EDGE_LOOP ( 'NONE', ( #39184, #20111, #46372, #24572 ) ) ;
#25048 = CARTESIAN_POINT ( 'NONE',  ( -1.195183497228115035E-16, 3.346456692913386100, -1.259842519685035134 ) ) ;
#25049 = DIRECTION ( 'NONE',  ( 0.000000000000000000, 0.000000000000000000, 1.000000000000000000 ) ) ;
#25050 = EDGE_CURVE ( 'NONE', #9761, #23674, #34020, .T. ) ;
#25051 = DIRECTION ( 'NONE',  ( -0.000000000000000000, 1.000000000000000000, -0.000000000000000000 ) ) ;
#25052 = DIRECTION ( 'NONE',  ( 0.9998717552508121775, 0.01601477604151182663, 0.000000000000000000 ) ) ;
#25053 = ORIENTED_EDGE ( 'NONE', *, *, #28047, .T. ) ;
#25054 = ORIENTED_EDGE ( 'NONE', *, *, #49650, .F. ) ;
#25055 = CONICAL_SURFACE ( 'NONE', #38259, 3.033577403570480779, 1.554780866114618743 ) ;
#25056 = CARTESIAN_POINT ( 'NONE',  ( 1.833433833923351353, 3.267716535433071279, -0.6299212598425181220 ) ) ;
#25057 = CARTESIAN_POINT ( 'NONE',  ( 1.287906020515830141, 0.000000000000000000, 0.6299212598425161236 ) ) ;
#25058 = AXIS2_PLACEMENT_3D ( 'NONE', #40297, #16798, #32556 ) ;
#25059 = CARTESIAN_POINT ( 'NONE',  ( 1.091055626815042645, 0.000000000000000000, -0.6299212598425181220 ) ) ;
#25060 = ADVANCED_FACE ( 'NONE', ( #17755 ), #7182, .T. ) ;
#25061 = VECTOR ( 'NONE', #20369, 39.37007874015748143 ) ;
#25062 = CARTESIAN_POINT ( 'NONE',  ( 0.000000000000000000, 3.346456692913386100, 0.000000000000000000 ) ) ;
#25063 = VECTOR ( 'NONE', #29776, 39.37007874015748143 ) ;
#25064 = CARTESIAN_POINT ( 'NONE',  ( 1.833433833923351353, 0.000000000000000000, 1.259842519685033135 ) ) ;
#25065 = AXIS2_PLACEMENT_3D ( 'NONE', #34902, #19641, #8290 ) ;
#25066 = DIRECTION ( 'NONE',  ( 0.9510565162951500895, 0.000000000000000000, 0.3090169943749582204 ) ) ;
#25067 = ADVANCED_FACE ( 'NONE', ( #22643 ), #50778, .T. ) ;
#25068 = DIRECTION ( 'NONE',  ( 0.000000000000000000, 0.000000000000000000, -1.000000000000000000 ) ) ;
#25069 = AXIS2_PLACEMENT_3D ( 'NONE', #21710, #37470, #49024 ) ;
#25070 = EDGE_LOOP ( 'NONE', ( #6882, #49394, #17557, #30506 ) ) ;
#25071 = DIRECTION ( 'NONE',  ( -0.9998717552508121775, -0.01601477604151182316, 0.000000000000000000 ) ) ;
#25072 = DIRECTION ( 'NONE',  ( 0.000000000000000000, 0.000000000000000000, -1.000000000000000000 ) ) ;
#25073 = ORIENTED_EDGE ( 'NONE', *, *, #23006, .F. ) ;
#25074 = ADVANCED_FACE ( 'NONE', ( #3026 ), #13747, .F. ) ;
#25075 = ORIENTED_EDGE ( 'NONE', *, *, #49236, .T. ) ;
#25076 = DIRECTION ( 'NONE',  ( -0.7530714660036196273, 0.000000000000000000, 0.6579387259397027066 ) ) ;
#25077 = DIRECTION ( 'NONE',  ( 1.734723475976806848E-16, 0.000000000000000000, 1.000000000000000000 ) ) ;
#25078 =( BOUNDED_CURVE ( )  B_SPLINE_CURVE ( 3, ( #41216, #37344, #45309, #13335 ),
 .UNSPECIFIED., .F., .F. ) 
 B_SPLINE_CURVE_WITH_KNOTS ( ( 4, 4 ),
 ( 5.813044721214517985, 5.863817393281590462 ),
 .UNSPECIFIED. ) 
 CURVE ( )  GEOMETRIC_REPRESENTATION_ITEM ( )  RATIONAL_B_SPLINE_CURVE ( ( 1.000000000000000000, 0.9997851895178078152, 0.9997851895178078152, 1.000000000000000000 ) ) 
 REPRESENTATION_ITEM ( '' )  );
#25079 = ORIENTED_EDGE ( 'NONE', *, *, #47952, .F. ) ;
#25080 = EDGE_CURVE ( 'NONE', #34410, #20385, #29442, .T. ) ;
#25081 = VERTEX_POINT ( 'NONE', #50208 ) ;
#25082 = CARTESIAN_POINT ( 'NONE',  ( 2.168245791271198097, 5.905511811023623991, -2.004968704497247955 ) ) ;
#25083 = ORIENTED_EDGE ( 'NONE', *, *, #35626, .F. ) ;
#25084 = EDGE_CURVE ( 'NONE', #24599, #25849, #48411, .T. ) ;
#25085 = DIRECTION ( 'NONE',  ( -1.000000000000000000, 0.000000000000000000, -0.000000000000000000 ) ) ;
#25086 = LINE ( 'NONE', #5464, #21457 ) ;
#25087 = ORIENTED_EDGE ( 'NONE', *, *, #12907, .T. ) ;
#25088 = ORIENTED_EDGE ( 'NONE', *, *, #23277, .T. ) ;
#25089 = ORIENTED_EDGE ( 'NONE', *, *, #26663, .T. ) ;
#25090 = PLANE ( 'NONE',  #35395 ) ;
#25091 = VECTOR ( 'NONE', #27204, 39.37007874015748143 ) ;
#25092 = VERTEX_POINT ( 'NONE', #34772 ) ;
#25093 = ORIENTED_EDGE ( 'NONE', *, *, #10826, .T. ) ;
#25094 = CONICAL_SURFACE ( 'NONE', #48126, 2.246510896728926010, 0.01601546068027819014 ) ;
#25095 = CARTESIAN_POINT ( 'NONE',  ( 0.8182917201112819283, 3.267716535433071279, 0.5905511811023579360 ) ) ;
#25096 = CARTESIAN_POINT ( 'NONE',  ( 1.636583440222563857, 0.000000000000000000, -1.161035397307311917E-15 ) ) ;
#25097 = CARTESIAN_POINT ( 'NONE',  ( 1.770012363201889594, 3.267716535433071279, -1.141732283464564013 ) ) ;
#25098 = B_SPLINE_CURVE_WITH_KNOTS ( 'NONE', 3,
 ( #40770, #5395, #13399, #17279 ),
 .UNSPECIFIED., .F., .F.,
 ( 4, 4 ),
 ( 2.008072039916852648E-07, 0.006151689351068225821 ),
 .UNSPECIFIED. ) ;
#25099 = VECTOR ( 'NONE', #32725, 39.37007874015748143 ) ;
#25100 = EDGE_CURVE ( 'NONE', #34448, #44880, #15397, .T. ) ;
#25101 = AXIS2_PLACEMENT_3D ( 'NONE', #12052, #43018, #35547 ) ;
#25102 = ORIENTED_EDGE ( 'NONE', *, *, #41574, .T. ) ;
#25103 = CARTESIAN_POINT ( 'NONE',  ( 0.000000000000000000, 3.267716535433071279, -0.6299212598425177889 ) ) ;
#25104 = DIRECTION ( 'NONE',  ( 0.9998717552508121775, 0.01601477604151182663, 0.000000000000000000 ) ) ;
#25105 = DIRECTION ( 'NONE',  ( 1.734723475976806848E-16, -0.000000000000000000, 1.000000000000000000 ) ) ;
#25106 = ADVANCED_FACE ( 'NONE', ( #19264 ), #19511, .F. ) ;
#25107 = ORIENTED_EDGE ( 'NONE', *, *, #47196, .F. ) ;
#25108 = PLANE ( 'NONE',  #38115 ) ;
#25109 = CARTESIAN_POINT ( 'NONE',  ( -1.636583440222563635, 0.000000000000000000, 1.062992125984246083 ) ) ;
#25110 = AXIS2_PLACEMENT_3D ( 'NONE', #25007, #37405, #16759 ) ;
#25111 = PLANE ( 'NONE',  #13416 ) ;
#25112 = VERTEX_POINT ( 'NONE', #18522 ) ;
#25113 = ORIENTED_EDGE ( 'NONE', *, *, #24554, .T. ) ;
#25114 = PLANE ( 'NONE',  #32182 ) ;
#25115 = CARTESIAN_POINT ( 'NONE',  ( 1.325491792074623643, 0.000000000000000000, -2.638988599164732385 ) ) ;
#25116 = LINE ( 'NONE', #31854, #18899 ) ;
#25117 = ORIENTED_EDGE ( 'NONE', *, *, #2663, .F. ) ;
#25118 = ORIENTED_EDGE ( 'NONE', *, *, #3487, .F. ) ;
#25119 = DIRECTION ( 'NONE',  ( 0.000000000000000000, 0.000000000000000000, 1.000000000000000000 ) ) ;
#25120 = VERTEX_POINT ( 'NONE', #49963 ) ;
#25121 = DIRECTION ( 'NONE',  ( -0.9998717552508121775, -0.01601477604151182316, 0.000000000000000000 ) ) ;
#25122 = FACE_OUTER_BOUND ( 'NONE', #32038, .T. ) ;
#25123 = EDGE_CURVE ( 'NONE', #10879, #12204, #18771, .T. ) ;
#25124 = CARTESIAN_POINT ( 'NONE',  ( -2.138597145901436125, 6.692913385826772199, 0.3393547186366932533 ) ) ;
#25125 = DIRECTION ( 'NONE',  ( -3.469446951953613696E-16, 0.000000000000000000, -1.000000000000000000 ) ) ;
#25126 = CARTESIAN_POINT ( 'NONE',  ( 0.002207914879453961969, 5.905511811023623991, 0.04916304461325442243 ) ) ;
#25127 = VERTEX_POINT ( 'NONE', #27516 ) ;
#25128 = AXIS2_PLACEMENT_3D ( 'NONE', #10961, #30838, #19204 ) ;
#25129 = LINE ( 'NONE', #40881, #34905 ) ;
#25130 = VECTOR ( 'NONE', #40817, 39.37007874015748143 ) ;
#25131 = LINE ( 'NONE', #49089, #16658 ) ;
#25132 = EDGE_CURVE ( 'NONE', #25457, #41221, #19013, .T. ) ;
#25133 = VECTOR ( 'NONE', #13024, 39.37007874015748143 ) ;
#25134 = ORIENTED_EDGE ( 'NONE', *, *, #11105, .F. ) ;
#25135 = DIRECTION ( 'NONE',  ( 0.000000000000000000, -1.000000000000000000, -0.000000000000000000 ) ) ;
#25136 = EDGE_CURVE ( 'NONE', #47240, #44618, #39148, .T. ) ;
#25137 = DIRECTION ( 'NONE',  ( 0.01601477604151182663, -0.9998717552508123996, 0.000000000000000000 ) ) ;
#25138 = DIRECTION ( 'NONE',  ( -0.01601477604151182663, 0.9998717552508123996, -0.000000000000000000 ) ) ;
#25140 = EDGE_CURVE ( 'NONE', #33320, #33364, #46359, .T. ) ;
#25139 = ORIENTED_EDGE ( 'NONE', *, *, #3360, .T. ) ;
#25141 = LINE ( 'NONE', #9389, #49701 ) ;
#25142 = PLANE ( 'NONE',  #18470 ) ;
#25143 = VECTOR ( 'NONE', #39770, 39.37007874015748143 ) ;
#25144 = ADVANCED_FACE ( 'NONE', ( #50454 ), #26761, .F. ) ;
#25145 = ORIENTED_EDGE ( 'NONE', *, *, #39645, .F. ) ;
#25146 = CARTESIAN_POINT ( 'NONE',  ( 1.769879628650530723, 0.05626752682809384870, -0.8100022834900426627 ) ) ;
#25147 = DIRECTION ( 'NONE',  ( -3.469446951953613696E-16, 0.000000000000000000, -1.000000000000000000 ) ) ;
#25148 = ORIENTED_EDGE ( 'NONE', *, *, #11116, .F. ) ;
#25149 = CARTESIAN_POINT ( 'NONE',  ( -1.091055626815042201, 0.000000000000000000, 0.7480314960629874665 ) ) ;
#25150 = CARTESIAN_POINT ( 'NONE',  ( -0.2727639067037604392, 3.267716535433071279, 4.731699523581607892E-17 ) ) ;
#25151 = DIRECTION ( 'NONE',  ( -0.000000000000000000, 0.000000000000000000, 1.000000000000000000 ) ) ;
#25152 = FACE_OUTER_BOUND ( 'NONE', #38153, .T. ) ;
#25153 = DIRECTION ( 'NONE',  ( 0.9989930665413151445, 5.167793568183051143E-18, -0.04486483035050446017 ) ) ;
#25154 = ORIENTED_EDGE ( 'NONE', *, *, #27, .T. ) ;
#25155 = ORIENTED_EDGE ( 'NONE', *, *, #29460, .F. ) ;
#25156 = CARTESIAN_POINT ( 'NONE',  ( -1.420868632364155282, 0.000000000000000000, 1.070159647439151707 ) ) ;
#25157 = CARTESIAN_POINT ( 'NONE',  ( -1.636583440222564301, 3.346456692913386100, -1.141732283464563791 ) ) ;
#25158 = EDGE_LOOP ( 'NONE', ( #46153, #38759, #24190, #22960 ) ) ;
#25159 = CARTESIAN_POINT ( 'NONE',  ( -2.734482843737247038, 1.578211097029592169, -1.115254632218712016 ) ) ;
#25160 = CARTESIAN_POINT ( 'NONE',  ( 0.000000000000000000, 3.267716535433071279, 0.1574803149606280872 ) ) ;
#25161 = CARTESIAN_POINT ( 'NONE',  ( -1.252307872741886374, 1.622227152372770487, -1.807379388168664613 ) ) ;
#25162 = ADVANCED_FACE ( 'NONE', ( #11280 ), #27008, .F. ) ;
#25163 = CARTESIAN_POINT ( 'NONE',  ( 1.909347346926324684, 3.267716535433071279, -0.6692913385826764205 ) ) ;
#25164 = VERTEX_POINT ( 'NONE', #15409 ) ;
#25165 = ORIENTED_EDGE ( 'NONE', *, *, #44360, .T. ) ;
#25166 = CARTESIAN_POINT ( 'NONE',  ( -1.166969139818015977, 0.000000000000000000, -0.4724409448818886470 ) ) ;
#25167 = DIRECTION ( 'NONE',  ( -0.000000000000000000, 1.000000000000000000, -0.000000000000000000 ) ) ;
#25168 = CARTESIAN_POINT ( 'NONE',  ( 0.04921259842519669359, 1.621581020286960051, 2.952755905511811108 ) ) ;
#25169 = EDGE_CURVE ( 'NONE', #13855, #11136, #46860, .T. ) ;
#25170 = VERTEX_POINT ( 'NONE', #7652 ) ;
#25171 = DIRECTION ( 'NONE',  ( 1.000000000000000000, 0.000000000000000000, 0.000000000000000000 ) ) ;
#25172 = FACE_BOUND ( 'NONE', #34915, .T. ) ;
#25173 = VECTOR ( 'NONE', #13194, 39.37007874015748143 ) ;
#25174 = ORIENTED_EDGE ( 'NONE', *, *, #11037, .T. ) ;
#25175 = VECTOR ( 'NONE', #43361, 39.37007874015748143 ) ;
#25176 = CARTESIAN_POINT ( 'NONE',  ( 0.8182917201112817063, 3.346456692913386100, -1.614173228346451605 ) ) ;
#25177 = VECTOR ( 'NONE', #12880, 39.37007874015748143 ) ;
#25178 = VERTEX_POINT ( 'NONE', #23393 ) ;
#25179 = ORIENTED_EDGE ( 'NONE', *, *, #49941, .T. ) ;
#25180 = CARTESIAN_POINT ( 'NONE',  ( 0.08119777152254364916, 1.623385212329073957, 0.000000000000000000 ) ) ;
#25181 = AXIS2_PLACEMENT_3D ( 'NONE', #3175, #23048, #30546 ) ;
#25182 = ORIENTED_EDGE ( 'NONE', *, *, #6221, .F. ) ;
#25183 = DIRECTION ( 'NONE',  ( 0.000000000000000000, 0.000000000000000000, 1.000000000000000000 ) ) ;
#25184 = EDGE_CURVE ( 'NONE', #3567, #19884, #19518, .T. ) ;
#25185 = CARTESIAN_POINT ( 'NONE',  ( -2.164823134740035737, 6.692913385826772199, -0.04796011690018289753 ) ) ;
#25186 = ORIENTED_EDGE ( 'NONE', *, *, #46450, .T. ) ;
#25187 = AXIS2_PLACEMENT_3D ( 'NONE', #2492, #25464, #37869 ) ;
#25188 = DIRECTION ( 'NONE',  ( -0.000000000000000000, 1.000000000000000000, -0.000000000000000000 ) ) ;
#25189 = CARTESIAN_POINT ( 'NONE',  ( 1.560669927219590747, 3.346456692913386100, 0.1574803149606283648 ) ) ;
#25190 = CARTESIAN_POINT ( 'NONE',  ( 1.833433833923351353, 3.346456692913386100, 1.574803149606291974 ) ) ;
#25191 = DIRECTION ( 'NONE',  ( 0.000000000000000000, 0.000000000000000000, -1.000000000000000000 ) ) ;
#25192 = CARTESIAN_POINT ( 'NONE',  ( -1.220415235146723454, 0.5160455853568218787, -2.362204724409449064 ) ) ;
#25193 = ORIENTED_EDGE ( 'NONE', *, *, #34832, .T. ) ;
#25194 = DIRECTION ( 'NONE',  ( 1.000000000000000000, 0.000000000000000000, 0.000000000000000000 ) ) ;
#25195 = CARTESIAN_POINT ( 'NONE',  ( -1.363819533518803473, 0.000000000000000000, -0.4724409448818886470 ) ) ;
#25196 = VERTEX_POINT ( 'NONE', #31405 ) ;
#25197 = CARTESIAN_POINT ( 'NONE',  ( 2.313772584725266146, 1.653356997568332210, -1.468340530687288981 ) ) ;
#25198 = EDGE_CURVE ( 'NONE', #1172, #36221, #7905, .T. ) ;
#25199 = LINE ( 'NONE', #40956, #40944 ) ;
#25200 = VERTEX_POINT ( 'NONE', #15903 ) ;
#25201 = LINE ( 'NONE', #13333, #7302 ) ;
#25202 = EDGE_CURVE ( 'NONE', #22897, #536, #35536, .T. ) ;
#25203 = CARTESIAN_POINT ( 'NONE',  ( 0.000000000000000000, 1.574803149606302854, 0.000000000000000000 ) ) ;
#25204 = EDGE_CURVE ( 'NONE', #9920, #13689, #3088, .T. ) ;
#25205 = DIRECTION ( 'NONE',  ( -0.000000000000000000, -1.000000000000000000, 0.000000000000000000 ) ) ;
#25206 = AXIS2_PLACEMENT_3D ( 'NONE', #15473, #31223, #11591 ) ;
#25207 = AXIS2_PLACEMENT_3D ( 'NONE', #19569, #35085, #15205 ) ;
#25208 = VERTEX_POINT ( 'NONE', #20552 ) ;
#25209 = FACE_OUTER_BOUND ( 'NONE', #46990, .T. ) ;
#25210 = ORIENTED_EDGE ( 'NONE', *, *, #16667, .T. ) ;
#25211 = FACE_BOUND ( 'NONE', #34861, .T. ) ;
#25212 = VECTOR ( 'NONE', #26176, 39.37007874015748143 ) ;
#25213 = CARTESIAN_POINT ( 'NONE',  ( 0.08139965876239094178, 1.610780518492231694, 0.000000000000000000 ) ) ;
#25214 = CARTESIAN_POINT ( 'NONE',  ( 0.08139965876239094178, 1.610780518492231694, 0.000000000000000000 ) ) ;
#25215 = FACE_OUTER_BOUND ( 'NONE', #1228, .T. ) ;
#25216 = CIRCLE ( 'NONE', #16150, 2.165354330708661568 ) ;
#25217 = EDGE_LOOP ( 'NONE', ( #41885, #48991, #41439, #46502 ) ) ;
#25218 = VERTEX_POINT ( 'NONE', #40441 ) ;
#25219 = CARTESIAN_POINT ( 'NONE',  ( 1.022166022721139322, 1.636725766563431606, 2.770237021105635300 ) ) ;
#25220 = VERTEX_POINT ( 'NONE', #4291 ) ;
#25221 = ADVANCED_FACE ( 'NONE', ( #28803 ), #12967, .F. ) ;
#25222 = CARTESIAN_POINT ( 'NONE',  ( 0.5455278134075216556, 3.346456692913386100, 2.007874015748021268 ) ) ;
#25223 = VERTEX_POINT ( 'NONE', #4044 ) ;
#25224 = LINE ( 'NONE', #44571, #5013 ) ;
#25225 = EDGE_CURVE ( 'NONE', #49076, #13566, #39404, .T. ) ;
#25226 = VERTEX_POINT ( 'NONE', #36307 ) ;
#25227 = PLANE ( 'NONE',  #23271 ) ;
#25228 = EDGE_CURVE ( 'NONE', #15126, #29929, #30286, .T. ) ;
#25229 = DIRECTION ( 'NONE',  ( 1.734723475976806848E-16, -0.000000000000000000, 1.000000000000000000 ) ) ;
#25230 = ORIENTED_EDGE ( 'NONE', *, *, #42861, .T. ) ;
#25231 = ADVANCED_FACE ( 'NONE', ( #20287 ), #8424, .F. ) ;
#25232 = LINE ( 'NONE', #40991, #21603 ) ;
#25233 = ORIENTED_EDGE ( 'NONE', *, *, #30590, .F. ) ;
#25234 = ORIENTED_EDGE ( 'NONE', *, *, #26415, .F. ) ;
#25235 = VECTOR ( 'NONE', #12679, 39.37007874015748143 ) ;
#25236 = ORIENTED_EDGE ( 'NONE', *, *, #33676, .F. ) ;
#25237 = EDGE_LOOP ( 'NONE', ( #37347, #17333, #18436, #31651 ) ) ;
#25238 = CARTESIAN_POINT ( 'NONE',  ( -0.2727639067037607723, 3.346456692913386100, 2.362204724409437961 ) ) ;
#25239 = VECTOR ( 'NONE', #41334, 39.37007874015748143 ) ;
#25240 = CIRCLE ( 'NONE', #2173, 2.246510896728926010 ) ;
#25241 = EDGE_LOOP ( 'NONE', ( #28259, #47689, #31216, #26573 ) ) ;
#25242 = CARTESIAN_POINT ( 'NONE',  ( 0.000000000000000000, 0.000000000000000000, -1.968503937007874072 ) ) ;
#25243 = VECTOR ( 'NONE', #22552, 39.37007874015748143 ) ;
#25244 = ORIENTED_EDGE ( 'NONE', *, *, #12323, .F. ) ;
#25245 = CARTESIAN_POINT ( 'NONE',  ( 0.4696143004045479352, 0.000000000000000000, -1.417322834645664331 ) ) ;
#25246 = AXIS2_PLACEMENT_3D ( 'NONE', #26935, #42681, #23072 ) ;
#25247 = PLANE ( 'NONE',  #29705 ) ;
#25248 = EDGE_LOOP ( 'NONE', ( #45340, #1369, #3941, #43410 ) ) ;
#25249 = VECTOR ( 'NONE', #43487, 39.37007874015748143 ) ;
#25250 = CARTESIAN_POINT ( 'NONE',  ( -1.091055626815042645, 0.000000000000000000, -0.3149606299212593941 ) ) ;
#25251 = LINE ( 'NONE', #44094, #50827 ) ;
#25252 = B_SPLINE_CURVE_WITH_KNOTS ( 'NONE', 3,
 ( #25168, #13048, #1161, #6052 ),
 .UNSPECIFIED., .F., .F.,
 ( 4, 4 ),
 ( 0.0008137531722819554792, 0.003314056422229540947 ),
 .UNSPECIFIED. ) ;
#25253 = VERTEX_POINT ( 'NONE', #48384 ) ;
#25254 = LINE ( 'NONE', #33267, #21678 ) ;
#25255 = PLANE ( 'NONE',  #50536 ) ;
#25256 = CARTESIAN_POINT ( 'NONE',  ( -0.3498457532482182053, 1.702298530840201662, 2.203421978946157989 ) ) ;
#25257 = DIRECTION ( 'NONE',  ( -0.9998717552508121775, -0.01601477604151182316, 0.000000000000000000 ) ) ;
#25258 = ORIENTED_EDGE ( 'NONE', *, *, #33795, .T. ) ;
#25259 = CARTESIAN_POINT ( 'NONE',  ( 0.7423782071083084855, 3.267716535433071279, -2.575641807848709208E-16 ) ) ;
#25260 = CARTESIAN_POINT ( 'NONE',  ( 2.106197740627111958, 3.267716535433071279, -7.307341331430321661E-16 ) ) ;
#25261 = EDGE_CURVE ( 'NONE', #19068, #24661, #13072, .T. ) ;
#25262 = VERTEX_POINT ( 'NONE', #28033 ) ;
#25263 = DIRECTION ( 'NONE',  ( -0.5128992774059071280, 0.000000000000000000, 0.8584487936018655452 ) ) ;
#25264 = EDGE_CURVE ( 'NONE', #6293, #33009, #8168, .T. ) ;
#25265 = ORIENTED_EDGE ( 'NONE', *, *, #49143, .T. ) ;
#25266 = LINE ( 'NONE', #37407, #17092 ) ;
#25267 = ADVANCED_FACE ( 'NONE', ( #47359 ), #47622, .F. ) ;
#25268 = CARTESIAN_POINT ( 'NONE',  ( -1.712496953225537188, 0.000000000000000000, 0.7874015748031456541 ) ) ;
#25269 = CARTESIAN_POINT ( 'NONE',  ( -0.6393972184786450574, 0.000000000000000000, 1.750134138416205687 ) ) ;
#25270 = B_SPLINE_CURVE_WITH_KNOTS ( 'NONE', 3,
 ( #9790, #49237, #37418, #41285 ),
 .UNSPECIFIED., .F., .F.,
 ( 4, 4 ),
 ( 2.271194419226085044E-07, 0.01976584882222652551 ),
 .UNSPECIFIED. ) ;
#25271 = LINE ( 'NONE', #38176, #30891 ) ;
#25272 = DIRECTION ( 'NONE',  ( 1.000000000000000000, -0.000000000000000000, 0.000000000000000000 ) ) ;
#25273 = ORIENTED_EDGE ( 'NONE', *, *, #19103, .T. ) ;
#25274 = AXIS2_PLACEMENT_3D ( 'NONE', #9456, #21584, #38104 ) ;
#25275 = CARTESIAN_POINT ( 'NONE',  ( 1.748857742710046237, 1.648042031076149883, -2.379187494666238134 ) ) ;
#25276 = VECTOR ( 'NONE', #19509, 39.37007874015748143 ) ;
#25277 = FACE_BOUND ( 'NONE', #39805, .T. ) ;
#25278 = VECTOR ( 'NONE', #4737, 39.37007874015748143 ) ;
#25279 = ORIENTED_EDGE ( 'NONE', *, *, #22631, .F. ) ;
#25280 = CARTESIAN_POINT ( 'NONE',  ( 2.378961647330872786, 3.255931344577397191, 0.5824936282491406381 ) ) ;
#25281 = ORIENTED_EDGE ( 'NONE', *, *, #49878, .F. ) ;
#25282 = LINE ( 'NONE', #30111, #2954 ) ;
#25283 = LINE ( 'NONE', #33048, #27224 ) ;
#25284 = EDGE_CURVE ( 'NONE', #1622, #4594, #675, .T. ) ;
#25285 = DIRECTION ( 'NONE',  ( 0.9009688679024154823, -1.160734090543304660E-16, 0.4338837391175656699 ) ) ;
#25286 = VECTOR ( 'NONE', #31065, 39.37007874015748143 ) ;
#25287 = DIRECTION ( 'NONE',  ( -0.01601477604151182663, 0.9998717552508123996, -0.000000000000000000 ) ) ;
#25288 = ORIENTED_EDGE ( 'NONE', *, *, #43360, .F. ) ;
#25289 = VERTEX_POINT ( 'NONE', #5061 ) ;
#25290 = EDGE_CURVE ( 'NONE', #2346, #13212, #24173, .T. ) ;
#25291 = CARTESIAN_POINT ( 'NONE',  ( -2.159905143290285601, 6.332733149760729319, 0.1535224723189610174 ) ) ;
#25292 = DIRECTION ( 'NONE',  ( -0.4338837391175526803, 1.045958227173635857E-16, -0.9009688679024218105 ) ) ;
#25293 = FACE_BOUND ( 'NONE', #29917, .T. ) ;
#25294 = EDGE_LOOP ( 'NONE', ( #7316, #11601, #6236, #48997 ) ) ;
#25295 = LINE ( 'NONE', #25038, #3929 ) ;
#25296 = CARTESIAN_POINT ( 'NONE',  ( 0.000000000000000000, 3.267716535433071279, 1.574803149606291974 ) ) ;
#25297 = EDGE_LOOP ( 'NONE', ( #50870, #23219, #5221, #4426 ) ) ;
#25298 = PLANE ( 'NONE',  #47965 ) ;
#25299 = DIRECTION ( 'NONE',  ( -3.986037398843765983E-20, -1.000000000000000000, -1.160734090543304660E-16 ) ) ;
#25300 = VERTEX_POINT ( 'NONE', #415 ) ;
#25301 = ORIENTED_EDGE ( 'NONE', *, *, #5442, .T. ) ;
#25302 = VERTEX_POINT ( 'NONE', #44540 ) ;
#25303 = CARTESIAN_POINT ( 'NONE',  ( 1.558105373646060388, 3.346456692913386100, 1.417322834645662777 ) ) ;
#25305 = LINE ( 'NONE', #21439, #39909 ) ;
#25304 = VECTOR ( 'NONE', #2977, 39.37007874015748143 ) ;
#25306 = CARTESIAN_POINT ( 'NONE',  ( 2.278027606577265107, 1.645963535160160696, -0.4694667435916627385 ) ) ;
#25307 = ORIENTED_EDGE ( 'NONE', *, *, #28012, .T. ) ;
#25308 = ORIENTED_EDGE ( 'NONE', *, *, #8200, .F. ) ;
#25310 = VECTOR ( 'NONE', #18838, 39.37007874015748854 ) ;
#25309 = CARTESIAN_POINT ( 'NONE',  ( 1.162932091021788183, 1.205361022782829114E-17, -1.684364178081092067 ) ) ;
#25311 = DIRECTION ( 'NONE',  ( 0.000000000000000000, -0.7660444431189770143, 0.6427876096865403621 ) ) ;
#25312 = FACE_OUTER_BOUND ( 'NONE', #47848, .T. ) ;
#25313 = CARTESIAN_POINT ( 'NONE',  ( 1.636583440222563857, 3.346456692913386100, -0.8267716535433055070 ) ) ;
#25314 = FACE_OUTER_BOUND ( 'NONE', #26456, .T. ) ;
#25315 = VECTOR ( 'NONE', #11141, 39.37007874015748143 ) ;
#25316 = B_SPLINE_CURVE_WITH_KNOTS ( 'NONE', 3,
 ( #13110, #28324, #1229, #5356 ),
 .UNSPECIFIED., .F., .F.,
 ( 4, 4 ),
 ( 2.175066537435804214E-07, 0.002500264305833190676 ),
 .UNSPECIFIED. ) ;
#25317 = CARTESIAN_POINT ( 'NONE',  ( 1.720314620805546646, 0.000000000000000000, 0.2826945007888405637 ) ) ;
#25318 = B_SPLINE_CURVE_WITH_KNOTS ( 'NONE', 3,
 ( #4559, #16440, #31938, #35800 ),
 .UNSPECIFIED., .F., .F.,
 ( 4, 4 ),
 ( 9.107130028278628622E-06, 2.039057899801572380E-05 ),
 .UNSPECIFIED. ) ;
#25319 = EDGE_CURVE ( 'NONE', #16395, #37228, #39917, .T. ) ;
#25320 = ORIENTED_EDGE ( 'NONE', *, *, #48344, .F. ) ;
#25321 = DIRECTION ( 'NONE',  ( 1.734723475976806848E-16, -0.000000000000000000, 1.000000000000000000 ) ) ;
#25322 = CARTESIAN_POINT ( 'NONE',  ( 1.091055626815042423, 3.346456692913386100, -1.771653543307081691 ) ) ;
#25323 = EDGE_CURVE ( 'NONE', #21738, #42844, #44033, .T. ) ;
#25324 = ORIENTED_EDGE ( 'NONE', *, *, #46915, .F. ) ;
#25325 = EDGE_CURVE ( 'NONE', #38556, #8556, #16946, .T. ) ;
#25326 = ORIENTED_EDGE ( 'NONE', *, *, #47608, .T. ) ;
#25327 = DIRECTION ( 'NONE',  ( 0.6579387259397027066, 0.000000000000000000, 0.7530714660036195163 ) ) ;
#25328 = CARTESIAN_POINT ( 'NONE',  ( -1.166969139818015977, 3.267716535433071279, 4.048737525165546155E-16 ) ) ;
#25329 = EDGE_CURVE ( 'NONE', #31055, #31998, #35790, .T. ) ;
#25330 = ORIENTED_EDGE ( 'NONE', *, *, #4983, .F. ) ;
#25331 = EDGE_CURVE ( 'NONE', #10406, #45153, #43771, .T. ) ;
#25332 = ORIENTED_EDGE ( 'NONE', *, *, #39312, .F. ) ;
#25333 = DIRECTION ( 'NONE',  ( -0.000000000000000000, 1.000000000000000000, -0.000000000000000000 ) ) ;
#25334 = ORIENTED_EDGE ( 'NONE', *, *, #45086, .T. ) ;
#25335 = CARTESIAN_POINT ( 'NONE',  ( -1.985260859929297794, 3.346456692913386100, -0.1968503937007880511 ) ) ;
#25336 = LINE ( 'NONE', #17849, #41252 ) ;
#25337 = EDGE_CURVE ( 'NONE', #48833, #34963, #49405, .T. ) ;
#25338 = VECTOR ( 'NONE', #40349, 39.37007874015748143 ) ;
#25339 = VECTOR ( 'NONE', #4173, 39.37007874015748143 ) ;
#25340 = ORIENTED_EDGE ( 'NONE', *, *, #26886, .T. ) ;
#25341 = VERTEX_POINT ( 'NONE', #45293 ) ;
#25342 = ORIENTED_EDGE ( 'NONE', *, *, #9993, .T. ) ;
#25343 = AXIS2_PLACEMENT_3D ( 'NONE', #42760, #7406, #50702 ) ;
#25344 = CARTESIAN_POINT ( 'NONE',  ( 0.000000000000000000, 3.346456692913386100, 0.000000000000000000 ) ) ;
#25345 = ORIENTED_EDGE ( 'NONE', *, *, #49799, .T. ) ;
#25346 = ORIENTED_EDGE ( 'NONE', *, *, #12542, .F. ) ;
#25347 = EDGE_CURVE ( 'NONE', #30593, #41937, #29831, .T. ) ;
#25348 = CARTESIAN_POINT ( 'NONE',  ( 0.000000000000000000, 3.267716535433071279, 0.000000000000000000 ) ) ;
#25349 = PLANE ( 'NONE',  #41753 ) ;
#25350 = DIRECTION ( 'NONE',  ( 0.1938878870612535943, 0.000000000000000000, 0.9810236935216818388 ) ) ;
#25351 = EDGE_LOOP ( 'NONE', ( #22837, #37059, #26210, #11386 ) ) ;
#25352 = DIRECTION ( 'NONE',  ( 0.000000000000000000, 1.000000000000000000, 0.000000000000000000 ) ) ;
#25353 = DIRECTION ( 'NONE',  ( 0.01601477604151182663, -0.9998717552508123996, 0.000000000000000000 ) ) ;
#25354 = EDGE_CURVE ( 'NONE', #35441, #40968, #9704, .T. ) ;
#25355 = DIRECTION ( 'NONE',  ( -0.7818314824680309139, 0.000000000000000000, 0.6234898018587318180 ) ) ;
#25356 = ORIENTED_EDGE ( 'NONE', *, *, #12847, .T. ) ;
#25357 = DIRECTION ( 'NONE',  ( -3.469446951953613696E-16, 0.000000000000000000, -1.000000000000000000 ) ) ;
#25358 = CARTESIAN_POINT ( 'NONE',  ( -2.182111253630085290, 0.000000000000000000, 0.9448818897637749625 ) ) ;
#25359 = PLANE ( 'NONE',  #40618 ) ;
#25360 = EDGE_LOOP ( 'NONE', ( #27863, #11059, #16065, #35925 ) ) ;
#25361 = ORIENTED_EDGE ( 'NONE', *, *, #35945, .F. ) ;
#25362 =( CONVERSION_BASED_UNIT ( 'INCH', #36995 ) LENGTH_UNIT ( ) NAMED_UNIT ( #28796 ) );
#25363 = VECTOR ( 'NONE', #28288, 39.37007874015748143 ) ;
#25364 = EDGE_CURVE ( 'NONE', #9169, #17362, #21576, .T. ) ;
#25365 = DIRECTION ( 'NONE',  ( 1.734723475976806848E-16, -0.000000000000000000, 1.000000000000000000 ) ) ;
#25366 = CARTESIAN_POINT ( 'NONE',  ( 1.550261229843175492, 1.634307024739966696, 1.699618603577774945 ) ) ;
#25367 = DIRECTION ( 'NONE',  ( 0.9959742939952397345, 0.000000000000000000, -0.08963930890342654279 ) ) ;
#25368 = ORIENTED_EDGE ( 'NONE', *, *, #7017, .F. ) ;
#25369 = ORIENTED_EDGE ( 'NONE', *, *, #35422, .T. ) ;
#25370 = DIRECTION ( 'NONE',  ( -0.9510565162951544194, 0.000000000000000000, 0.3090169943749447312 ) ) ;
#25371 = ORIENTED_EDGE ( 'NONE', *, *, #10349, .T. ) ;
#25372 = PLANE ( 'NONE',  #15080 ) ;
#25373 = CARTESIAN_POINT ( 'NONE',  ( -1.690941099774203815, 0.0008361491594236539725, -0.4364244636917575804 ) ) ;
#25374 = CIRCLE ( 'NONE', #24563, 2.244934639244525076 ) ;
#25375 = DIRECTION ( 'NONE',  ( 1.000000000000000000, 0.000000000000000000, 0.000000000000000000 ) ) ;
#25376 = DIRECTION ( 'NONE',  ( 0.000000000000000000, -1.000000000000000000, 0.000000000000000000 ) ) ;
#25377 = CARTESIAN_POINT ( 'NONE',  ( 0.7423782071083091516, 0.000000000000000000, 1.692913385826762873 ) ) ;
#25378 = ORIENTED_EDGE ( 'NONE', *, *, #15177, .T. ) ;
#25379 = DIRECTION ( 'NONE',  ( 1.000000000000000000, 0.000000000000000000, 0.000000000000000000 ) ) ;
#25380 = VECTOR ( 'NONE', #22498, 39.37007874015748143 ) ;
#25381 = FACE_OUTER_BOUND ( 'NONE', #1261, .T. ) ;
#25382 = EDGE_CURVE ( 'NONE', #35273, #51000, #48637, .T. ) ;
#25383 = ORIENTED_EDGE ( 'NONE', *, *, #43118, .T. ) ;
#25384 = DIRECTION ( 'NONE',  ( -0.000000000000000000, 1.000000000000000000, -0.000000000000000000 ) ) ;
#25385 = CARTESIAN_POINT ( 'NONE',  ( 0.002207914879453961969, 6.692913385826772199, 0.04916304461325451958 ) ) ;
#25386 = CARTESIAN_POINT ( 'NONE',  ( 1.909347346926324684, 0.000000000000000000, -0.6692913385826764205 ) ) ;
#25387 = ORIENTED_EDGE ( 'NONE', *, *, #49316, .F. ) ;
#25388 = CARTESIAN_POINT ( 'NONE',  ( 2.277873973731426194, 0.000000000000000000, 1.879489153247667854 ) ) ;
#25389 = EDGE_CURVE ( 'NONE', #4391, #20592, #25697, .T. ) ;
#25390 = VECTOR ( 'NONE', #6191, 39.37007874015748143 ) ;
#25391 = CARTESIAN_POINT ( 'NONE',  ( -0.6214413264104939882, 3.346456692913386100, 0.7874015748031456541 ) ) ;
#25392 = ORIENTED_EDGE ( 'NONE', *, *, #26161, .T. ) ;
#25393 = CARTESIAN_POINT ( 'NONE',  ( -0.5455278134075214336, 3.346456692913386100, 0.1181102362204703021 ) ) ;
#25394 = CARTESIAN_POINT ( 'NONE',  ( 0.04921259842519689481, 0.000000000000000000, 1.742692369722729895 ) ) ;
#25395 = ORIENTED_EDGE ( 'NONE', *, *, #19491, .T. ) ;
#25396 = VECTOR ( 'NONE', #5762, 39.37007874015748143 ) ;
#25397 = CARTESIAN_POINT ( 'NONE',  ( 3.927031490892378253E-16, 3.267716535433071279, 1.377952755905504256 ) ) ;
#25398 = CARTESIAN_POINT ( 'NONE',  ( -0.5455278134075214336, 0.000000000000000000, 0.1181102362204703021 ) ) ;
#25399 = CARTESIAN_POINT ( 'NONE',  ( 1.091055626815042423, 0.000000000000000000, -1.456692913385822630 ) ) ;
#25400 = LINE ( 'NONE', #21530, #40842 ) ;
#25401 = CARTESIAN_POINT ( 'NONE',  ( -2.161044708975090156, 5.905511811023623991, 0.1463148319730357971 ) ) ;
#25402 = ORIENTED_EDGE ( 'NONE', *, *, #18064, .F. ) ;
#25403 = ORIENTED_EDGE ( 'NONE', *, *, #22890, .F. ) ;
#25404 = DIRECTION ( 'NONE',  ( -0.000000000000000000, 1.000000000000000000, -0.000000000000000000 ) ) ;
#25405 = DIRECTION ( 'NONE',  ( 0.000000000000000000, 0.000000000000000000, -1.000000000000000000 ) ) ;
#25406 = ORIENTED_EDGE ( 'NONE', *, *, #13715, .F. ) ;
#25407 = DIRECTION ( 'NONE',  ( -0.9909497617679352555, -1.554141314384320336E-17, 0.1342332658176522420 ) ) ;
#25408 = LINE ( 'NONE', #45511, #34356 ) ;
#25409 = CARTESIAN_POINT ( 'NONE',  ( -1.091055626815042645, 3.346456692913386100, -2.086614173228339641 ) ) ;
#25410 = EDGE_LOOP ( 'NONE', ( #15526, #35172, #45406, #31041 ) ) ;
#25411 = VERTEX_POINT ( 'NONE', #9448 ) ;
#25412 = CARTESIAN_POINT ( 'NONE',  ( 1.091055626815042645, 3.267716535433071279, 0.6299212598425161236 ) ) ;
#25413 = DIRECTION ( 'NONE',  ( -1.000000000000000000, 0.000000000000000000, -0.000000000000000000 ) ) ;
#25414 = ADVANCED_FACE ( 'NONE', ( #1950 ), #32961, .F. ) ;
#25415 = DIRECTION ( 'NONE',  ( -3.469446951953613696E-16, 0.000000000000000000, -1.000000000000000000 ) ) ;
#25416 = ORIENTED_EDGE ( 'NONE', *, *, #6195, .F. ) ;
#25417 = FACE_BOUND ( 'NONE', #35697, .T. ) ;
#25418 = ORIENTED_EDGE ( 'NONE', *, *, #34783, .T. ) ;
#25419 = DIRECTION ( 'NONE',  ( 1.734723475976806848E-16, -0.000000000000000000, 1.000000000000000000 ) ) ;
#25420 = EDGE_LOOP ( 'NONE', ( #20318, #39884, #43926, #44303, #39788 ) ) ;
#25422 = ORIENTED_EDGE ( 'NONE', *, *, #19402, .T. ) ;
#25421 = VECTOR ( 'NONE', #16215, 39.37007874015748143 ) ;
#25423 = CARTESIAN_POINT ( 'NONE',  ( 0.9794755770252102645, 0.5905511811023621549, -1.097585813245683717 ) ) ;
#25424 = DIRECTION ( 'NONE',  ( 0.000000000000000000, 0.000000000000000000, -1.000000000000000000 ) ) ;
#25425 = EDGE_CURVE ( 'NONE', #32340, #18300, #21067, .T. ) ;
#25426 = VECTOR ( 'NONE', #26100, 39.37007874015748143 ) ;
#25427 = EDGE_CURVE ( 'NONE', #15952, #8046, #31106, .T. ) ;
#25428 = ORIENTED_EDGE ( 'NONE', *, *, #39312, .T. ) ;
#25429 = PLANE ( 'NONE',  #7954 ) ;
#25431 = DIRECTION ( 'NONE',  ( 0.9485564197619719140, 0.000000000000000000, -0.3166081466550567658 ) ) ;
#25430 = AXIS2_PLACEMENT_3D ( 'NONE', #34269, #4036, #11273 ) ;
#25432 = ORIENTED_EDGE ( 'NONE', *, *, #5325, .T. ) ;
#25433 = ADVANCED_FACE ( 'NONE', ( #41204 ), #17703, .F. ) ;
#25435 = LINE ( 'NONE', #40938, #32068 ) ;
#25434 = AXIS2_PLACEMENT_3D ( 'NONE', #4561, #36574, #47884 ) ;
#25436 = DIRECTION ( 'NONE',  ( -0.000000000000000000, 1.000000000000000000, -0.000000000000000000 ) ) ;
#25437 = DIRECTION ( 'NONE',  ( -0.000000000000000000, 1.000000000000000000, -0.000000000000000000 ) ) ;
#25438 = ADVANCED_FACE ( 'NONE', ( #14080 ), #9956, .F. ) ;
#25439 = CARTESIAN_POINT ( 'NONE',  ( 1.560669927219590525, 3.346456692913386100, 0.5905511811023579360 ) ) ;
#25440 = DIRECTION ( 'NONE',  ( 0.000000000000000000, 0.000000000000000000, 1.000000000000000000 ) ) ;
#25441 = CARTESIAN_POINT ( 'NONE',  ( 0.08139965876239094178, 1.610780518492231694, 0.000000000000000000 ) ) ;
#25442 = EDGE_LOOP ( 'NONE', ( #11111, #31723, #3842, #26550 ) ) ;
#25443 = DIRECTION ( 'NONE',  ( -0.9998717552508121775, -0.01601477604151182316, 0.000000000000000000 ) ) ;
#25444 = LINE ( 'NONE', #41208, #42977 ) ;
#25445 = EDGE_CURVE ( 'NONE', #49614, #7280, #6073, .T. ) ;
#25446 = ORIENTED_EDGE ( 'NONE', *, *, #22840, .T. ) ;
#25447 = CYLINDRICAL_SURFACE ( 'NONE', #43808, 2.165354330708661568 ) ;
#25448 = CARTESIAN_POINT ( 'NONE',  ( -0.3500732549360408563, 1.603869690133923331, 2.204675616574417685 ) ) ;
#25449 = VERTEX_POINT ( 'NONE', #24936 ) ;
#25450 = DIRECTION ( 'NONE',  ( -0.000000000000000000, 1.000000000000000000, -0.000000000000000000 ) ) ;
#25451 = VECTOR ( 'NONE', #27486, 39.37007874015748143 ) ;
#25452 = B_SPLINE_CURVE_WITH_KNOTS ( 'NONE', 3,
 ( #6018, #25640, #5769, #40384 ),
 .UNSPECIFIED., .F., .F.,
 ( 4, 4 ),
 ( 0.01233407828749484916, 0.03073846733299314196 ),
 .UNSPECIFIED. ) ;
#25453 = EDGE_CURVE ( 'NONE', #10658, #20943, #22088, .T. ) ;
#25454 = CARTESIAN_POINT ( 'NONE',  ( -0.5455278134075208785, 3.346456692913386100, 0.7480314960629874665 ) ) ;
#25455 = EDGE_CURVE ( 'NONE', #37535, #2752, #14332, .T. ) ;
#25456 = DIRECTION ( 'NONE',  ( -3.469446951953613696E-16, 0.000000000000000000, -1.000000000000000000 ) ) ;
#25457 = VERTEX_POINT ( 'NONE', #45798 ) ;
#25458 = LINE ( 'NONE', #1970, #8446 ) ;
#25459 = EDGE_LOOP ( 'NONE', ( #29211, #29045, #33755, #10061, #41024 ) ) ;
#25460 = FACE_BOUND ( 'NONE', #44379, .T. ) ;
#25461 = DIRECTION ( 'NONE',  ( -0.000000000000000000, 1.000000000000000000, -0.000000000000000000 ) ) ;
#25462 = CONICAL_SURFACE ( 'NONE', #21345, 1.850107469027523210, 0.6386652850508578450 ) ;
#25463 = FACE_OUTER_BOUND ( 'NONE', #44646, .T. ) ;
#25464 = DIRECTION ( 'NONE',  ( -0.8090169943749507819, 1.288287287306305530E-16, 0.5877852522924685852 ) ) ;
#25465 = VECTOR ( 'NONE', #32563, 39.37007874015748143 ) ;
#25466 = ORIENTED_EDGE ( 'NONE', *, *, #16668, .T. ) ;
#25467 = EDGE_LOOP ( 'NONE', ( #20094, #32491, #11810, #49686 ) ) ;
#25468 = CARTESIAN_POINT ( 'NONE',  ( -1.985260859929297572, 3.267716535433071279, 0.3149606299212578953 ) ) ;
#25469 = ORIENTED_EDGE ( 'NONE', *, *, #28855, .T. ) ;
#25470 = VECTOR ( 'NONE', #14600, 39.37007874015748143 ) ;
#25471 = PLANE ( 'NONE',  #48275 ) ;
#25472 = ORIENTED_EDGE ( 'NONE', *, *, #17774, .F. ) ;
#25473 = CARTESIAN_POINT ( 'NONE',  ( -1.363819533518803029, 0.000000000000000000, 1.220472440944875281 ) ) ;
#25474 = ORIENTED_EDGE ( 'NONE', *, *, #42467, .T. ) ;
#25475 = LINE ( 'NONE', #10242, #45521 ) ;
#25476 = EDGE_CURVE ( 'NONE', #344, #33287, #2827, .T. ) ;
#25477 = CARTESIAN_POINT ( 'NONE',  ( -0.7855418668307150298, 5.905511811023623991, -2.846347029613745416 ) ) ;
#25478 = VERTEX_POINT ( 'NONE', #1441 ) ;
#25479 = CARTESIAN_POINT ( 'NONE',  ( 0.1968503937007877735, 3.267716535433071279, 1.692913385826762873 ) ) ;
#25480 = ORIENTED_EDGE ( 'NONE', *, *, #23448, .F. ) ;
#25481 = EDGE_LOOP ( 'NONE', ( #29201, #32576, #46662, #27498, #40854, #1295, #32337, #37554, #5070, #24559, #3284 ) ) ;
#25482 = ADVANCED_FACE ( 'NONE', ( #29316 ), #40688, .F. ) ;
#25483 = EDGE_CURVE ( 'NONE', #48933, #47342, #18961, .T. ) ;
#25484 = AXIS2_PLACEMENT_3D ( 'NONE', #6303, #18174, #33930 ) ;
#25485 = ADVANCED_FACE ( 'NONE', ( #34968 ), #23333, .F. ) ;
#25486 = ORIENTED_EDGE ( 'NONE', *, *, #21494, .F. ) ;
#25487 = EDGE_LOOP ( 'NONE', ( #34305, #29854, #21689, #14135 ) ) ;
#25488 = DIRECTION ( 'NONE',  ( -0.000000000000000000, 1.000000000000000000, -0.000000000000000000 ) ) ;
#25489 = EDGE_CURVE ( 'NONE', #35180, #14599, #50648, .T. ) ;
#25490 = EDGE_LOOP ( 'NONE', ( #25193, #9873, #19344, #17979 ) ) ;
#25491 = PLANE ( 'NONE',  #33713 ) ;
#25492 = PLANE ( 'NONE',  #12042 ) ;
#25493 = VECTOR ( 'NONE', #42190, 39.37007874015748143 ) ;
#25494 = DIRECTION ( 'NONE',  ( -1.000000000000000000, 0.000000000000000000, 1.734723475976806848E-16 ) ) ;
#25495 = VECTOR ( 'NONE', #2486, 39.37007874015748143 ) ;
#25496 = ORIENTED_EDGE ( 'NONE', *, *, #32989, .F. ) ;
#25497 = DIRECTION ( 'NONE',  ( 0.000000000000000000, 0.000000000000000000, 1.000000000000000000 ) ) ;
#25498 = CARTESIAN_POINT ( 'NONE',  ( 2.559055118110236560, 0.000000000000000000, -4.133858267716535195 ) ) ;
#25499 = VERTEX_POINT ( 'NONE', #22842 ) ;
#25500 = DIRECTION ( 'NONE',  ( -3.469446951953613696E-16, 0.000000000000000000, -1.000000000000000000 ) ) ;
#25501 = LINE ( 'NONE', #45862, #26676 ) ;
#25502 = ADVANCED_FACE ( 'NONE', ( #2969 ), #22339, .F. ) ;
#25503 = CIRCLE ( 'NONE', #28002, 2.106299212598425008 ) ;
#25504 = DIRECTION ( 'NONE',  ( -0.01601477604151182663, 0.9998717552508123996, -0.000000000000000000 ) ) ;
#25505 = CARTESIAN_POINT ( 'NONE',  ( -1.930190994932097004, 6.692913385826772199, -0.9827944786818715306 ) ) ;
#25506 = B_SPLINE_CURVE_WITH_KNOTS ( 'NONE', 3,
 ( #13628, #41001, #37130, #1492 ),
 .UNSPECIFIED., .F., .F.,
 ( 4, 4 ),
 ( 0.01079281432884818606, 0.03073583335247125417 ),
 .UNSPECIFIED. ) ;
#25507 = EDGE_CURVE ( 'NONE', #48833, #42740, #26208, .T. ) ;
#25508 = CARTESIAN_POINT ( 'NONE',  ( 0.1968503937007878568, 3.346456692913386100, 0.9448818897637749625 ) ) ;
#25509 = PLANE ( 'NONE',  #11267 ) ;
#25510 = ORIENTED_EDGE ( 'NONE', *, *, #38839, .F. ) ;
#25511 = PLANE ( 'NONE',  #45200 ) ;
#25512 = DIRECTION ( 'NONE',  ( 2.866708903754326305E-17, 1.000000000000000000, 1.255987235303924321E-16 ) ) ;
#25513 = EDGE_CURVE ( 'NONE', #5893, #21285, #10717, .T. ) ;
#25514 = ORIENTED_EDGE ( 'NONE', *, *, #38170, .T. ) ;
#25515 = DIRECTION ( 'NONE',  ( -1.000000000000000000, 0.000000000000000000, 0.000000000000000000 ) ) ;
#25516 = ADVANCED_FACE ( 'NONE', ( #42199 ), #7597, .F. ) ;
#25517 = ADVANCED_FACE ( 'NONE', ( #15346 ), #39343, .T. ) ;
#25518 = ORIENTED_EDGE ( 'NONE', *, *, #23687, .T. ) ;
#25519 = DIRECTION ( 'NONE',  ( -0.000000000000000000, 1.000000000000000000, -0.000000000000000000 ) ) ;
#25520 = CARTESIAN_POINT ( 'NONE',  ( -0.7331725592709618100, 1.597733653658881758, 2.093588567519426569 ) ) ;
#25521 = CARTESIAN_POINT ( 'NONE',  ( -0.6982598466389058345, 0.000000000000000000, 1.720449438420079691 ) ) ;
#25522 = PLANE ( 'NONE',  #27552 ) ;
#25523 = LINE ( 'NONE', #758, #43353 ) ;
#25524 = AXIS2_PLACEMENT_3D ( 'NONE', #23747, #38987, #3622 ) ;
#25525 = ORIENTED_EDGE ( 'NONE', *, *, #31347, .F. ) ;
#25526 = LINE ( 'NONE', #17783, #49550 ) ;
#25527 = ORIENTED_EDGE ( 'NONE', *, *, #4473, .T. ) ;
#25528 = CARTESIAN_POINT ( 'NONE',  ( 1.363819533518803029, 3.346456692913386100, -1.299212598425193210 ) ) ;
#25529 = EDGE_LOOP ( 'NONE', ( #18920, #24032, #47879, #47213 ) ) ;
#25530 = DIRECTION ( 'NONE',  ( 1.000000000000000000, 0.000000000000000000, 0.000000000000000000 ) ) ;
#25531 = CARTESIAN_POINT ( 'NONE',  ( -0.3486774197067339376, 3.346456692913386100, 0.3149606299212577287 ) ) ;
#25532 = ORIENTED_EDGE ( 'NONE', *, *, #28940, .T. ) ;
#25533 = AXIS2_PLACEMENT_3D ( 'NONE', #41318, #37711, #18078 ) ;
#25534 = LINE ( 'NONE', #20899, #42878 ) ;
#25535 = LINE ( 'NONE', #17537, #47935 ) ;
#25536 = LINE ( 'NONE', #26549, #37921 ) ;
#25537 = VERTEX_POINT ( 'NONE', #30591 ) ;
#25538 = VERTEX_POINT ( 'NONE', #19208 ) ;
#25539 = DIRECTION ( 'NONE',  ( -0.9989930665413151445, 0.000000000000000000, 0.04486483035050446017 ) ) ;
#25540 = FACE_BOUND ( 'NONE', #5581, .T. ) ;
#25541 = ORIENTED_EDGE ( 'NONE', *, *, #47475, .F. ) ;
#25542 = AXIS2_PLACEMENT_3D ( 'NONE', #29723, #22738, #38492 ) ;
#25543 = B_SPLINE_CURVE_WITH_KNOTS ( 'NONE', 3,
 ( #7354, #19459, #3476, #46310 ),
 .UNSPECIFIED., .F., .F.,
 ( 4, 4 ),
 ( 2.002015897020957629E-07, 0.02001440658365299941 ),
 .UNSPECIFIED. ) ;
#25544 = DIRECTION ( 'NONE',  ( -0.000000000000000000, 0.000000000000000000, 1.000000000000000000 ) ) ;
#25545 = CARTESIAN_POINT ( 'NONE',  ( 0.5284761224300885685, 1.574803149606302854, -2.099874368989729234 ) ) ;
#25546 = ADVANCED_FACE ( 'NONE', ( #26704 ), #45923, .T. ) ;
#25547 = ORIENTED_EDGE ( 'NONE', *, *, #45074, .T. ) ;
#25548 = ORIENTED_EDGE ( 'NONE', *, *, #45976, .T. ) ;
#25549 = CARTESIAN_POINT ( 'NONE',  ( 3.927031490892378253E-16, 3.346456692913386100, 0.7480314960629874665 ) ) ;
#25550 = EDGE_CURVE ( 'NONE', #40703, #6865, #49903, .T. ) ;
#25551 = EDGE_CURVE ( 'NONE', #43566, #46444, #15598, .T. ) ;
#25552 = CARTESIAN_POINT ( 'NONE',  ( -1.439733046521776139, 3.346456692913386100, 0.6299212598425164567 ) ) ;
#25553 = VERTEX_POINT ( 'NONE', #15093 ) ;
#25554 = ORIENTED_EDGE ( 'NONE', *, *, #48210, .T. ) ;
#25555 = ORIENTED_EDGE ( 'NONE', *, *, #50051, .T. ) ;
#25556 = DIRECTION ( 'NONE',  ( -3.469446951953613696E-16, 0.000000000000000000, -1.000000000000000000 ) ) ;
#25557 = CARTESIAN_POINT ( 'NONE',  ( -0.8182917201112819283, 3.346456692913386100, 2.047244094488179567 ) ) ;
#25558 = VECTOR ( 'NONE', #17172, 39.37007874015748143 ) ;
#25559 = DIRECTION ( 'NONE',  ( 0.000000000000000000, 0.000000000000000000, -1.000000000000000000 ) ) ;
#25560 = DIRECTION ( 'NONE',  ( 1.160706738777443955E-16, 1.000000000000000000, -5.589669052740684758E-17 ) ) ;
#25561 = EDGE_LOOP ( 'NONE', ( #21288, #16697, #46067, #9835 ) ) ;
#25562 = EDGE_LOOP ( 'NONE', ( #15820, #14672, #33828, #29135 ) ) ;
#25563 = CARTESIAN_POINT ( 'NONE',  ( 1.909347346926324684, 3.267716535433071279, -3.312189666507128175E-16 ) ) ;
#25564 = DIRECTION ( 'NONE',  ( -1.000000000000000000, -0.000000000000000000, -0.000000000000000000 ) ) ;
#25565 = LINE ( 'NONE', #21699, #9325 ) ;
#25566 = ADVANCED_FACE ( 'NONE', ( #26954 ), #31952, .T. ) ;
#25567 = DIRECTION ( 'NONE',  ( -0.9909497617679352555, 0.000000000000000000, 0.1342332658176522697 ) ) ;
#25568 = CARTESIAN_POINT ( 'NONE',  ( -0.8239235538337883469, 1.661896910481805767, 2.055279188836330206 ) ) ;
#25569 = VECTOR ( 'NONE', #29111, 39.37007874015748854 ) ;
#25570 = EDGE_CURVE ( 'NONE', #40954, #32558, #31096, .T. ) ;
#25571 = VECTOR ( 'NONE', #9365, 39.37007874015748143 ) ;
#25572 = CARTESIAN_POINT ( 'NONE',  ( -0.6214413264104939882, 0.000000000000000000, 0.4724409448818872592 ) ) ;
#25573 = CARTESIAN_POINT ( 'NONE',  ( -0.6214413264104945434, 3.346456692913386100, -0.03937007874015895081 ) ) ;
#25574 = VERTEX_POINT ( 'NONE', #19456 ) ;
#25575 = CARTESIAN_POINT ( 'NONE',  ( 1.550261229843175492, 1.634307024739966696, 1.699618603577774945 ) ) ;
#25576 = CYLINDRICAL_SURFACE ( 'NONE', #17831, 2.165354330708661568 ) ;
#25577 = ADVANCED_FACE ( 'NONE', ( #46057 ), #29474, .T. ) ;
#25578 = AXIS2_PLACEMENT_3D ( 'NONE', #43555, #12071, #31960 ) ;
#25579 = ADVANCED_FACE ( 'NONE', ( #46307 ), #34469, .F. ) ;
#25580 = ORIENTED_EDGE ( 'NONE', *, *, #49401, .F. ) ;
#25581 = EDGE_LOOP ( 'NONE', ( #42050, #49564, #12325, #13977, #505, #25416, #39099, #36652, #24323, #31756, #3096, #13259, #35571 ) ) ;
#25582 = CARTESIAN_POINT ( 'NONE',  ( 0.2727639067037604392, 3.346456692913386100, -0.03937007874015908959 ) ) ;
#25583 = CARTESIAN_POINT ( 'NONE',  ( 0.9992734692680932396, 3.240154784483734396, -2.244094488188969283 ) ) ;
#25584 = VERTEX_POINT ( 'NONE', #42945 ) ;
#25585 = B_SPLINE_CURVE_WITH_KNOTS ( 'NONE', 3,
 ( #22653, #3542, #161, #38408 ),
 .UNSPECIFIED., .F., .F.,
 ( 4, 4 ),
 ( 2.396442746870937374E-07, 0.01967631564410392969 ),
 .UNSPECIFIED. ) ;
#25586 = ORIENTED_EDGE ( 'NONE', *, *, #25807, .T. ) ;
#25587 = CARTESIAN_POINT ( 'NONE',  ( -0.1450362469327505233, 5.905511811023623991, -2.160491579385213523 ) ) ;
#25588 = ORIENTED_EDGE ( 'NONE', *, *, #958, .F. ) ;
#25589 = FACE_OUTER_BOUND ( 'NONE', #33306, .T. ) ;
#25590 = CARTESIAN_POINT ( 'NONE',  ( -2.182111253630085290, 0.000000000000000000, -0.3149606299212589500 ) ) ;
#25591 = ORIENTED_EDGE ( 'NONE', *, *, #20509, .F. ) ;
#25592 = ORIENTED_EDGE ( 'NONE', *, *, #7475, .T. ) ;
#25593 = B_SPLINE_CURVE_WITH_KNOTS ( 'NONE', 3,
 ( #28894, #36915, #44629, #1539 ),
 .UNSPECIFIED., .F., .F.,
 ( 4, 4 ),
 ( 0.01084969948538288577, 0.03073585646796594267 ),
 .UNSPECIFIED. ) ;
#25594 = PLANE ( 'NONE',  #13993 ) ;
#25595 = ORIENTED_EDGE ( 'NONE', *, *, #31717, .F. ) ;
#25596 = EDGE_LOOP ( 'NONE', ( #21755, #21631, #6359, #6223, #35651, #48525, #27791, #9284, #23432, #3823, #1838, #1237, #14315, #8961, #6463, #32186, #50409, #27800, #45774, #9995, #45065, #10042, #24564, #46535, #3590, #34336, #12489, #26763, #37563, #19730, #17725, #5297, #47591, #9102, #17425, #32290, #42036, #38261, #4208, #33092, #38779, #38120, #8793, #30539, #9817, #3747, #1168, #29637, #43228, #38766, #36827, #33194, #38895, #25660, #20156 ) ) ;
#25597 = CARTESIAN_POINT ( 'NONE',  ( 0.5455278134075212115, 3.346456692913386100, -0.3149606299212593941 ) ) ;
#25598 = CYLINDRICAL_SURFACE ( 'NONE', #26812, 2.165354330708661568 ) ;
#25599 = CARTESIAN_POINT ( 'NONE',  ( 1.560669927219590303, 3.346456692913386100, -1.501022570047217508 ) ) ;
#25600 = B_SPLINE_CURVE_WITH_KNOTS ( 'NONE', 3,
 ( #5328, #40701, #48649, #2226 ),
 .UNSPECIFIED., .F., .F.,
 ( 4, 4 ),
 ( 0.001741610281575217993, 0.004241651184184463616 ),
 .UNSPECIFIED. ) ;
#25601 = VECTOR ( 'NONE', #31791, 39.37007874015748143 ) ;
#25602 = ORIENTED_EDGE ( 'NONE', *, *, #48491, .F. ) ;
#25603 = VECTOR ( 'NONE', #39054, 39.37007874015748143 ) ;
#25604 = DIRECTION ( 'NONE',  ( -1.000000000000000000, 0.000000000000000000, 1.734723475976806848E-16 ) ) ;
#25605 = CARTESIAN_POINT ( 'NONE',  ( 1.091055626815042423, 3.346456692913386100, -1.889763779527552368 ) ) ;
#25606 = FACE_OUTER_BOUND ( 'NONE', #15090, .T. ) ;
#25607 = ORIENTED_EDGE ( 'NONE', *, *, #21965, .T. ) ;
#25608 = DIRECTION ( 'NONE',  ( 0.000000000000000000, 0.000000000000000000, -1.000000000000000000 ) ) ;
#25609 = CARTESIAN_POINT ( 'NONE',  ( -1.979793062125318803, 5.905511811023623991, 2.191257344206540392 ) ) ;
#25610 = EDGE_CURVE ( 'NONE', #10846, #10682, #10462, .T. ) ;
#25611 = EDGE_CURVE ( 'NONE', #46032, #33703, #19450, .T. ) ;
#25612 = DIRECTION ( 'NONE',  ( -0.000000000000000000, 0.000000000000000000, 1.000000000000000000 ) ) ;
#25613 = ORIENTED_EDGE ( 'NONE', *, *, #17299, .T. ) ;
#25614 = ORIENTED_EDGE ( 'NONE', *, *, #38003, .F. ) ;
#25615 = AXIS2_PLACEMENT_3D ( 'NONE', #5856, #18495, #49936 ) ;
#25616 = ADVANCED_FACE ( 'NONE', ( #32375 ), #35986, .F. ) ;
#25617 = EDGE_CURVE ( 'NONE', #31288, #49909, #23590, .T. ) ;
#25618 = LINE ( 'NONE', #50081, #19803 ) ;
#25619 = CARTESIAN_POINT ( 'NONE',  ( -1.883550378546958060, 1.205361022782829114E-17, -1.069467267250448161 ) ) ;
#25620 = EDGE_CURVE ( 'NONE', #12778, #11040, #17828, .T. ) ;
#25621 = CARTESIAN_POINT ( 'NONE',  ( -0.2646829987305902021, 0.000000000000000000, -2.940868978332400463 ) ) ;
#25622 = EDGE_LOOP ( 'NONE', ( #9628, #40829, #37915, #40633 ) ) ;
#25623 = EDGE_LOOP ( 'NONE', ( #14781, #51001, #19939, #44142 ) ) ;
#25624 = DIRECTION ( 'NONE',  ( -3.469446951953613696E-16, 0.000000000000000000, -1.000000000000000000 ) ) ;
#25625 = ORIENTED_EDGE ( 'NONE', *, *, #19498, .F. ) ;
#25626 = DIRECTION ( 'NONE',  ( 1.734723475976806848E-16, -0.000000000000000000, 1.000000000000000000 ) ) ;
#25627 = CARTESIAN_POINT ( 'NONE',  ( -1.461782879395278734, 6.692913385826772199, -1.598346982901828861 ) ) ;
#25628 = B_SPLINE_CURVE_WITH_KNOTS ( 'NONE', 3,
 ( #5288, #21042, #5545, #33693 ),
 .UNSPECIFIED., .F., .F.,
 ( 4, 4 ),
 ( 2.032896354352839205E-07, 0.002500497150405497481 ),
 .UNSPECIFIED. ) ;
#25629 = EDGE_CURVE ( 'NONE', #42940, #28023, #43964, .T. ) ;
#25630 = FACE_OUTER_BOUND ( 'NONE', #36257, .T. ) ;
#25631 = CARTESIAN_POINT ( 'NONE',  ( -0.8182917201112814842, 0.000000000000000000, 0.7874015748031456541 ) ) ;
#25632 = DIRECTION ( 'NONE',  ( 1.734723475976806848E-16, -0.000000000000000000, 1.000000000000000000 ) ) ;
#25633 = ORIENTED_EDGE ( 'NONE', *, *, #21992, .T. ) ;
#25634 = PLANE ( 'NONE',  #27485 ) ;
#25635 = DIRECTION ( 'NONE',  ( -0.000000000000000000, 0.000000000000000000, 1.000000000000000000 ) ) ;
#25636 = EDGE_CURVE ( 'NONE', #18328, #37024, #7849, .T. ) ;
#25637 = CARTESIAN_POINT ( 'NONE',  ( 0.000000000000000000, 3.267716535433071279, -0.03937007874015895081 ) ) ;
#25638 = CIRCLE ( 'NONE', #3373, 2.165354330708661568 ) ;
#25639 = ORIENTED_EDGE ( 'NONE', *, *, #34360, .T. ) ;
#25640 = CARTESIAN_POINT ( 'NONE',  ( -0.4894113334356742229, 1.605499969913384728, 2.421265748518004468 ) ) ;
#25641 = AXIS2_PLACEMENT_3D ( 'NONE', #24332, #28955, #33367 ) ;
#25642 = FACE_OUTER_BOUND ( 'NONE', #44374, .T. ) ;
#25643 = DIRECTION ( 'NONE',  ( 0.000000000000000000, 1.000000000000000000, 0.000000000000000000 ) ) ;
#25644 = EDGE_LOOP ( 'NONE', ( #9097, #23172, #18882, #28691 ) ) ;
#25645 = CARTESIAN_POINT ( 'NONE',  ( 1.560669927219590747, 3.346456692913386100, 0.4724409448818871482 ) ) ;
#25646 = CARTESIAN_POINT ( 'NONE',  ( -1.467375622110394184, 1.037978273280383279, -2.103394750075909148 ) ) ;
#25647 = ORIENTED_EDGE ( 'NONE', *, *, #29630, .F. ) ;
#25648 = CARTESIAN_POINT ( 'NONE',  ( -1.083598637574820334, 1.538470290252458739, 2.747180975113330259 ) ) ;
#25649 = AXIS2_PLACEMENT_3D ( 'NONE', #45077, #9738, #25732 ) ;
#25650 = LINE ( 'NONE', #41402, #29076 ) ;
#25651 = ORIENTED_EDGE ( 'NONE', *, *, #26403, .T. ) ;
#25652 = FACE_OUTER_BOUND ( 'NONE', #36464, .T. ) ;
#25653 = EDGE_CURVE ( 'NONE', #33862, #10859, #19712, .T. ) ;
#25654 = VECTOR ( 'NONE', #50713, 39.37007874015748143 ) ;
#25655 = DIRECTION ( 'NONE',  ( -0.000000000000000000, 0.000000000000000000, 1.000000000000000000 ) ) ;
#25656 = PLANE ( 'NONE',  #38705 ) ;
#25657 = DIRECTION ( 'NONE',  ( -0.000000000000000000, 1.000000000000000000, -0.000000000000000000 ) ) ;
#25658 = FACE_OUTER_BOUND ( 'NONE', #39246, .T. ) ;
#25659 = VERTEX_POINT ( 'NONE', #40377 ) ;
#25660 = ORIENTED_EDGE ( 'NONE', *, *, #21532, .T. ) ;
#25661 = DIRECTION ( 'NONE',  ( -0.000000000000000000, 1.000000000000000000, -0.000000000000000000 ) ) ;
#25662 = LINE ( 'NONE', #41170, #44418 ) ;
#25663 = ORIENTED_EDGE ( 'NONE', *, *, #49599, .F. ) ;
#25664 = PLANE ( 'NONE',  #19295 ) ;
#25665 = LINE ( 'NONE', #2434, #17836 ) ;
#25666 = CARTESIAN_POINT ( 'NONE',  ( 2.318785432985194905, 1.656916041303249987, 1.828187805987539827 ) ) ;
#25667 = ORIENTED_EDGE ( 'NONE', *, *, #41807, .F. ) ;
#25668 = EDGE_LOOP ( 'NONE', ( #23499, #2928, #51049, #8648 ) ) ;
#25669 = LINE ( 'NONE', #14565, #1580 ) ;
#25670 = CARTESIAN_POINT ( 'NONE',  ( -2.532674450597738769, 1.050099741429788791, 0.2934120129488018702 ) ) ;
#25671 = DIRECTION ( 'NONE',  ( -1.000000000000000000, 0.000000000000000000, -0.000000000000000000 ) ) ;
#25672 = ORIENTED_EDGE ( 'NONE', *, *, #21913, .T. ) ;
#25673 = CARTESIAN_POINT ( 'NONE',  ( 0.000000000000000000, 3.267716535433071279, 0.6299212598425161236 ) ) ;
#25674 = DIRECTION ( 'NONE',  ( 0.01601477604151182663, -0.9998717552508123996, 0.000000000000000000 ) ) ;
#25675 = VERTEX_POINT ( 'NONE', #28221 ) ;
#25676 = ADVANCED_FACE ( 'NONE', ( #39341 ), #12745, .F. ) ;
#25677 = CARTESIAN_POINT ( 'NONE',  ( 0.9836083787002611878, 1.574803149606302854, -1.929060376159698720 ) ) ;
#25678 = VERTEX_POINT ( 'NONE', #24363 ) ;
#25679 = ORIENTED_EDGE ( 'NONE', *, *, #36863, .T. ) ;
#25680 = FACE_OUTER_BOUND ( 'NONE', #19304, .T. ) ;
#25681 = FACE_OUTER_BOUND ( 'NONE', #38476, .T. ) ;
#25682 = ADVANCED_FACE ( 'NONE', ( #8102 ), #40114, .F. ) ;
#25683 = VECTOR ( 'NONE', #34474, 39.37007874015748143 ) ;
#25684 = ADVANCED_FACE ( 'NONE', ( #36498 ), #47297, .F. ) ;
#25685 = ORIENTED_EDGE ( 'NONE', *, *, #35215, .T. ) ;
#25686 = DIRECTION ( 'NONE',  ( 0.000000000000000000, 1.000000000000000000, 0.000000000000000000 ) ) ;
#25687 = EDGE_CURVE ( 'NONE', #19566, #27803, #36245, .T. ) ;
#25688 = CARTESIAN_POINT ( 'NONE',  ( 1.287906020515829919, 3.267716535433071279, -1.740706023381844547 ) ) ;
#25689 = ORIENTED_EDGE ( 'NONE', *, *, #26254, .T. ) ;
#25690 = CIRCLE ( 'NONE', #12526, 2.106299212598425008 ) ;
#25691 = VECTOR ( 'NONE', #5030, 39.37007874015748143 ) ;
#25692 = DIRECTION ( 'NONE',  ( -1.000000000000000000, 0.000000000000000000, -0.000000000000000000 ) ) ;
#25693 = CARTESIAN_POINT ( 'NONE',  ( -1.439733046521776583, 3.267716535433071279, -0.3149606299212592275 ) ) ;
#25694 = VECTOR ( 'NONE', #17139, 39.37007874015748143 ) ;
#25695 = EDGE_CURVE ( 'NONE', #5907, #36731, #49109, .T. ) ;
#25696 = CARTESIAN_POINT ( 'NONE',  ( 2.179222933086670366, 2.755905511811027164, 2.848360286204475234 ) ) ;
#25697 = LINE ( 'NONE', #40946, #22880 ) ;
#25698 = CARTESIAN_POINT ( 'NONE',  ( -2.100227814008681637, 1.588094595312779855, -2.076109931251943763 ) ) ;
#25699 = VERTEX_POINT ( 'NONE', #11974 ) ;
#25700 = CARTESIAN_POINT ( 'NONE',  ( 2.106197740627111958, 3.267716535433071279, -7.307341331430321661E-16 ) ) ;
#25701 = EDGE_CURVE ( 'NONE', #46139, #39964, #4995, .T. ) ;
#25702 = LINE ( 'NONE', #1702, #33951 ) ;
#25703 = ORIENTED_EDGE ( 'NONE', *, *, #48688, .T. ) ;
#25704 = CARTESIAN_POINT ( 'NONE',  ( 0.000000000000000000, 3.267716535433071279, -0.6299212598425177889 ) ) ;
#25705 = LINE ( 'NONE', #21842, #22801 ) ;
#25706 = EDGE_LOOP ( 'NONE', ( #31319, #15374, #11760, #28869 ) ) ;
#25707 = CARTESIAN_POINT ( 'NONE',  ( -0.6924561055946872878, 0.005671908246031987996, 1.704985425709532043 ) ) ;
#25708 = ADVANCED_FACE ( 'NONE', ( #867 ), #27456, .T. ) ;
#25710 = B_SPLINE_CURVE_WITH_KNOTS ( 'NONE', 3,
 ( #6128, #26999, #46598, #42503 ),
 .UNSPECIFIED., .F., .F.,
 ( 4, 4 ),
 ( 0.001106910458727990501, 0.003607175275882030987 ),
 .UNSPECIFIED. ) ;
#25709 = PLANE ( 'NONE',  #42331 ) ;
#25711 = LINE ( 'NONE', #37089, #31799 ) ;
#25712 = ORIENTED_EDGE ( 'NONE', *, *, #10716, .F. ) ;
#25713 = CARTESIAN_POINT ( 'NONE',  ( -1.712496953225537633, 3.346456692913386100, 1.220472440944875059 ) ) ;
#25714 = ORIENTED_EDGE ( 'NONE', *, *, #17227, .F. ) ;
#25715 = CARTESIAN_POINT ( 'NONE',  ( -1.472219874544909768, 1.696317054561777171, 2.560030851058948898 ) ) ;
#25716 = ADVANCED_FACE ( 'NONE', ( #12232 ), #8359, .T. ) ;
#25717 = FACE_OUTER_BOUND ( 'NONE', #31596, .T. ) ;
#25718 = CIRCLE ( 'NONE', #47929, 2.165354330708661568 ) ;
#25719 = AXIS2_PLACEMENT_3D ( 'NONE', #34947, #26934, #46777 ) ;
#25720 = DIRECTION ( 'NONE',  ( 1.000000000000000000, 0.000000000000000000, 0.000000000000000000 ) ) ;
#25721 = DIRECTION ( 'NONE',  ( 1.000000000000000000, 0.000000000000000000, 0.000000000000000000 ) ) ;
#25722 = AXIS2_PLACEMENT_3D ( 'NONE', #38806, #23298, #26668 ) ;
#25723 = ORIENTED_EDGE ( 'NONE', *, *, #5644, .F. ) ;
#25724 = ORIENTED_EDGE ( 'NONE', *, *, #10303, .F. ) ;
#25725 = CARTESIAN_POINT ( 'NONE',  ( 0.5455278134075213226, 3.267716535433071279, -9.463399047163221947E-17 ) ) ;
#25726 = ORIENTED_EDGE ( 'NONE', *, *, #16239, .F. ) ;
#25727 = EDGE_CURVE ( 'NONE', #6760, #33442, #44982, .T. ) ;
#25728 = VECTOR ( 'NONE', #38136, 39.37007874015748143 ) ;
#25729 = DIRECTION ( 'NONE',  ( -1.000000000000000000, 0.000000000000000000, -0.000000000000000000 ) ) ;
#25730 = ORIENTED_EDGE ( 'NONE', *, *, #26702, .F. ) ;
#25731 = EDGE_CURVE ( 'NONE', #40564, #12580, #17891, .T. ) ;
#25732 = DIRECTION ( 'NONE',  ( 1.000000000000000000, 0.000000000000000000, 0.000000000000000000 ) ) ;
#25733 = AXIS2_PLACEMENT_3D ( 'NONE', #28679, #17083, #9326 ) ;
#25734 = EDGE_LOOP ( 'NONE', ( #20450, #20877, #20697, #26250 ) ) ;
#25735 = CARTESIAN_POINT ( 'NONE',  ( 2.052631463899901920, 3.346456692913386100, -0.4724409448818889246 ) ) ;
#25736 = DIRECTION ( 'NONE',  ( 0.9998717552508121775, 0.01601477604151182663, 0.000000000000000000 ) ) ;
#25737 = VERTEX_POINT ( 'NONE', #5761 ) ;
#25738 = CARTESIAN_POINT ( 'NONE',  ( -0.3136974817027969320, 1.205361022782829114E-17, -2.936457595020224520 ) ) ;
#25739 = ORIENTED_EDGE ( 'NONE', *, *, #24103, .T. ) ;
#25740 = EDGE_LOOP ( 'NONE', ( #38230, #8202, #39455, #40483 ) ) ;
#25741 = EDGE_CURVE ( 'NONE', #8210, #40819, #44728, .T. ) ;
#25742 = ORIENTED_EDGE ( 'NONE', *, *, #41438, .T. ) ;
#25743 = VERTEX_POINT ( 'NONE', #2143 ) ;
#25744 = CARTESIAN_POINT ( 'NONE',  ( -0.2493161376872249368, 1.671100300131709737, -2.221122275763622866 ) ) ;
#25745 = EDGE_CURVE ( 'NONE', #27359, #21474, #22023, .T. ) ;
#25746 = VERTEX_POINT ( 'NONE', #6272 ) ;
#25747 = CARTESIAN_POINT ( 'NONE',  ( 1.387332044438934986, 1.697314215445209218, -1.825773270393029168 ) ) ;
#25748 = CARTESIAN_POINT ( 'NONE',  ( 0.7423782071083087075, 3.346456692913386100, -0.3149606299212593941 ) ) ;
#25749 = AXIS2_PLACEMENT_3D ( 'NONE', #2061, #25808, #49506 ) ;
#25750 = CARTESIAN_POINT ( 'NONE',  ( 1.909347346926324462, 0.000000000000000000, -0.9842519685039348154 ) ) ;
#25751 = ORIENTED_EDGE ( 'NONE', *, *, #41818, .F. ) ;
#25752 = AXIS2_PLACEMENT_3D ( 'NONE', #32994, #714, #21104 ) ;
#25753 = DIRECTION ( 'NONE',  ( 1.000000000000000000, -0.000000000000000000, 0.000000000000000000 ) ) ;
#25754 = CARTESIAN_POINT ( 'NONE',  ( 0.7423782071083091516, 3.267716535433071279, 2.034117492951036166 ) ) ;
#25755 = VERTEX_POINT ( 'NONE', #33402 ) ;
#25756 = CARTESIAN_POINT ( 'NONE',  ( 0.04921259842519603439, 6.692913385826772199, 2.164795024401847456 ) ) ;
#25757 = CARTESIAN_POINT ( 'NONE',  ( 1.636583440222563857, 3.346456692913386100, 0.4330708661417290162 ) ) ;
#25758 = CIRCLE ( 'NONE', #29038, 2.165354330708661568 ) ;
#25759 = CARTESIAN_POINT ( 'NONE',  ( -0.04921259842519758176, 5.905511811023623991, 2.213182383082911375 ) ) ;
#25760 = DIRECTION ( 'NONE',  ( -3.986037398843765983E-20, -1.000000000000000000, -1.160734090543304660E-16 ) ) ;
#25761 = VECTOR ( 'NONE', #45753, 39.37007874015748143 ) ;
#25762 = DIRECTION ( 'NONE',  ( -0.000000000000000000, 1.000000000000000000, -0.000000000000000000 ) ) ;
#25763 = CARTESIAN_POINT ( 'NONE',  ( 0.5455278134075212115, 3.346456692913386100, -0.9448818897637765168 ) ) ;
#25764 = VERTEX_POINT ( 'NONE', #45227 ) ;
#25765 = CARTESIAN_POINT ( 'NONE',  ( 0.000000000000000000, 3.267716535433071279, -0.03937007874015908959 ) ) ;
#25766 = EDGE_CURVE ( 'NONE', #36675, #20192, #29510, .T. ) ;
#25767 = PLANE ( 'NONE',  #1184 ) ;
#25768 = ORIENTED_EDGE ( 'NONE', *, *, #14784, .T. ) ;
#25769 = CARTESIAN_POINT ( 'NONE',  ( 0.2727639067037604947, 0.000000000000000000, -1.417322834645664331 ) ) ;
#25770 = ORIENTED_EDGE ( 'NONE', *, *, #14839, .F. ) ;
#25771 = CARTESIAN_POINT ( 'NONE',  ( -2.277873973731453727, 1.585326468414270495, 1.879489153247635214 ) ) ;
#25772 = ADVANCED_FACE ( 'NONE', ( #33650 ), #13765, .F. ) ;
#25773 = FACE_OUTER_BOUND ( 'NONE', #12501, .T. ) ;
#25774 = CARTESIAN_POINT ( 'NONE',  ( 0.8182917201112821504, 3.267716535433071279, -1.419509857074483539E-16 ) ) ;
#25775 = EDGE_CURVE ( 'NONE', #43424, #782, #41591, .T. ) ;
#25776 = DIRECTION ( 'NONE',  ( -1.000000000000000000, 0.000000000000000000, 0.000000000000000000 ) ) ;
#25777 = LINE ( 'NONE', #30162, #2184 ) ;
#25778 = ORIENTED_EDGE ( 'NONE', *, *, #48659, .T. ) ;
#25779 = ADVANCED_FACE ( 'NONE', ( #41384 ), #37776, .F. ) ;
#25780 = CARTESIAN_POINT ( 'NONE',  ( -0.5455278134075208785, 3.346456692913386100, 1.377952755905504256 ) ) ;
#25781 = VERTEX_POINT ( 'NONE', #48827 ) ;
#25782 = EDGE_LOOP ( 'NONE', ( #33495, #4180, #6164, #11034, #44985, #36800, #31492, #15877 ) ) ;
#25783 = CARTESIAN_POINT ( 'NONE',  ( -0.3381173457103602287, 1.574803149606302854, 2.138793126519845877 ) ) ;
#25784 = EDGE_LOOP ( 'NONE', ( #21942, #9475, #14228, #38924 ) ) ;
#25785 = CARTESIAN_POINT ( 'NONE',  ( 0.000000000000000000, 3.267716535433071279, 0.000000000000000000 ) ) ;
#25786 = DIRECTION ( 'NONE',  ( -3.469446951953613696E-16, 0.000000000000000000, -1.000000000000000000 ) ) ;
#25787 = ORIENTED_EDGE ( 'NONE', *, *, #14733, .T. ) ;
#25788 = CARTESIAN_POINT ( 'NONE',  ( -0.8942052331142552601, 3.346456692913386100, 1.889763779527550147 ) ) ;
#25789 = DIRECTION ( 'NONE',  ( -3.469446951953613696E-16, 0.000000000000000000, -1.000000000000000000 ) ) ;
#25790 = EDGE_CURVE ( 'NONE', #24, #29095, #17131, .T. ) ;
#25791 = CIRCLE ( 'NONE', #24983, 2.165354330708661568 ) ;
#25792 = CARTESIAN_POINT ( 'NONE',  ( -1.743516651958532115, 0.0004834999639498430428, -4.958524412099369637E-19 ) ) ;
#25793 = VERTEX_POINT ( 'NONE', #9378 ) ;
#25794 = VERTEX_POINT ( 'NONE', #28986 ) ;
#25796 = DIRECTION ( 'NONE',  ( 1.734723475976806848E-16, -0.000000000000000000, 1.000000000000000000 ) ) ;
#25795 = AXIS2_PLACEMENT_3D ( 'NONE', #8593, #40858, #40602 ) ;
#25797 = FACE_BOUND ( 'NONE', #4666, .T. ) ;
#25798 = VERTEX_POINT ( 'NONE', #17380 ) ;
#25799 = AXIS2_PLACEMENT_3D ( 'NONE', #14260, #45729, #10394 ) ;
#25800 = EDGE_CURVE ( 'NONE', #6620, #25903, #5506, .T. ) ;
#25801 = VECTOR ( 'NONE', #11090, 39.37007874015748854 ) ;
#25802 = CARTESIAN_POINT ( 'NONE',  ( 0.9436074722315215269, 1.690207154491363273, -2.072844574113425153 ) ) ;
#25803 = CARTESIAN_POINT ( 'NONE',  ( -2.623503965249869729, 1.569838463031876685, 1.355882097269834885 ) ) ;
#25804 = VERTEX_POINT ( 'NONE', #21256 ) ;
#25805 = ORIENTED_EDGE ( 'NONE', *, *, #40017, .F. ) ;
#25806 = EDGE_CURVE ( 'NONE', #19022, #49191, #37014, .T. ) ;
#25807 = EDGE_CURVE ( 'NONE', #36899, #11586, #20285, .T. ) ;
#25808 = DIRECTION ( 'NONE',  ( -0.000000000000000000, -1.000000000000000000, -0.000000000000000000 ) ) ;
#25809 = AXIS2_PLACEMENT_3D ( 'NONE', #10467, #33471, #40691 ) ;
#25810 = CARTESIAN_POINT ( 'NONE',  ( -2.076715649576790224, 1.576214352228098470, 0.6230206298219045369 ) ) ;
#25811 = ORIENTED_EDGE ( 'NONE', *, *, #16193, .T. ) ;
#25812 = EDGE_LOOP ( 'NONE', ( #5926, #14638, #1415, #15663 ) ) ;
#25813 = ORIENTED_EDGE ( 'NONE', *, *, #31572, .T. ) ;
#25814 = CARTESIAN_POINT ( 'NONE',  ( -1.602125192864240821, 3.346456692913386100, -1.456692913385822186 ) ) ;
#25815 = DIRECTION ( 'NONE',  ( 1.000000000000000000, -0.000000000000000000, 0.000000000000000000 ) ) ;
#25816 = DIRECTION ( 'NONE',  ( -0.000000000000000000, 1.000000000000000000, -0.000000000000000000 ) ) ;
#25817 = CARTESIAN_POINT ( 'NONE',  ( 0.2727639067037609943, 3.267716535433071279, 0.9055118110236167750 ) ) ;
#25818 = ORIENTED_EDGE ( 'NONE', *, *, #35135, .F. ) ;
#25819 = EDGE_LOOP ( 'NONE', ( #21372, #6741, #49026, #1782 ) ) ;
#25820 = CARTESIAN_POINT ( 'NONE',  ( -2.047277537895663801, 1.675111054312220515, 0.7169459839182066307 ) ) ;
#25821 = CARTESIAN_POINT ( 'NONE',  ( 1.833433833923351353, 3.267716535433071279, -6.361001426713998480E-16 ) ) ;
#25822 = LINE ( 'NONE', #33591, #21715 ) ;
#25823 = CARTESIAN_POINT ( 'NONE',  ( 1.287906020515829919, 3.255645222919215431, -2.083306009933192371 ) ) ;
#25824 = DIRECTION ( 'NONE',  ( 0.5407162030609374836, -0.6444004775717706579, 0.5407162030609373726 ) ) ;
#25825 = DIRECTION ( 'NONE',  ( 1.000000000000000000, 0.000000000000000000, -3.469446951953613696E-16 ) ) ;
#25826 =( BOUNDED_CURVE ( )  B_SPLINE_CURVE ( 3, ( #6608, #37343, #22352, #38107 ),
 .UNSPECIFIED., .F., .F. ) 
 B_SPLINE_CURVE_WITH_KNOTS ( ( 4, 4 ),
 ( 2.995205087924649234, 3.045949865762518360 ),
 .UNSPECIFIED. ) 
 CURVE ( )  GEOMETRIC_REPRESENTATION_ITEM ( )  RATIONAL_B_SPLINE_CURVE ( ( 1.000000000000000000, 0.9997854254717271072, 0.9997854254717271072, 1.000000000000000000 ) ) 
 REPRESENTATION_ITEM ( '' )  );
#25827 = CARTESIAN_POINT ( 'NONE',  ( -0.8942052331142552601, 0.000000000000000000, -1.889763779527552146 ) ) ;
#25828 = CIRCLE ( 'NONE', #2760, 2.165354330708661568 ) ;
#25829 = ORIENTED_EDGE ( 'NONE', *, *, #2335, .T. ) ;
#25830 = DIRECTION ( 'NONE',  ( -0.000000000000000000, -1.000000000000000000, -0.000000000000000000 ) ) ;
#25831 = DIRECTION ( 'NONE',  ( -0.9998717552508122886, -0.01601477604151182316, 0.000000000000000000 ) ) ;
#25832 = VECTOR ( 'NONE', #24888, 39.37007874015748143 ) ;
#25833 = ORIENTED_EDGE ( 'NONE', *, *, #6165, .T. ) ;
#25834 = CIRCLE ( 'NONE', #34065, 2.106299212598425008 ) ;
#25835 = ORIENTED_EDGE ( 'NONE', *, *, #5634, .F. ) ;
#25836 = AXIS2_PLACEMENT_3D ( 'NONE', #38716, #47428, #19327 ) ;
#25837 = CARTESIAN_POINT ( 'NONE',  ( -0.07591351300297359550, 0.000000000000000000, -2.047244094488181343 ) ) ;
#25838 = EDGE_CURVE ( 'NONE', #21355, #24653, #31013, .T. ) ;
#25839 = ORIENTED_EDGE ( 'NONE', *, *, #22621, .F. ) ;
#25840 = EDGE_CURVE ( 'NONE', #1622, #40318, #13004, .T. ) ;
#25841 = ADVANCED_FACE ( 'NONE', ( #20997 ), #33142, .F. ) ;
#25842 = ORIENTED_EDGE ( 'NONE', *, *, #3876, .F. ) ;
#25843 = CARTESIAN_POINT ( 'NONE',  ( 0.000000000000000000, 3.267716535433071279, 0.000000000000000000 ) ) ;
#25844 = VERTEX_POINT ( 'NONE', #37266 ) ;
#25845 = ADVANCED_FACE ( 'NONE', ( #1885 ), #42639, .F. ) ;
#25846 = PLANE ( 'NONE',  #14480 ) ;
#25847 = CARTESIAN_POINT ( 'NONE',  ( -1.636583440222564301, 0.000000000000000000, -0.5118110236220466680 ) ) ;
#25848 = EDGE_LOOP ( 'NONE', ( #37579, #25155, #6523, #44175 ) ) ;
#25849 = VERTEX_POINT ( 'NONE', #3404 ) ;
#25850 = DIRECTION ( 'NONE',  ( 0.000000000000000000, 0.000000000000000000, 1.000000000000000000 ) ) ;
#25851 = VERTEX_POINT ( 'NONE', #7531 ) ;
#25852 = ORIENTED_EDGE ( 'NONE', *, *, #24812, .F. ) ;
#25853 = CARTESIAN_POINT ( 'NONE',  ( -0.2727639067037607723, 0.000000000000000000, -0.7874015748031470974 ) ) ;
#25854 = PLANE ( 'NONE',  #35155 ) ;
#25855 = PLANE ( 'NONE',  #36751 ) ;
#25856 = EDGE_CURVE ( 'NONE', #12446, #10888, #30016, .T. ) ;
#25857 = ORIENTED_EDGE ( 'NONE', *, *, #22581, .T. ) ;
#25858 = EDGE_CURVE ( 'NONE', #17250, #35873, #26083, .T. ) ;
#25859 = FACE_OUTER_BOUND ( 'NONE', #2876, .T. ) ;
#25860 = DIRECTION ( 'NONE',  ( 1.734723475976806848E-16, -0.000000000000000000, 1.000000000000000000 ) ) ;
#25861 = CARTESIAN_POINT ( 'NONE',  ( -1.461363083917493810, 6.692913385826772199, 1.597866488315562439 ) ) ;
#25862 = ORIENTED_EDGE ( 'NONE', *, *, #15299, .F. ) ;
#25863 = B_SPLINE_CURVE_WITH_KNOTS ( 'NONE', 3,
 ( #37823, #33449, #2451, #2193 ),
 .UNSPECIFIED., .F., .F.,
 ( 4, 4 ),
 ( 2.032912791916312219E-07, 0.002500496826745732259 ),
 .UNSPECIFIED. ) ;
#25864 = ADVANCED_FACE ( 'NONE', ( #50095 ), #11151, .F. ) ;
#25865 = DIRECTION ( 'NONE',  ( 0.3930250316539278810, 0.000000000000000000, -0.9195277725514489076 ) ) ;
#25866 = VECTOR ( 'NONE', #42439, 39.37007874015748143 ) ;
#25867 = CARTESIAN_POINT ( 'NONE',  ( 0.08139965876239094178, 1.610780518492231694, 0.000000000000000000 ) ) ;
#25868 = EDGE_CURVE ( 'NONE', #13111, #16270, #41893, .T. ) ;
#25869 = CARTESIAN_POINT ( 'NONE',  ( 0.4696143004045479352, 3.346456692913386100, -0.7874015748031473194 ) ) ;
#25870 = ORIENTED_EDGE ( 'NONE', *, *, #40594, .T. ) ;
#25871 = VECTOR ( 'NONE', #19790, 39.37007874015748143 ) ;
#25872 = ORIENTED_EDGE ( 'NONE', *, *, #48014, .F. ) ;
#25873 = ADVANCED_FACE ( 'NONE', ( #33900 ), #14779, .F. ) ;
#25874 = AXIS2_PLACEMENT_3D ( 'NONE', #42572, #19071, #38954 ) ;
#25875 = VECTOR ( 'NONE', #611, 39.37007874015748143 ) ;
#25876 = LINE ( 'NONE', #6517, #42301 ) ;
#25877 = CARTESIAN_POINT ( 'NONE',  ( -2.695799277629577162, 1.571269479597534824, -1.205759334241492731 ) ) ;
#25878 = CARTESIAN_POINT ( 'NONE',  ( 0.7513820654849657776, 1.719936709731724189, 2.142107623314860376 ) ) ;
#25879 = ORIENTED_EDGE ( 'NONE', *, *, #15489, .F. ) ;
#25880 = VERTEX_POINT ( 'NONE', #6534 ) ;
#25881 = VECTOR ( 'NONE', #38032, 39.37007874015748143 ) ;
#25882 = LINE ( 'NONE', #26385, #18506 ) ;
#25883 = ORIENTED_EDGE ( 'NONE', *, *, #3758, .F. ) ;
#25884 = CARTESIAN_POINT ( 'NONE',  ( -0.7874015748031493178, 0.000000000000000000, -1.968503937007874072 ) ) ;
#25885 = LINE ( 'NONE', #49336, #38299 ) ;
#25886 = CARTESIAN_POINT ( 'NONE',  ( -0.5455278134075208785, 0.000000000000000000, 0.6299212598425164567 ) ) ;
#25887 = DIRECTION ( 'NONE',  ( -0.000000000000000000, 0.000000000000000000, 1.000000000000000000 ) ) ;
#25888 = CARTESIAN_POINT ( 'NONE',  ( 2.793030215715258446, 0.000000000000000000, 0.9592557174602679426 ) ) ;
#25889 = ORIENTED_EDGE ( 'NONE', *, *, #41239, .T. ) ;
#25890 = DIRECTION ( 'NONE',  ( -1.000000000000000000, 0.000000000000000000, -0.000000000000000000 ) ) ;
#25891 = FILL_AREA_STYLE ('',( #10404 ) ) ;
#25892 = DIRECTION ( 'NONE',  ( 0.000000000000000000, 1.000000000000000000, 0.000000000000000000 ) ) ;
#25893 = VERTEX_POINT ( 'NONE', #11405 ) ;
#25894 = DIRECTION ( 'NONE',  ( 0.000000000000000000, 0.000000000000000000, -1.000000000000000000 ) ) ;
#25895 = PLANE ( 'NONE',  #8828 ) ;
#25896 = DIRECTION ( 'NONE',  ( 0.000000000000000000, 0.000000000000000000, 1.000000000000000000 ) ) ;
#25897 = ORIENTED_EDGE ( 'NONE', *, *, #12225, .T. ) ;
#25898 = CARTESIAN_POINT ( 'NONE',  ( -2.437180031585919782, 1.582844051365913662, -1.667735833703134718 ) ) ;
#25899 = AXIS2_PLACEMENT_3D ( 'NONE', #32105, #339, #15825 ) ;
#25900 = ADVANCED_FACE ( 'NONE', ( #22779 ), #7285, .F. ) ;
#25901 = AXIS2_PLACEMENT_3D ( 'NONE', #6202, #19514, #49271 ) ;
#25902 = ADVANCED_FACE ( 'NONE', ( #49587 ), #22275, .F. ) ;
#25903 = VERTEX_POINT ( 'NONE', #2647 ) ;
#25904 = AXIS2_PLACEMENT_3D ( 'NONE', #31423, #1207, #13091 ) ;
#25905 = FACE_OUTER_BOUND ( 'NONE', #42283, .T. ) ;
#25906 = DIRECTION ( 'NONE',  ( -1.000000000000000000, 0.000000000000000000, 1.734723475976806848E-16 ) ) ;
#25907 = ORIENTED_EDGE ( 'NONE', *, *, #25445, .F. ) ;
#25908 = CARTESIAN_POINT ( 'NONE',  ( -1.531154912952794378, 5.905511811023623991, 1.532020527533836329 ) ) ;
#25909 = EDGE_CURVE ( 'NONE', #27651, #30226, #34903, .T. ) ;
#25910 = AXIS2_PLACEMENT_3D ( 'NONE', #13545, #45017, #41172 ) ;
#25911 = AXIS2_PLACEMENT_3D ( 'NONE', #7529, #39024, #3657 ) ;
#25912 = CARTESIAN_POINT ( 'NONE',  ( -1.091055626815042645, 3.346456692913386100, 2.007874015748021268 ) ) ;
#25913 = CARTESIAN_POINT ( 'NONE',  ( 0.8182917201112817063, 0.000000000000000000, -2.047244094488181343 ) ) ;
#25914 = CARTESIAN_POINT ( 'NONE',  ( 1.015142113812069979, 3.267716535433071279, 1.535433070866133898 ) ) ;
#25915 = LINE ( 'NONE', #41408, #43605 ) ;
#25916 = VERTEX_POINT ( 'NONE', #18656 ) ;
#25917 = ORIENTED_EDGE ( 'NONE', *, *, #22195, .T. ) ;
#25918 = LINE ( 'NONE', #48855, #28133 ) ;
#25919 = CIRCLE ( 'NONE', #16028, 2.165354330708661568 ) ;
#25920 = DIRECTION ( 'NONE',  ( -3.469446951953613696E-16, 0.000000000000000000, -1.000000000000000000 ) ) ;
#25921 = ORIENTED_EDGE ( 'NONE', *, *, #19139, .T. ) ;
#25922 = DIRECTION ( 'NONE',  ( -0.000000000000000000, 0.000000000000000000, 1.000000000000000000 ) ) ;
#25923 = CARTESIAN_POINT ( 'NONE',  ( 1.287906020515830141, 3.346456692913386100, 1.259842519685033357 ) ) ;
#25924 = CARTESIAN_POINT ( 'NONE',  ( 0.08119777152254364916, 1.623385212329073957, 0.000000000000000000 ) ) ;
#25925 = ORIENTED_EDGE ( 'NONE', *, *, #29598, .F. ) ;
#25926 = ORIENTED_EDGE ( 'NONE', *, *, #47562, .F. ) ;
#25927 = EDGE_CURVE ( 'NONE', #29864, #23897, #11411, .T. ) ;
#25928 = DIRECTION ( 'NONE',  ( 1.000000000000000000, 0.000000000000000000, 0.000000000000000000 ) ) ;
#25929 = LINE ( 'NONE', #17677, #28245 ) ;
#25930 = PLANE ( 'NONE',  #46746 ) ;
#25931 = VERTEX_POINT ( 'NONE', #18398 ) ;
#25932 = FACE_OUTER_BOUND ( 'NONE', #25490, .T. ) ;
#25933 = DIRECTION ( 'NONE',  ( 1.734723475976806848E-16, -0.000000000000000000, 1.000000000000000000 ) ) ;
#25934 = ORIENTED_EDGE ( 'NONE', *, *, #2754, .F. ) ;
#25935 = EDGE_CURVE ( 'NONE', #13751, #49632, #26641, .T. ) ;
#25936 = EDGE_CURVE ( 'NONE', #15315, #38140, #49948, .T. ) ;
#25937 = LINE ( 'NONE', #45033, #18319 ) ;
#25938 = VERTEX_POINT ( 'NONE', #34404 ) ;
#25939 = ORIENTED_EDGE ( 'NONE', *, *, #28685, .T. ) ;
#25940 = DIRECTION ( 'NONE',  ( -1.000000000000000000, 0.000000000000000000, 0.000000000000000000 ) ) ;
#25941 = PLANE ( 'NONE',  #11049 ) ;
#25942 = LINE ( 'NONE', #6829, #17325 ) ;
#25943 = EDGE_LOOP ( 'NONE', ( #27954, #24051, #7543, #21095 ) ) ;
#25944 = CARTESIAN_POINT ( 'NONE',  ( 0.000000000000000000, 3.267716535433071279, 0.000000000000000000 ) ) ;
#25945 = LINE ( 'NONE', #50148, #29629 ) ;
#25946 = ORIENTED_EDGE ( 'NONE', *, *, #33563, .F. ) ;
#25947 =( REPRESENTATION_RELATIONSHIP ('NONE','NONE', #50198, #5020 ) REPRESENTATION_RELATIONSHIP_WITH_TRANSFORMATION ( #11886 )SHAPE_REPRESENTATION_RELATIONSHIP( ) );
#25948 = VECTOR ( 'NONE', #45222, 39.37007874015748143 ) ;
#25949 = CIRCLE ( 'NONE', #27583, 2.165354330708661568 ) ;
#25950 = EDGE_LOOP ( 'NONE', ( #23477, #10095, #18644, #45983 ) ) ;
#25951 = CARTESIAN_POINT ( 'NONE',  ( 0.000000000000000000, 3.267716535433071279, -1.299212598425192544 ) ) ;
#25952 = PLANE ( 'NONE',  #39944 ) ;
#25953 = AXIS2_PLACEMENT_3D ( 'NONE', #45375, #17524, #33284 ) ;
#25954 = VECTOR ( 'NONE', #18275, 39.37007874015748143 ) ;
#25955 = DIRECTION ( 'NONE',  ( 0.000000000000000000, -0.000000000000000000, 1.000000000000000000 ) ) ;
#25956 = CARTESIAN_POINT ( 'NONE',  ( -0.2834077913992259501, -0.6299212598425202314, -0.2440651625074179987 ) ) ;
#25957 = VECTOR ( 'NONE', #22919, 39.37007874015748143 ) ;
#25958 = ORIENTED_EDGE ( 'NONE', *, *, #13900, .F. ) ;
#25959 = CARTESIAN_POINT ( 'NONE',  ( 2.734482843737263025, 1.452693199995327644, -1.115254632218672270 ) ) ;
#25960 = CARTESIAN_POINT ( 'NONE',  ( -3.927031490892378253E-16, 3.346456692913386100, -2.204724409448811429 ) ) ;
#25961 = EDGE_LOOP ( 'NONE', ( #29212, #27609, #26283, #15836 ) ) ;
#25962 = LINE ( 'NONE', #37339, #47051 ) ;
#25963 = CARTESIAN_POINT ( 'NONE',  ( -0.3498457532482182053, 1.702298530840201662, 2.203421978946157989 ) ) ;
#25964 = ORIENTED_EDGE ( 'NONE', *, *, #16239, .T. ) ;
#25965 = LINE ( 'NONE', #45305, #24625 ) ;
#25966 = CARTESIAN_POINT ( 'NONE',  ( 2.182111253630085290, 3.267716535433071279, 0.1181102362204698858 ) ) ;
#25967 = CARTESIAN_POINT ( 'NONE',  ( 0.000000000000000000, 3.267716535433071279, -1.771653543307081025 ) ) ;
#25968 = EDGE_CURVE ( 'NONE', #45742, #19132, #36019, .T. ) ;
#25969 = ORIENTED_EDGE ( 'NONE', *, *, #18809, .F. ) ;
#25970 = FACE_OUTER_BOUND ( 'NONE', #43556, .T. ) ;
#25971 = VERTEX_POINT ( 'NONE', #31028 ) ;
#25972 = FACE_BOUND ( 'NONE', #27088, .T. ) ;
#25973 = EDGE_CURVE ( 'NONE', #19682, #47308, #42883, .T. ) ;
#25974 = CARTESIAN_POINT ( 'NONE',  ( -0.5455278134075217666, 3.226699998040866824, -2.401574803149598036 ) ) ;
#25975 = CARTESIAN_POINT ( 'NONE',  ( 1.287906020515830141, 3.267716535433071279, 1.062992125984246083 ) ) ;
#25977 = ADVANCED_FACE ( 'NONE', ( #7028 ), #1349, .T. ) ;
#25976 = DIRECTION ( 'NONE',  ( -1.000000000000000000, -0.000000000000000000, -0.000000000000000000 ) ) ;
#25978 = EDGE_CURVE ( 'NONE', #30890, #15224, #8550, .T. ) ;
#25979 = ORIENTED_EDGE ( 'NONE', *, *, #21092, .F. ) ;
#25980 = ORIENTED_EDGE ( 'NONE', *, *, #36362, .F. ) ;
#25981 = AXIS2_PLACEMENT_3D ( 'NONE', #30466, #29956, #11092 ) ;
#25982 = FACE_OUTER_BOUND ( 'NONE', #25297, .T. ) ;
#25983 = VECTOR ( 'NONE', #21540, 39.37007874015748143 ) ;
#25984 = AXIS2_PLACEMENT_3D ( 'NONE', #25572, #25825, #37467 ) ;
#25985 = LINE ( 'NONE', #37877, #44221 ) ;
#25986 = ORIENTED_EDGE ( 'NONE', *, *, #45059, .F. ) ;
#25987 = VECTOR ( 'NONE', #38612, 39.37007874015748143 ) ;
#25988 = DIRECTION ( 'NONE',  ( 1.734723475976806848E-16, -0.000000000000000000, 1.000000000000000000 ) ) ;
#25989 = EDGE_CURVE ( 'NONE', #373, #713, #39787, .T. ) ;
#25990 = ORIENTED_EDGE ( 'NONE', *, *, #41993, .F. ) ;
#25991 = CARTESIAN_POINT ( 'NONE',  ( 1.287906020515829919, 0.000000000000000000, -1.889763779527552368 ) ) ;
#25992 = DIRECTION ( 'NONE',  ( 1.000000000000000000, 0.000000000000000000, 0.000000000000000000 ) ) ;
#25993 = VECTOR ( 'NONE', #13027, 39.37007874015748143 ) ;
#25994 = ORIENTED_EDGE ( 'NONE', *, *, #37602, .F. ) ;
#25995 = EDGE_CURVE ( 'NONE', #35300, #41147, #37315, .T. ) ;
#25996 = DIRECTION ( 'NONE',  ( 1.160734090543304660E-16, -1.000000000000000000, 0.000000000000000000 ) ) ;
#25997 = ORIENTED_EDGE ( 'NONE', *, *, #25169, .T. ) ;
#25998 = VERTEX_POINT ( 'NONE', #35661 ) ;
#25999 = ADVANCED_FACE ( 'NONE', ( #35920 ), #28413, .F. ) ;
#26000 = ORIENTED_EDGE ( 'NONE', *, *, #13871, .F. ) ;
#26001 = ORIENTED_EDGE ( 'NONE', *, *, #35077, .T. ) ;
#26002 = LINE ( 'NONE', #37380, #7944 ) ;
#26003 = VERTEX_POINT ( 'NONE', #32310 ) ;
#26004 = DIRECTION ( 'NONE',  ( -3.469446951953613696E-16, 0.000000000000000000, -1.000000000000000000 ) ) ;
#26005 = EDGE_CURVE ( 'NONE', #19370, #34440, #14550, .T. ) ;
#26006 = DIRECTION ( 'NONE',  ( 0.000000000000000000, 1.000000000000000000, 0.000000000000000000 ) ) ;
#26007 = DIRECTION ( 'NONE',  ( -0.01601477604151182663, 0.9998717552508123996, -0.000000000000000000 ) ) ;
#26008 = CARTESIAN_POINT ( 'NONE',  ( -1.325491792074585451, 1.600165750963108646, -2.638988599164751481 ) ) ;
#26009 = DIRECTION ( 'NONE',  ( -0.7227948638273878901, 0.000000000000000000, -0.6910626489868684219 ) ) ;
#26010 = VECTOR ( 'NONE', #48700, 39.37007874015748143 ) ;
#26011 = ORIENTED_EDGE ( 'NONE', *, *, #43364, .T. ) ;
#26012 = DIRECTION ( 'NONE',  ( -1.000000000000000000, 0.000000000000000000, 1.734723475976806848E-16 ) ) ;
#26013 = CARTESIAN_POINT ( 'NONE',  ( -0.5455278134075214336, 0.000000000000000000, 0.3149606299212577287 ) ) ;
#26014 = CONICAL_SURFACE ( 'NONE', #32584, 3.483074324928249421, 1.244861948955335196 ) ;
#26015 = PLANE ( 'NONE',  #16095 ) ;
#26016 = VECTOR ( 'NONE', #50796, 39.37007874015748143 ) ;
#26017 = CARTESIAN_POINT ( 'NONE',  ( 0.8182917201112819283, 3.267716535433071279, 1.102362204724403938 ) ) ;
#26018 = EDGE_LOOP ( 'NONE', ( #10819, #1378, #42669, #29189 ) ) ;
#26019 = DIRECTION ( 'NONE',  ( 0.000000000000000000, -1.000000000000000000, 0.000000000000000000 ) ) ;
#26020 = PLANE ( 'NONE',  #35998 ) ;
#26021 = ORIENTED_EDGE ( 'NONE', *, *, #44483, .F. ) ;
#26022 = CARTESIAN_POINT ( 'NONE',  ( -0.2783729501556720387, 0.02346101323895649626, 1.809574371873096110 ) ) ;
#26023 = AXIS2_PLACEMENT_3D ( 'NONE', #38252, #2874, #18627 ) ;
#26024 = LINE ( 'NONE', #2022, #19333 ) ;
#26025 = AXIS2_PLACEMENT_3D ( 'NONE', #30296, #46017, #1652 ) ;
#26026 = ORIENTED_EDGE ( 'NONE', *, *, #10399, .T. ) ;
#26027 = ORIENTED_EDGE ( 'NONE', *, *, #44685, .T. ) ;
#26028 = LINE ( 'NONE', #41778, #51 ) ;
#26029 = ADVANCED_FACE ( 'NONE', ( #47233 ), #8034, .F. ) ;
#26030 = LINE ( 'NONE', #42031, #44832 ) ;
#26031 = CARTESIAN_POINT ( 'NONE',  ( -1.472219874544909768, 1.597879704547665369, 2.560030851058948898 ) ) ;
#26032 = DIRECTION ( 'NONE',  ( 0.9989930665413151445, 0.000000000000000000, -0.04486483035050446017 ) ) ;
#26033 = DIRECTION ( 'NONE',  ( -1.000000000000000000, 0.000000000000000000, 0.000000000000000000 ) ) ;
#26034 = ORIENTED_EDGE ( 'NONE', *, *, #18926, .T. ) ;
#26035 = ADVANCED_FACE ( 'NONE', ( #7783 ), #28155, .F. ) ;
#26036 = DIRECTION ( 'NONE',  ( 0.000000000000000000, 0.000000000000000000, -1.000000000000000000 ) ) ;
#26037 = ORIENTED_EDGE ( 'NONE', *, *, #16332, .F. ) ;
#26038 = ORIENTED_EDGE ( 'NONE', *, *, #40317, .F. ) ;
#26039 = DIRECTION ( 'NONE',  ( 0.000000000000000000, -1.000000000000000000, 0.000000000000000000 ) ) ;
#26040 = EDGE_LOOP ( 'NONE', ( #44021, #27985, #29981 ) ) ;
#26041 = LINE ( 'NONE', #49995, #41134 ) ;
#26042 = DIRECTION ( 'NONE',  ( 5.500355109725658086E-17, -1.000000000000000000, 1.022137253806229789E-16 ) ) ;
#26043 = ORIENTED_EDGE ( 'NONE', *, *, #25617, .T. ) ;
#26044 = CARTESIAN_POINT ( 'NONE',  ( -1.299212598425207865, 3.267716535433071279, 1.732283464566920950 ) ) ;
#26045 = LINE ( 'NONE', #22433, #34788 ) ;
#26046 = DIRECTION ( 'NONE',  ( -0.000000000000000000, 1.000000000000000000, -0.000000000000000000 ) ) ;
#26047 = VECTOR ( 'NONE', #29766, 39.37007874015748143 ) ;
#26048 = ORIENTED_EDGE ( 'NONE', *, *, #21861, .F. ) ;
#26049 = EDGE_LOOP ( 'NONE', ( #397, #39642, #41710, #5610 ) ) ;
#26050 = CIRCLE ( 'NONE', #1282, 0.3740157480314960647 ) ;
#26051 = CARTESIAN_POINT ( 'NONE',  ( -2.926032761125793247, 0.000000000000000000, 0.3963580683592094478 ) ) ;
#26052 = FACE_BOUND ( 'NONE', #8426, .T. ) ;
#26053 = ORIENTED_EDGE ( 'NONE', *, *, #34088, .T. ) ;
#26054 = AXIS2_PLACEMENT_3D ( 'NONE', #8255, #23740, #36137 ) ;
#26055 = LINE ( 'NONE', #6183, #37781 ) ;
#26056 = DIRECTION ( 'NONE',  ( 0.000000000000000000, 0.000000000000000000, -1.000000000000000000 ) ) ;
#26057 = AXIS2_PLACEMENT_3D ( 'NONE', #42179, #25674, #6819 ) ;
#26058 = EDGE_CURVE ( 'NONE', #14448, #42497, #11906, .T. ) ;
#26059 = ORIENTED_EDGE ( 'NONE', *, *, #17766, .F. ) ;
#26060 = ORIENTED_EDGE ( 'NONE', *, *, #37683, .F. ) ;
#26061 = DIRECTION ( 'NONE',  ( -9.701723960855857903E-17, 1.000000000000000000, 8.476140964546263859E-17 ) ) ;
#26062 = AXIS2_PLACEMENT_3D ( 'NONE', #32474, #5089, #49681 ) ;
#26063 = PLANE ( 'NONE',  #39715 ) ;
#26064 = ORIENTED_EDGE ( 'NONE', *, *, #6497, .F. ) ;
#26065 = ORIENTED_EDGE ( 'NONE', *, *, #21728, .T. ) ;
#26066 = EDGE_CURVE ( 'NONE', #11553, #48423, #15775, .T. ) ;
#26067 = ORIENTED_EDGE ( 'NONE', *, *, #13219, .F. ) ;
#26068 = DIRECTION ( 'NONE',  ( 1.000000000000000000, 0.000000000000000000, 0.000000000000000000 ) ) ;
#26069 = CARTESIAN_POINT ( 'NONE',  ( -0.8182917201112819283, 0.000000000000000000, -1.614173228346451605 ) ) ;
#26070 = EDGE_CURVE ( 'NONE', #43045, #39291, #805, .T. ) ;
#26071 = EDGE_CURVE ( 'NONE', #30219, #38377, #3914, .T. ) ;
#26072 = CARTESIAN_POINT ( 'NONE',  ( -2.151809081513409438, 1.673437530708463017, 0.2418202932658340965 ) ) ;
#26073 = CARTESIAN_POINT ( 'NONE',  ( -1.091055626815042201, 0.000000000000000000, 0.9448818897637749625 ) ) ;
#26074 = VERTEX_POINT ( 'NONE', #46980 ) ;
#26075 = ORIENTED_EDGE ( 'NONE', *, *, #7827, .T. ) ;
#26076 = CARTESIAN_POINT ( 'NONE',  ( -0.9914495361339011881, 1.605369965488712136, 2.781765111341808705 ) ) ;
#26077 = CARTESIAN_POINT ( 'NONE',  ( -1.363819533518803473, 3.346456692913386100, -0.6692913385826760875 ) ) ;
#26078 = ADVANCED_FACE ( 'NONE', ( #12420 ), #19642, .F. ) ;
#26079 = DIRECTION ( 'NONE',  ( 0.000000000000000000, -1.000000000000000000, 0.000000000000000000 ) ) ;
#26080 = ADVANCED_FACE ( 'NONE', ( #43900 ), #40044, .F. ) ;
#26081 = CARTESIAN_POINT ( 'NONE',  ( -0.1181847168586561830, 0.01737573915606907896, -1.862146645277666934 ) ) ;
#26082 = CARTESIAN_POINT ( 'NONE',  ( -1.091055626815042201, 0.000000000000000000, 1.062992125984246083 ) ) ;
#26083 = CIRCLE ( 'NONE', #44201, 2.164630168518208109 ) ;
#26084 = DIRECTION ( 'NONE',  ( -0.000000000000000000, 0.000000000000000000, 1.000000000000000000 ) ) ;
#26085 = ORIENTED_EDGE ( 'NONE', *, *, #41257, .T. ) ;
#26086 = CIRCLE ( 'NONE', #37632, 2.443628662382284489 ) ;
#26087 = DIRECTION ( 'NONE',  ( 0.000000000000000000, 0.000000000000000000, -1.000000000000000000 ) ) ;
#26088 = CARTESIAN_POINT ( 'NONE',  ( 1.927369588301418135, 0.5223483550995119407, -1.213278145923846862 ) ) ;
#26089 = VERTEX_POINT ( 'NONE', #27904 ) ;
#26090 = VECTOR ( 'NONE', #6242, 39.37007874015748143 ) ;
#26092 = EDGE_CURVE ( 'NONE', #45803, #11936, #16039, .T. ) ;
#26091 = ORIENTED_EDGE ( 'NONE', *, *, #7903, .T. ) ;
#26093 = PLANE ( 'NONE',  #7217 ) ;
#26094 = VECTOR ( 'NONE', #14832, 39.37007874015748143 ) ;
#26095 = ORIENTED_EDGE ( 'NONE', *, *, #45120, .F. ) ;
#26096 = EDGE_CURVE ( 'NONE', #21949, #8694, #47494, .T. ) ;
#26097 = VECTOR ( 'NONE', #9417, 39.37007874015748143 ) ;
#26098 = EDGE_CURVE ( 'NONE', #42847, #31120, #40315, .T. ) ;
#26099 = ORIENTED_EDGE ( 'NONE', *, *, #20604, .T. ) ;
#26100 = DIRECTION ( 'NONE',  ( -0.000000000000000000, -1.000000000000000000, 0.000000000000000000 ) ) ;
#26101 = ORIENTED_EDGE ( 'NONE', *, *, #9144, .F. ) ;
#26102 = DIRECTION ( 'NONE',  ( 1.000000000000000000, -0.000000000000000000, 0.000000000000000000 ) ) ;
#26103 = LINE ( 'NONE', #46449, #32154 ) ;
#26104 = EDGE_CURVE ( 'NONE', #912, #36517, #8291, .T. ) ;
#26105 = ORIENTED_EDGE ( 'NONE', *, *, #44017, .F. ) ;
#26106 = ORIENTED_EDGE ( 'NONE', *, *, #8465, .T. ) ;
#26107 = DIRECTION ( 'NONE',  ( 1.086719731106949452E-16, -1.000000000000000000, -4.078527368698568598E-17 ) ) ;
#26108 = ORIENTED_EDGE ( 'NONE', *, *, #14702, .F. ) ;
#26109 = VERTEX_POINT ( 'NONE', #2529 ) ;
#26110 = CARTESIAN_POINT ( 'NONE',  ( 1.091055626815042645, 0.000000000000000000, -0.9448818897637765168 ) ) ;
#26111 = LINE ( 'NONE', #26856, #46581 ) ;
#26112 = CARTESIAN_POINT ( 'NONE',  ( -1.402715216960007005, 0.000000000000000000, 1.097573363406495472 ) ) ;
#26113 = DIRECTION ( 'NONE',  ( -0.8805955318567322276, 0.000000000000000000, -0.4738686624730094610 ) ) ;
#26114 = ORIENTED_EDGE ( 'NONE', *, *, #42774, .F. ) ;
#26115 = CARTESIAN_POINT ( 'NONE',  ( 0.8182917201112819283, 0.000000000000000000, 1.102362204724403938 ) ) ;
#26116 = DIRECTION ( 'NONE',  ( -1.000000000000000000, 0.000000000000000000, 1.734723475976806848E-16 ) ) ;
#26117 = DIRECTION ( 'NONE',  ( 0.000000000000000000, 0.000000000000000000, -1.000000000000000000 ) ) ;
#26118 = CIRCLE ( 'NONE', #32741, 0.3740157480314961203 ) ;
#26119 = ORIENTED_EDGE ( 'NONE', *, *, #15940, .F. ) ;
#26120 = FACE_OUTER_BOUND ( 'NONE', #18376, .T. ) ;
#26121 = DIRECTION ( 'NONE',  ( -0.000000000000000000, 0.000000000000000000, 1.000000000000000000 ) ) ;
#26122 = AXIS2_PLACEMENT_3D ( 'NONE', #14899, #35282, #31152 ) ;
#26123 = LINE ( 'NONE', #25869, #31540 ) ;
#26124 = EDGE_LOOP ( 'NONE', ( #34694, #50271, #28323, #46817, #48042 ) ) ;
#26125 = VERTEX_POINT ( 'NONE', #42023 ) ;
#26126 =( LENGTH_UNIT ( ) NAMED_UNIT ( * ) SI_UNIT ( $, .METRE. ) );
#26127 = LINE ( 'NONE', #38016, #16 ) ;
#26128 = EDGE_CURVE ( 'NONE', #43511, #2179, #17865, .T. ) ;
#26129 =( BOUNDED_CURVE ( )  B_SPLINE_CURVE ( 3, ( #15921, #946, #35806, #31677 ),
 .UNSPECIFIED., .F., .F. ) 
 B_SPLINE_CURVE_WITH_KNOTS ( ( 4, 4 ),
 ( 1.648115238091181434, 1.699061793389599950 ),
 .UNSPECIFIED. ) 
 CURVE ( )  GEOMETRIC_REPRESENTATION_ITEM ( )  RATIONAL_B_SPLINE_CURVE ( ( 1.000000000000000000, 0.9997837157376677775, 0.9997837157376677775, 1.000000000000000000 ) ) 
 REPRESENTATION_ITEM ( '' )  );
#26130 = AXIS2_PLACEMENT_3D ( 'NONE', #1362, #13247, #2126 ) ;
#26131 = ADVANCED_FACE ( 'NONE', ( #45360 ), #26020, .F. ) ;
#26132 = CARTESIAN_POINT ( 'NONE',  ( -1.591447364397243103, 0.002429723416550041374, -0.7337366736851151927 ) ) ;
#26133 = CARTESIAN_POINT ( 'NONE',  ( 0.000000000000000000, 1.574803149606302854, 0.000000000000000000 ) ) ;
#26134 = ORIENTED_EDGE ( 'NONE', *, *, #23677, .T. ) ;
#26136 = EDGE_CURVE ( 'NONE', #43954, #26976, #50774, .T. ) ;
#26135 = ORIENTED_EDGE ( 'NONE', *, *, #35178, .T. ) ;
#26137 = AXIS2_PLACEMENT_3D ( 'NONE', #30559, #50868, #47013 ) ;
#26138 = CARTESIAN_POINT ( 'NONE',  ( 2.739172746247211965, 1.660034045467230657, -0.1722785920648685354 ) ) ;
#26139 = ORIENTED_EDGE ( 'NONE', *, *, #22592, .T. ) ;
#26140 = CARTESIAN_POINT ( 'NONE',  ( 0.4435105686220205401, -2.456726483784180385E-16, 2.168331686854577001 ) ) ;
#26141 = DIRECTION ( 'NONE',  ( 0.000000000000000000, 0.000000000000000000, -1.000000000000000000 ) ) ;
#26142 = LINE ( 'NONE', #30015, #28328 ) ;
#26143 = DIRECTION ( 'NONE',  ( 0.000000000000000000, -1.000000000000000000, 0.000000000000000000 ) ) ;
#26144 = CARTESIAN_POINT ( 'NONE',  ( -1.556712866041156662, 1.548291375251236834, 2.509548638715847435 ) ) ;
#26145 = ORIENTED_EDGE ( 'NONE', *, *, #5851, .T. ) ;
#26146 = CARTESIAN_POINT ( 'NONE',  ( 0.000000000000000000, 3.267716535433071279, -0.5118110236220471121 ) ) ;
#26147 = SURFACE_SIDE_STYLE ('',( #33904 ) ) ;
#26148 = ADVANCED_FACE ( 'NONE', ( #41513 ), #25509, .F. ) ;
#26149 = CARTESIAN_POINT ( 'NONE',  ( -0.5455278134075208785, 3.346456692913386100, 0.6299212598425164567 ) ) ;
#26150 = ORIENTED_EDGE ( 'NONE', *, *, #43827, .F. ) ;
#26151 = CARTESIAN_POINT ( 'NONE',  ( -0.5455278134075214336, 0.000000000000000000, -1.456692913385822630 ) ) ;
#26152 = EDGE_CURVE ( 'NONE', #22204, #19885, #17767, .T. ) ;
#26153 = DIRECTION ( 'NONE',  ( 0.000000000000000000, -1.000000000000000000, 0.000000000000000000 ) ) ;
#26154 = PLANE ( 'NONE',  #7347 ) ;
#26155 = AXIS2_PLACEMENT_3D ( 'NONE', #36638, #33281, #24760 ) ;
#26156 = ORIENTED_EDGE ( 'NONE', *, *, #914, .T. ) ;
#26157 = VECTOR ( 'NONE', #3732, 39.37007874015748143 ) ;
#26158 = EDGE_CURVE ( 'NONE', #42434, #30956, #40311, .T. ) ;
#26159 = DIRECTION ( 'NONE',  ( -1.000000000000000000, 0.000000000000000000, 1.734723475976806848E-16 ) ) ;
#26160 = VECTOR ( 'NONE', #38594, 39.37007874015748143 ) ;
#26161 = EDGE_CURVE ( 'NONE', #28900, #39490, #6146, .T. ) ;
#26162 = EDGE_CURVE ( 'NONE', #44897, #19562, #18532, .T. ) ;
#26163 = VERTEX_POINT ( 'NONE', #2780 ) ;
#26164 = DIRECTION ( 'NONE',  ( -1.858431260983764056E-16, -0.7660444431189770143, 0.6427876096865403621 ) ) ;
#26165 = ORIENTED_EDGE ( 'NONE', *, *, #36454, .F. ) ;
#26166 = DIRECTION ( 'NONE',  ( -3.469446951953613696E-16, 0.000000000000000000, -1.000000000000000000 ) ) ;
#26167 = PLANE ( 'NONE',  #50680 ) ;
#26168 = FACE_OUTER_BOUND ( 'NONE', #48358, .T. ) ;
#26169 = DIRECTION ( 'NONE',  ( 0.000000000000000000, -1.000000000000000000, 0.000000000000000000 ) ) ;
#26170 = ORIENTED_EDGE ( 'NONE', *, *, #43547, .F. ) ;
#26171 = EDGE_LOOP ( 'NONE', ( #39181, #42127, #20011, #32475 ) ) ;
#26172 = CARTESIAN_POINT ( 'NONE',  ( -1.929629134066536134, 1.574803149606302854, 0.9824921284572128988 ) ) ;
#26173 = CARTESIAN_POINT ( 'NONE',  ( -2.277873973731453727, 1.562946399538843290, 1.879489153247635214 ) ) ;
#26174 = ORIENTED_EDGE ( 'NONE', *, *, #11830, .T. ) ;
#26175 = CARTESIAN_POINT ( 'NONE',  ( -1.110003343315104862, 1.595669590305086816, -2.191522224601501367 ) ) ;
#26176 = DIRECTION ( 'NONE',  ( -0.000000000000000000, 1.000000000000000000, -0.000000000000000000 ) ) ;
#26177 = DIRECTION ( 'NONE',  ( 0.9998717552508121775, 0.01601477604151182663, 0.000000000000000000 ) ) ;
#26178 = ORIENTED_EDGE ( 'NONE', *, *, #27076, .F. ) ;
#26179 = VERTEX_POINT ( 'NONE', #20673 ) ;
#26180 = CARTESIAN_POINT ( 'NONE',  ( -2.174914189033237299, 3.240375350693514456, -1.141732283464563791 ) ) ;
#26181 = PLANE ( 'NONE',  #36524 ) ;
#26182 = CARTESIAN_POINT ( 'NONE',  ( 0.3467207527347885843, -2.578434962089329135E-16, 2.186201806782070545 ) ) ;
#26183 = ORIENTED_EDGE ( 'NONE', *, *, #7267, .F. ) ;
#26184 = DIRECTION ( 'NONE',  ( 1.000000000000000000, -0.000000000000000000, 0.000000000000000000 ) ) ;
#26185 = CARTESIAN_POINT ( 'NONE',  ( -3.414809992080329023E-17, 0.000000000000000000, -0.1968503937007874405 ) ) ;
#26186 = ORIENTED_EDGE ( 'NONE', *, *, #39726, .F. ) ;
#26187 = LINE ( 'NONE', #18446, #2653 ) ;
#26188 = EDGE_LOOP ( 'NONE', ( #48227, #41736, #14433, #26387 ) ) ;
#26189 = VERTEX_POINT ( 'NONE', #34284 ) ;
#26190 = CARTESIAN_POINT ( 'NONE',  ( -1.439733046521776361, 3.267716535433071279, 1.062992125984246083 ) ) ;
#26191 = DIRECTION ( 'NONE',  ( -1.000000000000000000, 0.000000000000000000, -0.000000000000000000 ) ) ;
#26192 = CARTESIAN_POINT ( 'NONE',  ( -0.5455278134075208785, 0.000000000000000000, 1.692913385826762873 ) ) ;
#26193 = AXIS2_PLACEMENT_3D ( 'NONE', #11175, #50601, #35679 ) ;
#26194 = AXIS2_PLACEMENT_3D ( 'NONE', #11108, #50046, #50291 ) ;
#26195 = ORIENTED_EDGE ( 'NONE', *, *, #37358, .F. ) ;
#26196 = DIRECTION ( 'NONE',  ( -1.000000000000000000, 0.000000000000000000, 1.734723475976806848E-16 ) ) ;
#26197 = FACE_OUTER_BOUND ( 'NONE', #10509, .T. ) ;
#26198 = ORIENTED_EDGE ( 'NONE', *, *, #20054, .T. ) ;
#26199 = EDGE_CURVE ( 'NONE', #50303, #6760, #6338, .T. ) ;
#26200 = EDGE_CURVE ( 'NONE', #27482, #26900, #27395, .T. ) ;
#26201 = VECTOR ( 'NONE', #46656, 39.37007874015748143 ) ;
#26202 = VERTEX_POINT ( 'NONE', #48260 ) ;
#26203 = CARTESIAN_POINT ( 'NONE',  ( 0.7381027496705270252, 1.499047760149736952, -2.859439394060913298 ) ) ;
#26204 = EDGE_CURVE ( 'NONE', #11067, #19232, #14655, .T. ) ;
#26205 = PLANE ( 'NONE',  #25128 ) ;
#26206 = DIRECTION ( 'NONE',  ( 1.000000000000000000, 0.000000000000000000, 0.000000000000000000 ) ) ;
#26207 = CIRCLE ( 'NONE', #50075, 2.443628662382284489 ) ;
#26208 = LINE ( 'NONE', #11474, #40174 ) ;
#26209 = CARTESIAN_POINT ( 'NONE',  ( -2.168245791271168343, 1.587034731952809752, -2.004968704497279930 ) ) ;
#26210 = ORIENTED_EDGE ( 'NONE', *, *, #45086, .F. ) ;
#26211 = DIRECTION ( 'NONE',  ( 1.000000000000000000, 0.000000000000000000, 0.000000000000000000 ) ) ;
#26212 = AXIS2_PLACEMENT_3D ( 'NONE', #25441, #33207, #48890 ) ;
#26213 = PLANE ( 'NONE',  #37263 ) ;
#26214 = VERTEX_POINT ( 'NONE', #1054 ) ;
#26215 = CARTESIAN_POINT ( 'NONE',  ( 0.4696143004045476577, 0.000000000000000000, -2.047244094488182231 ) ) ;
#26216 = EDGE_CURVE ( 'NONE', #19232, #12600, #29898, .T. ) ;
#26217 = DIRECTION ( 'NONE',  ( 1.000000000000000000, 0.000000000000000000, -3.469446951953613696E-16 ) ) ;
#26218 = ORIENTED_EDGE ( 'NONE', *, *, #19307, .T. ) ;
#26219 = CARTESIAN_POINT ( 'NONE',  ( -2.001301579076982584, 3.267716535433071279, -0.8267716535433052849 ) ) ;
#26220 = CARTESIAN_POINT ( 'NONE',  ( 1.636583440222563857, 0.000000000000000000, 1.259842519685033135 ) ) ;
#26221 = CARTESIAN_POINT ( 'NONE',  ( 0.7697133566244497294, 1.497596064125990667, -2.850715420863024985 ) ) ;
#26222 = EDGE_CURVE ( 'NONE', #4005, #22546, #533, .T. ) ;
#26223 = ORIENTED_EDGE ( 'NONE', *, *, #26912, .T. ) ;
#26224 = PLANE ( 'NONE',  #18901 ) ;
#26225 = ORIENTED_EDGE ( 'NONE', *, *, #18868, .F. ) ;
#26226 = FACE_BOUND ( 'NONE', #14126, .T. ) ;
#26227 = LINE ( 'NONE', #41976, #15215 ) ;
#26228 = LINE ( 'NONE', #14613, #11128 ) ;
#26229 = PLANE ( 'NONE',  #25187 ) ;
#26230 = VECTOR ( 'NONE', #39175, 39.37007874015748143 ) ;
#26231 = AXIS2_PLACEMENT_3D ( 'NONE', #2541, #34547, #26531 ) ;
#26232 = VERTEX_POINT ( 'NONE', #37400 ) ;
#26233 = VERTEX_POINT ( 'NONE', #33533 ) ;
#26234 = CARTESIAN_POINT ( 'NONE',  ( -1.010509689441836390, 0.01173450346422093109, -1.474572740271697047 ) ) ;
#26235 = LINE ( 'NONE', #14620, #41122 ) ;
#26236 = VECTOR ( 'NONE', #39328, 39.37007874015748143 ) ;
#26237 = DIRECTION ( 'NONE',  ( -1.000000000000000000, -0.000000000000000000, -0.000000000000000000 ) ) ;
#26238 = FACE_BOUND ( 'NONE', #29646, .T. ) ;
#26239 = DIRECTION ( 'NONE',  ( -1.000000000000000000, -0.000000000000000000, -0.000000000000000000 ) ) ;
#26240 = VECTOR ( 'NONE', #43406, 39.37007874015748143 ) ;
#26241 = ORIENTED_EDGE ( 'NONE', *, *, #37449, .F. ) ;
#26242 = LINE ( 'NONE', #29352, #15071 ) ;
#26243 = VECTOR ( 'NONE', #40682, 39.37007874015748143 ) ;
#26244 = DIRECTION ( 'NONE',  ( -0.01601477604151182663, 0.9998717552508123996, -0.000000000000000000 ) ) ;
#26245 = ORIENTED_EDGE ( 'NONE', *, *, #39477, .T. ) ;
#26246 = LINE ( 'NONE', #18758, #37319 ) ;
#26247 = ORIENTED_EDGE ( 'NONE', *, *, #6058, .F. ) ;
#26248 = ORIENTED_EDGE ( 'NONE', *, *, #13256, .F. ) ;
#26249 = VECTOR ( 'NONE', #5642, 39.37007874015748143 ) ;
#26250 = ORIENTED_EDGE ( 'NONE', *, *, #36408, .F. ) ;
#26251 = ORIENTED_EDGE ( 'NONE', *, *, #42412, .F. ) ;
#26252 = CARTESIAN_POINT ( 'NONE',  ( -0.7148041136150262709, 1.205361022782829114E-17, -2.044646019095620826 ) ) ;
#26253 = EDGE_CURVE ( 'NONE', #34410, #42971, #13895, .T. ) ;
#26254 = EDGE_CURVE ( 'NONE', #44436, #2513, #2273, .T. ) ;
#26255 = ORIENTED_EDGE ( 'NONE', *, *, #7946, .F. ) ;
#26256 = LINE ( 'NONE', #37128, #27071 ) ;
#26257 = CARTESIAN_POINT ( 'NONE',  ( 0.000000000000000000, 0.000000000000000000, 0.000000000000000000 ) ) ;
#26258 = EDGE_CURVE ( 'NONE', #18949, #7323, #50715, .T. ) ;
#26259 = CIRCLE ( 'NONE', #4003, 2.106299212598425008 ) ;
#26260 = ADVANCED_FACE ( 'NONE', ( #4055 ), #34784, .F. ) ;
#26261 = CARTESIAN_POINT ( 'NONE',  ( 1.091055626815042645, 3.346456692913386100, 0.9448818897637746295 ) ) ;
#26262 = DIRECTION ( 'NONE',  ( -0.01601477604151182663, 0.9998717552508123996, -0.000000000000000000 ) ) ;
#26263 = DIRECTION ( 'NONE',  ( -3.469446951953613696E-16, 0.000000000000000000, -1.000000000000000000 ) ) ;
#26264 = ORIENTED_EDGE ( 'NONE', *, *, #18983, .F. ) ;
#26265 = CARTESIAN_POINT ( 'NONE',  ( 0.000000000000000000, 0.000000000000000000, 0.000000000000000000 ) ) ;
#26266 = DIRECTION ( 'NONE',  ( -1.000000000000000000, -0.000000000000000000, -0.000000000000000000 ) ) ;
#26267 = VECTOR ( 'NONE', #27599, 39.37007874015748143 ) ;
#26268 = DIRECTION ( 'NONE',  ( -3.469446951953613696E-16, 0.000000000000000000, -1.000000000000000000 ) ) ;
#26269 = DIRECTION ( 'NONE',  ( 1.000000000000000000, -0.000000000000000000, 0.000000000000000000 ) ) ;
#26270 = VECTOR ( 'NONE', #42489, 39.37007874015748143 ) ;
#26271 = VECTOR ( 'NONE', #2804, 39.37007874015748143 ) ;
#26272 = EDGE_LOOP ( 'NONE', ( #6816, #31666, #26590, #12819 ) ) ;
#26273 = DIRECTION ( 'NONE',  ( -0.000000000000000000, 1.000000000000000000, -0.000000000000000000 ) ) ;
#26274 = EDGE_CURVE ( 'NONE', #29685, #33217, #30658, .T. ) ;
#26275 = DIRECTION ( 'NONE',  ( 1.734723475976806848E-16, -0.000000000000000000, 1.000000000000000000 ) ) ;
#26276 = VERTEX_POINT ( 'NONE', #42265 ) ;
#26277 = DIRECTION ( 'NONE',  ( -1.000000000000000000, 0.000000000000000000, 0.000000000000000000 ) ) ;
#26278 = CARTESIAN_POINT ( 'NONE',  ( 0.000000000000000000, 3.267716535433071279, 0.7480314960629874665 ) ) ;
#26279 = MECHANICAL_DESIGN_GEOMETRIC_PRESENTATION_REPRESENTATION (  '', ( #34540 ), #44432 ) ;
#26280 = VERTEX_POINT ( 'NONE', #39157 ) ;
#26281 = EDGE_CURVE ( 'NONE', #17189, #1621, #25585, .T. ) ;
#26282 = VECTOR ( 'NONE', #1451, 39.37007874015748143 ) ;
#26283 = ORIENTED_EDGE ( 'NONE', *, *, #23732, .F. ) ;
#26284 = B_SPLINE_CURVE_WITH_KNOTS ( 'NONE', 3,
 ( #28627, #29396, #47956, #40515 ),
 .UNSPECIFIED., .F., .F.,
 ( 4, 4 ),
 ( 2.007575928058895981E-07, 0.002500799887775291813 ),
 .UNSPECIFIED. ) ;
#26285 = CARTESIAN_POINT ( 'NONE',  ( 0.7855418668307558860, 0.000000000000000000, -2.846347029613733870 ) ) ;
#26286 = DIRECTION ( 'NONE',  ( 1.000000000000000000, 0.000000000000000000, 0.000000000000000000 ) ) ;
#26287 = PLANE ( 'NONE',  #50889 ) ;
#26288 = CARTESIAN_POINT ( 'NONE',  ( -1.088097428176262760, 1.690474079180120492, 1.917118167796188821 ) ) ;
#26289 = CARTESIAN_POINT ( 'NONE',  ( -0.8182917201112814842, 0.000000000000000000, 0.5905511811023582691 ) ) ;
#26290 = VERTEX_POINT ( 'NONE', #26519 ) ;
#26291 = FACE_OUTER_BOUND ( 'NONE', #8914, .T. ) ;
#26292 = VERTEX_POINT ( 'NONE', #3795 ) ;
#26293 = EDGE_LOOP ( 'NONE', ( #9198, #17980, #36580, #20420 ) ) ;
#26294 = CARTESIAN_POINT ( 'NONE',  ( -1.353122744573580727, 3.346456692913386100, -1.614173228346451605 ) ) ;
#26295 = ORIENTED_EDGE ( 'NONE', *, *, #13469, .F. ) ;
#26296 = CARTESIAN_POINT ( 'NONE',  ( 1.387661672111480948, 5.905511811023623991, -1.663104731517921930 ) ) ;
#26297 = CARTESIAN_POINT ( 'NONE',  ( 1.015142113812069091, 3.267716535433071279, -1.912654141836395816 ) ) ;
#26298 = EDGE_CURVE ( 'NONE', #47500, #41777, #38907, .T. ) ;
#26299 = ORIENTED_EDGE ( 'NONE', *, *, #38149, .F. ) ;
#26300 = CARTESIAN_POINT ( 'NONE',  ( -2.139229417893219853, 1.205361022782829114E-17, -0.3394403656973710159 ) ) ;
#26301 = VECTOR ( 'NONE', #2237, 39.37007874015748143 ) ;
#26302 = LINE ( 'NONE', #37687, #50393 ) ;
#26303 = CARTESIAN_POINT ( 'NONE',  ( 1.636583440222563635, 3.346456692913386100, -1.417869535855832419 ) ) ;
#26304 = ORIENTED_EDGE ( 'NONE', *, *, #9644, .T. ) ;
#26305 = ORIENTED_EDGE ( 'NONE', *, *, #49291, .T. ) ;
#26306 = CARTESIAN_POINT ( 'NONE',  ( 0.8069532150559736161, 1.205361022782829114E-17, -2.010061882867131278 ) ) ;
#26307 = FACE_BOUND ( 'NONE', #45932, .T. ) ;
#26308 = EDGE_LOOP ( 'NONE', ( #49292, #2107, #12282, #33670 ) ) ;
#26309 = VECTOR ( 'NONE', #4203, 39.37007874015748143 ) ;
#26310 = LINE ( 'NONE', #38201, #15472 ) ;
#26311 = LINE ( 'NONE', #33823, #24244 ) ;
#26312 = ORIENTED_EDGE ( 'NONE', *, *, #9663, .F. ) ;
#26313 = ORIENTED_EDGE ( 'NONE', *, *, #23252, .T. ) ;
#26314 = VECTOR ( 'NONE', #21782, 39.37007874015748143 ) ;
#26315 = DIRECTION ( 'NONE',  ( -3.469446951953613696E-16, 0.000000000000000000, -1.000000000000000000 ) ) ;
#26316 = LINE ( 'NONE', #7208, #5608 ) ;
#26317 = VERTEX_POINT ( 'NONE', #11033 ) ;
#26318 = EDGE_LOOP ( 'NONE', ( #40957, #23502, #14381, #13366 ) ) ;
#26319 = VECTOR ( 'NONE', #33977, 39.37007874015748143 ) ;
#26320 = ORIENTED_EDGE ( 'NONE', *, *, #46451, .F. ) ;
#26321 = DIRECTION ( 'NONE',  ( 0.000000000000000000, 1.000000000000000000, 0.000000000000000000 ) ) ;
#26322 = EDGE_CURVE ( 'NONE', #5168, #5952, #46371, .T. ) ;
#26323 = CARTESIAN_POINT ( 'NONE',  ( 1.091055626815042645, 3.346456692913386100, -0.8267716535433055070 ) ) ;
#26324 = EDGE_CURVE ( 'NONE', #16783, #972, #7167, .T. ) ;
#26325 = ADVANCED_FACE ( 'NONE', ( #35544 ), #7665, .F. ) ;
#26326 = DIRECTION ( 'NONE',  ( 1.734723475976806848E-16, -0.000000000000000000, 1.000000000000000000 ) ) ;
#26327 = EDGE_LOOP ( 'NONE', ( #46868, #31827, #42541, #11153, #37212, #10576, #11385, #17417, #22436, #41105, #39333 ) ) ;
#26328 = ORIENTED_EDGE ( 'NONE', *, *, #16184, .F. ) ;
#26329 = LINE ( 'NONE', #41568, #39796 ) ;
#26330 = DIRECTION ( 'NONE',  ( 0.1785568947986229116, 0.000000000000000000, 0.9839295885986321100 ) ) ;
#26331 = DIRECTION ( 'NONE',  ( -0.9998717552508122886, -0.01601477604151185785, 0.000000000000000000 ) ) ;
#26332 = B_SPLINE_CURVE_WITH_KNOTS ( 'NONE', 3,
 ( #192, #47402, #15942, #43299 ),
 .UNSPECIFIED., .F., .F.,
 ( 4, 4 ),
 ( 0.04410919144784399004, 0.04667637874967021927 ),
 .UNSPECIFIED. ) ;
#26333 = CARTESIAN_POINT ( 'NONE',  ( 1.363819533518803029, 3.346456692913386100, -1.102362204724405714 ) ) ;
#26334 = CARTESIAN_POINT ( 'NONE',  ( 1.015142113812069313, 0.000000000000000000, 0.5905511811023579360 ) ) ;
#26335 = LINE ( 'NONE', #22968, #18578 ) ;
#26336 = EDGE_CURVE ( 'NONE', #20150, #28628, #47114, .T. ) ;
#26337 = AXIS2_PLACEMENT_3D ( 'NONE', #14045, #10168, #22807 ) ;
#26338 = LINE ( 'NONE', #49530, #10251 ) ;
#26339 = EDGE_LOOP ( 'NONE', ( #29431, #23815, #34985, #30113 ) ) ;
#26340 = LINE ( 'NONE', #10844, #42376 ) ;
#26341 = CARTESIAN_POINT ( 'NONE',  ( -1.985260859929298016, 0.000000000000000000, -0.6299212598425177889 ) ) ;
#26342 = ORIENTED_EDGE ( 'NONE', *, *, #50750, .F. ) ;
#26343 = ORIENTED_EDGE ( 'NONE', *, *, #39082, .T. ) ;
#26344 = VECTOR ( 'NONE', #34890, 39.37007874015748143 ) ;
#26345 = DIRECTION ( 'NONE',  ( 5.782411586589357392E-17, 0.000000000000000000, 1.000000000000000000 ) ) ;
#26346 = EDGE_LOOP ( 'NONE', ( #2199, #18021, #27308, #46027 ) ) ;
#26347 = ADVANCED_FACE ( 'NONE', ( #34536 ), #50467, .F. ) ;
#26348 = VERTEX_POINT ( 'NONE', #50220 ) ;
#26349 = DIRECTION ( 'NONE',  ( 0.7071067811865483499, -0.000000000000000000, -0.7071067811865466846 ) ) ;
#26350 = CONICAL_SURFACE ( 'NONE', #17298, 2.244934639244524632, 1.554780866114618743 ) ;
#26351 = ADVANCED_FACE ( 'NONE', ( #38662 ), #26770, .F. ) ;
#26352 = ORIENTED_EDGE ( 'NONE', *, *, #12734, .T. ) ;
#26353 = LINE ( 'NONE', #26600, #11161 ) ;
#26354 = DIRECTION ( 'NONE',  ( 1.734723475976806848E-16, -0.000000000000000000, 1.000000000000000000 ) ) ;
#26355 = ORIENTED_EDGE ( 'NONE', *, *, #41851, .T. ) ;
#26356 = CARTESIAN_POINT ( 'NONE',  ( -2.122513613727505799, 1.575480814016643638, -0.4339716895473832436 ) ) ;
#26357 = ORIENTED_EDGE ( 'NONE', *, *, #262, .F. ) ;
#26358 = ORIENTED_EDGE ( 'NONE', *, *, #36863, .F. ) ;
#26359 = EDGE_CURVE ( 'NONE', #49030, #25746, #30911, .T. ) ;
#26360 = CARTESIAN_POINT ( 'NONE',  ( 2.603169958878716717, 0.9849481997864895089, 0.3029612783779465635 ) ) ;
#26361 = DIRECTION ( 'NONE',  ( -1.000000000000000000, 0.000000000000000000, 1.734723475976806848E-16 ) ) ;
#26362 = CARTESIAN_POINT ( 'NONE',  ( 0.1968503937007873017, 0.000000000000000000, 0.3149606299212576177 ) ) ;
#26363 = CARTESIAN_POINT ( 'NONE',  ( 0.8329809839909848579, 0.000000000000000000, -2.833254665166554442 ) ) ;
#26364 = EDGE_CURVE ( 'NONE', #22920, #44681, #29449, .T. ) ;
#26365 = ORIENTED_EDGE ( 'NONE', *, *, #35349, .F. ) ;
#26366 = DIRECTION ( 'NONE',  ( -5.782411586589357392E-17, 0.000000000000000000, -1.000000000000000000 ) ) ;
#26367 = CARTESIAN_POINT ( 'NONE',  ( 0.4696143004045478797, 3.267716535433071279, -0.6692913385826760875 ) ) ;
#26368 = AXIS2_PLACEMENT_3D ( 'NONE', #22993, #38745, #3367 ) ;
#26369 = CARTESIAN_POINT ( 'NONE',  ( 0.4696143004045484903, 3.267716535433071279, 2.047244094488179567 ) ) ;
#26370 = ORIENTED_EDGE ( 'NONE', *, *, #1770, .T. ) ;
#26371 = FACE_OUTER_BOUND ( 'NONE', #37770, .T. ) ;
#26372 = DIRECTION ( 'NONE',  ( -3.469446951953613696E-16, 0.000000000000000000, -1.000000000000000000 ) ) ;
#26373 = ORIENTED_EDGE ( 'NONE', *, *, #45912, .T. ) ;
#26374 = ORIENTED_EDGE ( 'NONE', *, *, #5388, .F. ) ;
#26375 = EDGE_CURVE ( 'NONE', #47793, #20337, #27017, .T. ) ;
#26376 = VECTOR ( 'NONE', #7711, 39.37007874015748143 ) ;
#26377 = CARTESIAN_POINT ( 'NONE',  ( 0.5905511811023627100, 0.000000000000000000, 2.165354330708661568 ) ) ;
#26378 = CARTESIAN_POINT ( 'NONE',  ( -1.091055626815042201, 3.267716535433071279, 0.3149606299212580063 ) ) ;
#26379 = EDGE_CURVE ( 'NONE', #23094, #20677, #26118, .T. ) ;
#26380 = EDGE_CURVE ( 'NONE', #1599, #30123, #7917, .T. ) ;
#26381 = CARTESIAN_POINT ( 'NONE',  ( -1.091055626815042201, 0.000000000000000000, 0.3149606299212580063 ) ) ;
#26382 = ORIENTED_EDGE ( 'NONE', *, *, #24551, .T. ) ;
#26383 = ORIENTED_EDGE ( 'NONE', *, *, #31717, .T. ) ;
#26384 = CARTESIAN_POINT ( 'NONE',  ( -0.5455278134075208785, 3.346456692913386100, 1.574803149606291974 ) ) ;
#26385 = CARTESIAN_POINT ( 'NONE',  ( -0.8942052331142548161, 3.267716535433071279, 3.102397620449221988E-16 ) ) ;
#26386 = CIRCLE ( 'NONE', #50256, 2.244934639244525076 ) ;
#26387 = ORIENTED_EDGE ( 'NONE', *, *, #24398, .F. ) ;
#26388 = CARTESIAN_POINT ( 'NONE',  ( 0.4696143004045484903, 0.000000000000000000, 2.047244094488179567 ) ) ;
#26389 = DIRECTION ( 'NONE',  ( -0.000000000000000000, 1.000000000000000000, -0.000000000000000000 ) ) ;
#26390 = EDGE_CURVE ( 'NONE', #17201, #17605, #40697, .T. ) ;
#26391 = CARTESIAN_POINT ( 'NONE',  ( -2.339241080213612545, 1.682800407567106360, 1.802537235681883843 ) ) ;
#26392 = CARTESIAN_POINT ( 'NONE',  ( 1.681836973804981428, 0.5249316475426862860, 0.8491494810026807283 ) ) ;
#26393 = DIRECTION ( 'NONE',  ( 0.5773502691896261751, 0.5773502691896261751, -0.5773502691896248429 ) ) ;
#26394 = EDGE_LOOP ( 'NONE', ( #17173, #12797, #45391, #36264 ) ) ;
#26395 = LINE ( 'NONE', #31032, #30861 ) ;
#26396 = CARTESIAN_POINT ( 'NONE',  ( -2.182111253630085290, 0.000000000000000000, 0.4330708661417290162 ) ) ;
#26397 = PLANE ( 'NONE',  #14177 ) ;
#26398 = ORIENTED_EDGE ( 'NONE', *, *, #36729, .T. ) ;
#26399 = DIRECTION ( 'NONE',  ( 0.000000000000000000, 0.000000000000000000, 1.000000000000000000 ) ) ;
#26400 = DIRECTION ( 'NONE',  ( 8.881784197001252323E-16, 0.000000000000000000, 1.000000000000000000 ) ) ;
#26401 = CARTESIAN_POINT ( 'NONE',  ( 0.8182917201112824834, 3.267716535433071279, 1.220472440944875281 ) ) ;
#26402 = VERTEX_POINT ( 'NONE', #23923 ) ;
#26403 = EDGE_CURVE ( 'NONE', #272, #18980, #32713, .T. ) ;
#26404 = CARTESIAN_POINT ( 'NONE',  ( -2.455258355620455024, 1.565786800488158770, -1.640348343447587398 ) ) ;
#26405 = VERTEX_POINT ( 'NONE', #21074 ) ;
#26406 = CARTESIAN_POINT ( 'NONE',  ( -1.521361932310741016, 3.267716535433071279, -1.456692913385822186 ) ) ;
#26407 = EDGE_LOOP ( 'NONE', ( #46545, #1197, #19856, #28578 ) ) ;
#26408 = DIRECTION ( 'NONE',  ( -3.469446951953613696E-16, 0.000000000000000000, -1.000000000000000000 ) ) ;
#26409 = EDGE_CURVE ( 'NONE', #27965, #42803, #13080, .T. ) ;
#26410 = VECTOR ( 'NONE', #37074, 39.37007874015748143 ) ;
#26411 = DIRECTION ( 'NONE',  ( -0.000000000000000000, 1.000000000000000000, -0.000000000000000000 ) ) ;
#26412 = FACE_OUTER_BOUND ( 'NONE', #16840, .T. ) ;
#26413 = CARTESIAN_POINT ( 'NONE',  ( 1.481515513156649977, 0.000000000000000000, -0.9189724476880527515 ) ) ;
#26414 = CIRCLE ( 'NONE', #45337, 2.244934639244525076 ) ;
#26415 = EDGE_CURVE ( 'NONE', #24633, #16952, #39669, .T. ) ;
#26416 = EDGE_CURVE ( 'NONE', #19157, #19280, #4300, .T. ) ;
#26417 = ORIENTED_EDGE ( 'NONE', *, *, #224, .F. ) ;
#26418 = ORIENTED_EDGE ( 'NONE', *, *, #41745, .F. ) ;
#26419 = FACE_OUTER_BOUND ( 'NONE', #31447, .T. ) ;
#26420 = LINE ( 'NONE', #46271, #27128 ) ;
#26421 = EDGE_LOOP ( 'NONE', ( #9576, #22311, #3134, #8704 ) ) ;
#26422 = CARTESIAN_POINT ( 'NONE',  ( 0.4696143004045478797, 3.267716535433071279, -1.299212598425193210 ) ) ;
#26423 = PLANE ( 'NONE',  #39271 ) ;
#26424 = VECTOR ( 'NONE', #34056, 39.37007874015748143 ) ;
#26425 = DIRECTION ( 'NONE',  ( -0.01601477604151182663, 0.9998717552508123996, -0.000000000000000000 ) ) ;
#26426 = ORIENTED_EDGE ( 'NONE', *, *, #32373, .T. ) ;
#26427 = ORIENTED_EDGE ( 'NONE', *, *, #25483, .T. ) ;
#26428 = CARTESIAN_POINT ( 'NONE',  ( 1.464430631143598172, 0.03384846671821301750, -1.332052510296074965 ) ) ;
#26429 = DIRECTION ( 'NONE',  ( 0.000000000000000000, -1.000000000000000000, 0.000000000000000000 ) ) ;
#26430 = CARTESIAN_POINT ( 'NONE',  ( -1.363819533518803473, 3.346456692913386100, -0.4724409448818886470 ) ) ;
#26431 = VERTEX_POINT ( 'NONE', #36318 ) ;
#26432 = LINE ( 'NONE', #9936, #5885 ) ;
#26433 = FACE_BOUND ( 'NONE', #14012, .T. ) ;
#26434 = EDGE_LOOP ( 'NONE', ( #11132, #38537, #22802, #6424 ) ) ;
#26435 = DIRECTION ( 'NONE',  ( -0.000000000000000000, 1.000000000000000000, -0.000000000000000000 ) ) ;
#26436 = VERTEX_POINT ( 'NONE', #44302 ) ;
#26437 = ORIENTED_EDGE ( 'NONE', *, *, #35226, .T. ) ;
#26438 = DIRECTION ( 'NONE',  ( 0.01601477604151182663, -0.9998717552508123996, 0.000000000000000000 ) ) ;
#26439 = CARTESIAN_POINT ( 'NONE',  ( -0.5455278134075214336, 3.346456692913386100, -8.878505979408855953E-16 ) ) ;
#26440 = ADVANCED_FACE ( 'NONE', ( #28812 ), #20031, .T. ) ;
#26441 = CARTESIAN_POINT ( 'NONE',  ( -1.775400203342670347, 1.552775173289138166, -2.359903268218729089 ) ) ;
#26442 = LINE ( 'NONE', #38083, #9624 ) ;
#26443 = EDGE_CURVE ( 'NONE', #44444, #23181, #5322, .T. ) ;
#26444 = EDGE_CURVE ( 'NONE', #16487, #9349, #25318, .T. ) ;
#26445 = DIRECTION ( 'NONE',  ( -3.469446951953613696E-16, 0.000000000000000000, -1.000000000000000000 ) ) ;
#26446 = ORIENTED_EDGE ( 'NONE', *, *, #45500, .F. ) ;
#26447 = EDGE_CURVE ( 'NONE', #15782, #16783, #36389, .T. ) ;
#26448 = ORIENTED_EDGE ( 'NONE', *, *, #29716, .T. ) ;
#26449 = FACE_OUTER_BOUND ( 'NONE', #16209, .T. ) ;
#26450 = CARTESIAN_POINT ( 'NONE',  ( -1.166969139818015533, 3.267716535433071279, 4.048737525165544183E-16 ) ) ;
#26451 = VECTOR ( 'NONE', #30717, 39.37007874015748143 ) ;
#26452 = VECTOR ( 'NONE', #23410, 39.37007874015748143 ) ;
#26453 = FACE_OUTER_BOUND ( 'NONE', #1331, .T. ) ;
#26454 = CARTESIAN_POINT ( 'NONE',  ( 0.07982360342473591996, 1.709180471932028711, 0.000000000000000000 ) ) ;
#26455 = CARTESIAN_POINT ( 'NONE',  ( 1.485598995959307889, 5.905511811023623991, 1.625606721701626567 ) ) ;
#26456 = EDGE_LOOP ( 'NONE', ( #43261, #51022, #38976, #27266 ) ) ;
#26457 = DIRECTION ( 'NONE',  ( -0.9998717552508122886, -0.01601477604151181275, 0.000000000000000000 ) ) ;
#26458 = VECTOR ( 'NONE', #29861, 39.37007874015748143 ) ;
#26459 = CARTESIAN_POINT ( 'NONE',  ( -1.439733046521776361, 3.267716535433071279, 0.4330708661417290162 ) ) ;
#26460 = ORIENTED_EDGE ( 'NONE', *, *, #38094, .T. ) ;
#26461 = CARTESIAN_POINT ( 'NONE',  ( -1.833791099076586217, 1.574803149606302854, -1.151507526013721083 ) ) ;
#26462 = CARTESIAN_POINT ( 'NONE',  ( 1.519644562253804621, 0.03439821511908755514, 1.274821374926282669 ) ) ;
#26463 = VERTEX_POINT ( 'NONE', #24698 ) ;
#26464 = DIRECTION ( 'NONE',  ( 0.000000000000000000, 1.000000000000000000, 0.000000000000000000 ) ) ;
#26465 = LINE ( 'NONE', #50168, #46432 ) ;
#26466 = DIRECTION ( 'NONE',  ( -0.000000000000000000, -1.000000000000000000, 0.000000000000000000 ) ) ;
#26467 = VERTEX_POINT ( 'NONE', #44550 ) ;
#26468 = CARTESIAN_POINT ( 'NONE',  ( 0.000000000000000000, 2.755905511811024056, 0.000000000000000000 ) ) ;
#26469 = ORIENTED_EDGE ( 'NONE', *, *, #37763, .F. ) ;
#26470 = FACE_BOUND ( 'NONE', #6187, .T. ) ;
#26471 = CARTESIAN_POINT ( 'NONE',  ( -0.8182917201112819283, 3.346456692913386100, -0.6692913385826760875 ) ) ;
#26472 = FACE_OUTER_BOUND ( 'NONE', #31916, .T. ) ;
#26473 = EDGE_CURVE ( 'NONE', #19997, #26534, #32970, .T. ) ;
#26474 = ADVANCED_FACE ( 'NONE', ( #32193 ), #12048, .T. ) ;
#26475 = EDGE_LOOP ( 'NONE', ( #11969, #45118, #37540, #19447 ) ) ;
#26476 = VERTEX_POINT ( 'NONE', #5069 ) ;
#26477 = CARTESIAN_POINT ( 'NONE',  ( 1.636583440222563857, 3.346456692913386100, 0.3149606299212576177 ) ) ;
#26478 = DIRECTION ( 'NONE',  ( 1.734723475976806848E-16, 0.000000000000000000, 1.000000000000000000 ) ) ;
#26479 = CARTESIAN_POINT ( 'NONE',  ( 2.793030215715258446, 1.451280567205322836, 0.9592557174602683867 ) ) ;
#26480 = CARTESIAN_POINT ( 'NONE',  ( 1.091055626815042645, 3.346456692913386100, 0.6299212598425161236 ) ) ;
#26481 = VECTOR ( 'NONE', #30451, 39.37007874015748143 ) ;
#26482 = VECTOR ( 'NONE', #40693, 39.37007874015748143 ) ;
#26483 = LINE ( 'NONE', #22118, #19046 ) ;
#26484 = AXIS2_PLACEMENT_3D ( 'NONE', #29867, #1988, #25736 ) ;
#26485 = ORIENTED_EDGE ( 'NONE', *, *, #7655, .T. ) ;
#26486 = ORIENTED_EDGE ( 'NONE', *, *, #24549, .F. ) ;
#26487 = CARTESIAN_POINT ( 'NONE',  ( 0.000000000000000000, 3.267716535433071279, -0.4724409448818886470 ) ) ;
#26488 = DIRECTION ( 'NONE',  ( -0.9998717552508122886, -0.01601477604151181275, 0.000000000000000000 ) ) ;
#26489 = B_SPLINE_CURVE_WITH_KNOTS ( 'NONE', 3,
 ( #23625, #12008, #4014, #8136 ),
 .UNSPECIFIED., .F., .F.,
 ( 4, 4 ),
 ( 0.0003090509669333037202, 0.002809230294771062394 ),
 .UNSPECIFIED. ) ;
#26490 = EDGE_LOOP ( 'NONE', ( #36459, #18094, #38973, #24790 ) ) ;
#26491 = CARTESIAN_POINT ( 'NONE',  ( -1.062992125984250968, 0.4724409448818890911, 1.181102362204724088 ) ) ;
#26492 = VERTEX_POINT ( 'NONE', #43779 ) ;
#26493 = VECTOR ( 'NONE', #28124, 39.37007874015748143 ) ;
#26494 = ORIENTED_EDGE ( 'NONE', *, *, #37248, .F. ) ;
#26495 = EDGE_CURVE ( 'NONE', #48519, #14792, #43416, .T. ) ;
#26496 = VECTOR ( 'NONE', #49659, 39.37007874015748143 ) ;
#26497 = EDGE_CURVE ( 'NONE', #26476, #7771, #20298, .T. ) ;
#26498 = VERTEX_POINT ( 'NONE', #12557 ) ;
#26499 = ORIENTED_EDGE ( 'NONE', *, *, #16958, .T. ) ;
#26500 = CARTESIAN_POINT ( 'NONE',  ( 1.319349709118413205, 0.000000000000000000, 1.584915398547334764 ) ) ;
#26501 = ADVANCED_FACE ( 'NONE', ( #20816 ), #9197, .F. ) ;
#26502 = EDGE_CURVE ( 'NONE', #43652, #35947, #24945, .T. ) ;
#26503 = CARTESIAN_POINT ( 'NONE',  ( -2.813306909032236014, 1.576974190620015648, 0.8968504722502548265 ) ) ;
#26504 = EDGE_CURVE ( 'NONE', #272, #43925, #16696, .T. ) ;
#26505 = DIRECTION ( 'NONE',  ( -0.000000000000000000, 1.000000000000000000, -0.000000000000000000 ) ) ;
#26506 = CARTESIAN_POINT ( 'NONE',  ( 2.277873973731426194, 1.754757658573260048, 1.879489153247668076 ) ) ;
#26507 = CARTESIAN_POINT ( 'NONE',  ( -0.5443978225238782498, 1.600757226547528500, -2.157565353623420723 ) ) ;
#26508 = PLANE ( 'NONE',  #17926 ) ;
#26509 = ORIENTED_EDGE ( 'NONE', *, *, #49825, .F. ) ;
#26510 = CARTESIAN_POINT ( 'NONE',  ( -2.082617625631827174, 3.346456692913386100, 0.3149606299212578953 ) ) ;
#26511 = DIRECTION ( 'NONE',  ( -3.469446951953613696E-16, 0.000000000000000000, -1.000000000000000000 ) ) ;
#26512 = B_SPLINE_CURVE_WITH_KNOTS ( 'NONE', 3,
 ( #19933, #23071, #27435, #70 ),
 .UNSPECIFIED., .F., .F.,
 ( 4, 4 ),
 ( 0.01148951601955449514, 0.03073652705649548150 ),
 .UNSPECIFIED. ) ;
#26513 = DIRECTION ( 'NONE',  ( 0.9998717552508121775, 0.01601477604151182663, 0.000000000000000000 ) ) ;
#26514 = PLANE ( 'NONE',  #48703 ) ;
#26515 = VECTOR ( 'NONE', #26646, 39.37007874015748143 ) ;
#26516 = VERTEX_POINT ( 'NONE', #33729 ) ;
#26517 = CONICAL_SURFACE ( 'NONE', #4263, 3.033577403570480779, 1.554780866114618743 ) ;
#26518 = CARTESIAN_POINT ( 'NONE',  ( -0.6214413264104939882, 3.346456692913386100, 0.4724409448818872592 ) ) ;
#26519 = CARTESIAN_POINT ( 'NONE',  ( 0.3467207527347881402, 5.905511811023623991, 2.186201806782071433 ) ) ;
#26520 = EDGE_LOOP ( 'NONE', ( #663, #11268, #254, #33539, #31228, #34800, #19665, #9945, #34826, #17855, #44718, #18369 ) ) ;
#26521 = DIRECTION ( 'NONE',  ( 0.000000000000000000, -0.000000000000000000, -1.000000000000000000 ) ) ;
#26522 = LINE ( 'NONE', #45112, #41611 ) ;
#26523 = AXIS2_PLACEMENT_3D ( 'NONE', #22613, #38865, #50672 ) ;
#26524 = VERTEX_POINT ( 'NONE', #10218 ) ;
#26525 = AXIS2_PLACEMENT_3D ( 'NONE', #41243, #16983, #13361 ) ;
#26526 = CARTESIAN_POINT ( 'NONE',  ( 2.222091332265985208, 1.743492810207595500, 0.6702560524809636489 ) ) ;
#26527 = VERTEX_POINT ( 'NONE', #45055 ) ;
#26528 = FACE_OUTER_BOUND ( 'NONE', #17938, .T. ) ;
#26529 = CARTESIAN_POINT ( 'NONE',  ( -0.2727639067037606613, 3.267716535433071279, 4.731699523581610974E-17 ) ) ;
#26530 = AXIS2_PLACEMENT_3D ( 'NONE', #27402, #11915, #19396 ) ;
#26531 = DIRECTION ( 'NONE',  ( 0.000000000000000000, 0.000000000000000000, -1.000000000000000000 ) ) ;
#26532 = DIRECTION ( 'NONE',  ( -2.200518442539857142E-16, 0.7071067811865483499, 0.7071067811865465735 ) ) ;
#26533 = LINE ( 'NONE', #22670, #45855 ) ;
#26534 = VERTEX_POINT ( 'NONE', #5580 ) ;
#26535 = B_SPLINE_CURVE_WITH_KNOTS ( 'NONE', 3,
 ( #20949, #33354, #17341, #41093 ),
 .UNSPECIFIED., .F., .F.,
 ( 4, 4 ),
 ( 0.1211775127643062722, 0.1625894504277921315 ),
 .UNSPECIFIED. ) ;
#26536 = DIRECTION ( 'NONE',  ( 0.5407162030609373726, -0.6444004775717706579, -0.5407162030609372616 ) ) ;
#26537 = EDGE_CURVE ( 'NONE', #25449, #15789, #12074, .T. ) ;
#26538 = VERTEX_POINT ( 'NONE', #41212 ) ;
#26539 = EDGE_LOOP ( 'NONE', ( #40735, #7259, #35073, #20852 ) ) ;
#26540 = EDGE_CURVE ( 'NONE', #18808, #22242, #25199, .T. ) ;
#26541 = DIRECTION ( 'NONE',  ( 0.000000000000000000, 1.160734090543304660E-16, -1.000000000000000000 ) ) ;
#26542 = ORIENTED_EDGE ( 'NONE', *, *, #41835, .T. ) ;
#26543 = CARTESIAN_POINT ( 'NONE',  ( 1.355960331127249452, 0.04963785175798203497, -1.364517356352728861 ) ) ;
#26544 = LINE ( 'NONE', #10799, #19401 ) ;
#26545 = ORIENTED_EDGE ( 'NONE', *, *, #37733, .F. ) ;
#26546 = EDGE_CURVE ( 'NONE', #49624, #48094, #33975, .T. ) ;
#26547 = CARTESIAN_POINT ( 'NONE',  ( 1.037524086854322292, 5.905511811023623991, 2.764473043227584803 ) ) ;
#26548 = DIRECTION ( 'NONE',  ( -1.000000000000000000, 0.000000000000000000, 0.000000000000000000 ) ) ;
#26549 = CARTESIAN_POINT ( 'NONE',  ( -1.636583440222563635, 3.267716535433071279, 2.839019714148966584E-16 ) ) ;
#26550 = ORIENTED_EDGE ( 'NONE', *, *, #50886, .F. ) ;
#26551 = ORIENTED_EDGE ( 'NONE', *, *, #37237, .T. ) ;
#26552 = LINE ( 'NONE', #26306, #40543 ) ;
#26553 = FACE_BOUND ( 'NONE', #18692, .T. ) ;
#26554 = ORIENTED_EDGE ( 'NONE', *, *, #47745, .T. ) ;
#26555 = AXIS2_PLACEMENT_3D ( 'NONE', #28450, #8845, #1351 ) ;
#26556 = DIRECTION ( 'NONE',  ( 0.000000000000000000, 0.000000000000000000, -1.000000000000000000 ) ) ;
#26557 = EDGE_CURVE ( 'NONE', #5044, #8046, #25705, .T. ) ;
#26558 = ORIENTED_EDGE ( 'NONE', *, *, #1036, .F. ) ;
#26559 = ORIENTED_EDGE ( 'NONE', *, *, #49603, .F. ) ;
#26560 = DIRECTION ( 'NONE',  ( -0.000000000000000000, 1.000000000000000000, -0.000000000000000000 ) ) ;
#26561 = VECTOR ( 'NONE', #2557, 39.37007874015748143 ) ;
#26562 = FACE_OUTER_BOUND ( 'NONE', #947, .T. ) ;
#26563 = ADVANCED_FACE ( 'NONE', ( #49413 ), #49149, .T. ) ;
#26564 = ORIENTED_EDGE ( 'NONE', *, *, #22316, .T. ) ;
#26565 = AXIS2_PLACEMENT_3D ( 'NONE', #29036, #48113, #1166 ) ;
#26566 = LINE ( 'NONE', #46663, #37790 ) ;
#26567 = ORIENTED_EDGE ( 'NONE', *, *, #46831, .T. ) ;
#26568 = CARTESIAN_POINT ( 'NONE',  ( 1.091055626815042645, 3.346456692913386100, 0.9448818897637746295 ) ) ;
#26569 = CIRCLE ( 'NONE', #25733, 2.244934639244525076 ) ;
#26570 = DIRECTION ( 'NONE',  ( 0.000000000000000000, 0.000000000000000000, 1.000000000000000000 ) ) ;
#26571 = LINE ( 'NONE', #35342, #14849 ) ;
#26572 = EDGE_LOOP ( 'NONE', ( #9670, #11183, #13064, #17477 ) ) ;
#26573 = ORIENTED_EDGE ( 'NONE', *, *, #2252, .F. ) ;
#26574 = CARTESIAN_POINT ( 'NONE',  ( -1.909347346926324462, 3.346456692913386100, 0.1574803149606286423 ) ) ;
#26575 = LINE ( 'NONE', #41569, #11464 ) ;
#26576 = DIRECTION ( 'NONE',  ( -3.469446951953613696E-16, 0.000000000000000000, -1.000000000000000000 ) ) ;
#26577 = ADVANCED_FACE ( 'NONE', ( #6605 ), #4663, .T. ) ;
#26578 = DIRECTION ( 'NONE',  ( 0.5407162030609374836, -0.6444004775717706579, -0.5407162030609372616 ) ) ;
#26579 = CARTESIAN_POINT ( 'NONE',  ( -2.889674983507169337, 1.575792602931942232, -0.6090712660038034576 ) ) ;
#26580 = CARTESIAN_POINT ( 'NONE',  ( -1.091055626815042201, 3.346456692913386100, 0.4330708661417290162 ) ) ;
#26581 = CARTESIAN_POINT ( 'NONE',  ( 0.5455278134075212115, 0.000000000000000000, 0.9448818897637746295 ) ) ;
#26582 = ORIENTED_EDGE ( 'NONE', *, *, #17468, .F. ) ;
#26583 = CARTESIAN_POINT ( 'NONE',  ( 0.000000000000000000, 3.267716535433071279, -1.456692913385822630 ) ) ;
#26584 = DIRECTION ( 'NONE',  ( -1.000000000000000000, -0.000000000000000000, -0.000000000000000000 ) ) ;
#26585 = ORIENTED_EDGE ( 'NONE', *, *, #23677, .F. ) ;
#26586 = VERTEX_POINT ( 'NONE', #37595 ) ;
#26587 = DIRECTION ( 'NONE',  ( 1.734723475976806848E-16, 0.000000000000000000, 1.000000000000000000 ) ) ;
#26588 = AXIS2_PLACEMENT_3D ( 'NONE', #13686, #2569, #22199 ) ;
#26589 = LINE ( 'NONE', #14216, #49221 ) ;
#26590 = ORIENTED_EDGE ( 'NONE', *, *, #38815, .F. ) ;
#26591 = VECTOR ( 'NONE', #12332, 39.37007874015748143 ) ;
#26592 = EDGE_CURVE ( 'NONE', #33429, #5817, #33216, .T. ) ;
#26593 = ORIENTED_EDGE ( 'NONE', *, *, #33689, .F. ) ;
#26594 = CARTESIAN_POINT ( 'NONE',  ( -1.091055626815042645, 0.000000000000000000, 2.204724409448808764 ) ) ;
#26595 = VECTOR ( 'NONE', #13490, 39.37007874015748143 ) ;
#26596 = ORIENTED_EDGE ( 'NONE', *, *, #1904, .T. ) ;
#26597 = EDGE_CURVE ( 'NONE', #44234, #27935, #21332, .T. ) ;
#26598 = VECTOR ( 'NONE', #1627, 39.37007874015748143 ) ;
#26599 = AXIS2_PLACEMENT_3D ( 'NONE', #13193, #17321, #12668 ) ;
#26600 = CARTESIAN_POINT ( 'NONE',  ( 0.04921259842519603439, 6.692913385826772199, 2.164795024401847456 ) ) ;
#26601 = CARTESIAN_POINT ( 'NONE',  ( 0.8182917201112819283, 3.267716535433071279, -1.419509857074483292E-16 ) ) ;
#26602 = ADVANCED_FACE ( 'NONE', ( #1962 ), #14343, .F. ) ;
#26603 = EDGE_CURVE ( 'NONE', #16416, #38863, #45590, .T. ) ;
#26604 = EDGE_LOOP ( 'NONE', ( #21367, #26903, #30415, #49518 ) ) ;
#26605 = APPLICATION_CONTEXT ( 'automotive_design' ) ;
#26606 = DIRECTION ( 'NONE',  ( -0.000000000000000000, -1.000000000000000000, -0.000000000000000000 ) ) ;
#26607 = ORIENTED_EDGE ( 'NONE', *, *, #27974, .F. ) ;
#26608 = EDGE_LOOP ( 'NONE', ( #34669, #45441, #49331, #29684 ) ) ;
#26609 = CARTESIAN_POINT ( 'NONE',  ( 1.944213194762889119, 0.05905979794000976862, 0.2136995197171435157 ) ) ;
#26610 = CARTESIAN_POINT ( 'NONE',  ( 0.9838852166858921278, 0.000000000000000000, 1.929635236160317735 ) ) ;
#26611 = FACE_OUTER_BOUND ( 'NONE', #30008, .T. ) ;
#26612 = CYLINDRICAL_SURFACE ( 'NONE', #39205, 2.165354330708661568 ) ;
#26613 = ORIENTED_EDGE ( 'NONE', *, *, #29197, .F. ) ;
#26614 = CARTESIAN_POINT ( 'NONE',  ( 0.3595914698493179462, 0.000000000000000000, 1.705899337635486290 ) ) ;
#26615 = ADVANCED_FACE ( 'NONE', ( #29586 ), #33583, .T. ) ;
#26616 = FACE_OUTER_BOUND ( 'NONE', #36768, .T. ) ;
#26617 = PLANE ( 'NONE',  #5557 ) ;
#26618 = VERTEX_POINT ( 'NONE', #45303 ) ;
#26619 = CARTESIAN_POINT ( 'NONE',  ( -1.363819533518803473, 0.000000000000000000, -1.417322834645664109 ) ) ;
#26620 = EDGE_CURVE ( 'NONE', #46385, #27405, #18217, .T. ) ;
#26621 = ORIENTED_EDGE ( 'NONE', *, *, #20433, .F. ) ;
#26622 = EDGE_LOOP ( 'NONE', ( #22814, #39368, #21203, #16794 ) ) ;
#26623 =( LENGTH_UNIT ( ) NAMED_UNIT ( * ) SI_UNIT ( $, .METRE. ) );
#26624 = DIRECTION ( 'NONE',  ( 0.000000000000000000, 0.000000000000000000, -1.000000000000000000 ) ) ;
#26625 = CARTESIAN_POINT ( 'NONE',  ( -0.6214413264104945434, 0.000000000000000000, -0.1574803149606301411 ) ) ;
#26626 = EDGE_CURVE ( 'NONE', #1213, #27411, #5833, .T. ) ;
#26627 = DIRECTION ( 'NONE',  ( 1.000000000000000000, -0.000000000000000000, 0.000000000000000000 ) ) ;
#26628 = DIRECTION ( 'NONE',  ( -0.2225209339563041788, 0.000000000000000000, -0.9749279121818259508 ) ) ;
#26629 = VERTEX_POINT ( 'NONE', #41712 ) ;
#26630 = VERTEX_POINT ( 'NONE', #48645 ) ;
#26631 = VECTOR ( 'NONE', #28261, 39.37007874015748143 ) ;
#26632 = DIRECTION ( 'NONE',  ( 1.734723475976806848E-16, 0.000000000000000000, 1.000000000000000000 ) ) ;
#26633 = LINE ( 'NONE', #22771, #2066 ) ;
#26634 = ORIENTED_EDGE ( 'NONE', *, *, #21701, .T. ) ;
#26635 = CARTESIAN_POINT ( 'NONE',  ( -1.252056778656947422, 1.687847970117562602, -1.807033786809818077 ) ) ;
#26636 = ADVANCED_FACE ( 'NONE', ( #13589 ), #2221, .F. ) ;
#26637 = LINE ( 'NONE', #38528, #3670 ) ;
#26638 = AXIS2_PLACEMENT_3D ( 'NONE', #42625, #38762, #3139 ) ;
#26639 = AXIS2_PLACEMENT_3D ( 'NONE', #20085, #32504, #13131 ) ;
#26640 = DIRECTION ( 'NONE',  ( -0.000000000000000000, 1.000000000000000000, -0.000000000000000000 ) ) ;
#26641 = LINE ( 'NONE', #42135, #12035 ) ;
#26642 = DIRECTION ( 'NONE',  ( 0.000000000000000000, 0.000000000000000000, -1.000000000000000000 ) ) ;
#26643 = VERTEX_POINT ( 'NONE', #13838 ) ;
#26644 = CARTESIAN_POINT ( 'NONE',  ( -0.5455278134075214336, 0.000000000000000000, -1.889763779527552146 ) ) ;
#26645 = EDGE_CURVE ( 'NONE', #35815, #25253, #6084, .T. ) ;
#26646 = DIRECTION ( 'NONE',  ( -3.469446951953613696E-16, 0.000000000000000000, -1.000000000000000000 ) ) ;
#26647 = EDGE_CURVE ( 'NONE', #42204, #7708, #11229, .T. ) ;
#26648 = ORIENTED_EDGE ( 'NONE', *, *, #1655, .F. ) ;
#26649 = CARTESIAN_POINT ( 'NONE',  ( -2.339241080213612545, 1.564176246289736616, 1.802537235681883843 ) ) ;
#26650 = DIRECTION ( 'NONE',  ( -1.000000000000000000, 0.000000000000000000, 1.734723475976806848E-16 ) ) ;
#26651 = CARTESIAN_POINT ( 'NONE',  ( 1.735586374879371174, 5.905511811023623991, -2.388829707800026014 ) ) ;
#26652 = ORIENTED_EDGE ( 'NONE', *, *, #31505, .F. ) ;
#26653 = DIRECTION ( 'NONE',  ( -0.000000000000000000, 1.000000000000000000, -0.000000000000000000 ) ) ;
#26654 = ORIENTED_EDGE ( 'NONE', *, *, #11771, .F. ) ;
#26655 = CARTESIAN_POINT ( 'NONE',  ( 1.015142113812069313, 0.000000000000000000, 0.4724409448818868706 ) ) ;
#26656 = ORIENTED_EDGE ( 'NONE', *, *, #31159, .T. ) ;
#26657 = CARTESIAN_POINT ( 'NONE',  ( 0.08139965876239094178, 1.610780518492231694, 0.000000000000000000 ) ) ;
#26658 = EDGE_LOOP ( 'NONE', ( #41411, #6482, #46230, #11269 ) ) ;
#26659 = EDGE_CURVE ( 'NONE', #16076, #29695, #50490, .T. ) ;
#26660 = CARTESIAN_POINT ( 'NONE',  ( 0.1067246931122726866, 0.02962905676920215767, 0.000000000000000000 ) ) ;
#26661 = DIRECTION ( 'NONE',  ( -0.000000000000000000, 1.000000000000000000, -0.000000000000000000 ) ) ;
#26662 = CARTESIAN_POINT ( 'NONE',  ( -2.010517631316633747, 5.905511811023623991, 0.8058170502102095512 ) ) ;
#26663 = EDGE_CURVE ( 'NONE', #37648, #43368, #46810, .T. ) ;
#26664 = ORIENTED_EDGE ( 'NONE', *, *, #33205, .T. ) ;
#26665 = AXIS2_PLACEMENT_3D ( 'NONE', #46216, #26116, #41866 ) ;
#26666 = ORIENTED_EDGE ( 'NONE', *, *, #31680, .T. ) ;
#26667 = VERTEX_POINT ( 'NONE', #34979 ) ;
#26668 = DIRECTION ( 'NONE',  ( 1.000000000000000000, 0.000000000000000000, 0.000000000000000000 ) ) ;
#26669 = DIRECTION ( 'NONE',  ( 1.000000000000000000, 0.000000000000000000, 0.000000000000000000 ) ) ;
#26670 = ORIENTED_EDGE ( 'NONE', *, *, #164, .F. ) ;
#26671 = AXIS2_PLACEMENT_3D ( 'NONE', #31610, #3485, #42211 ) ;
#26672 = DIRECTION ( 'NONE',  ( 0.000000000000000000, 0.000000000000000000, 1.000000000000000000 ) ) ;
#26673 = CARTESIAN_POINT ( 'NONE',  ( -2.275362778309363065, 1.679744148766246337, -1.442986439457680126 ) ) ;
#26674 = CARTESIAN_POINT ( 'NONE',  ( -0.8182917201112814842, 3.346456692913386100, 1.535433070866133898 ) ) ;
#26675 = CONICAL_SURFACE ( 'NONE', #6889, 2.244934639244524632, 1.554780866114618743 ) ;
#26676 = VECTOR ( 'NONE', #10521, 39.37007874015748143 ) ;
#26677 = EDGE_LOOP ( 'NONE', ( #37419, #1993, #22105, #33857 ) ) ;
#26678 = ORIENTED_EDGE ( 'NONE', *, *, #28280, .F. ) ;
#26679 = CARTESIAN_POINT ( 'NONE',  ( 2.153610746787201435, 1.643970771453353130, -0.8669779829368272628 ) ) ;
#26680 = DIRECTION ( 'NONE',  ( -3.469446951953613696E-16, 0.000000000000000000, -1.000000000000000000 ) ) ;
#26681 = PLANE ( 'NONE',  #30503 ) ;
#26682 = EDGE_LOOP ( 'NONE', ( #29208, #25474, #14926, #26446 ) ) ;
#26683 = LINE ( 'NONE', #11951, #37303 ) ;
#26684 = FACE_BOUND ( 'NONE', #3015, .T. ) ;
#26685 = VECTOR ( 'NONE', #33903, 39.37007874015748143 ) ;
#26686 = ORIENTED_EDGE ( 'NONE', *, *, #50594, .T. ) ;
#26687 = CARTESIAN_POINT ( 'NONE',  ( 2.182111253630085290, 3.346456692913386100, -0.1968503937007886062 ) ) ;
#26688 = VERTEX_POINT ( 'NONE', #30854 ) ;
#26689 = ORIENTED_EDGE ( 'NONE', *, *, #42330, .F. ) ;
#26690 = CARTESIAN_POINT ( 'NONE',  ( 0.7423782071083084855, 3.346456692913386100, -1.889763779527552812 ) ) ;
#26691 = CARTESIAN_POINT ( 'NONE',  ( 0.000000000000000000, 3.267716535433071279, -1.141732283464564013 ) ) ;
#26692 = CARTESIAN_POINT ( 'NONE',  ( -1.738757879605812073, 7.027592017269983715E-05, -0.1273499085982673085 ) ) ;
#26693 = EDGE_CURVE ( 'NONE', #42860, #28536, #27217, .T. ) ;
#26694 = CARTESIAN_POINT ( 'NONE',  ( 0.4696143004045479352, 0.000000000000000000, 0.4724409448818868706 ) ) ;
#26695 = DIRECTION ( 'NONE',  ( -0.000000000000000000, 1.000000000000000000, -0.000000000000000000 ) ) ;
#26696 = ORIENTED_EDGE ( 'NONE', *, *, #9069, .F. ) ;
#26697 = EDGE_LOOP ( 'NONE', ( #21258, #40566, #21490, #7432 ) ) ;
#26698 = DIRECTION ( 'NONE',  ( -0.000000000000000000, 1.000000000000000000, -0.000000000000000000 ) ) ;
#26699 = EDGE_CURVE ( 'NONE', #13594, #30262, #14855, .T. ) ;
#26700 = CARTESIAN_POINT ( 'NONE',  ( -1.439733046521776361, 0.000000000000000000, 1.062992125984246083 ) ) ;
#26701 = EDGE_CURVE ( 'NONE', #43417, #47601, #50658, .T. ) ;
#26702 = EDGE_CURVE ( 'NONE', #19788, #13030, #50166, .T. ) ;
#26703 = AXIS2_PLACEMENT_3D ( 'NONE', #3203, #35461, #50387 ) ;
#26704 = FACE_OUTER_BOUND ( 'NONE', #24542, .T. ) ;
#26705 = FACE_OUTER_BOUND ( 'NONE', #45314, .T. ) ;
#26706 = VERTEX_POINT ( 'NONE', #38353 ) ;
#26707 = AXIS2_PLACEMENT_3D ( 'NONE', #13573, #44787, #5307 ) ;
#26708 = DIRECTION ( 'NONE',  ( -0.4338837391175656699, 0.000000000000000000, 0.9009688679024154823 ) ) ;
#26709 = EDGE_CURVE ( 'NONE', #37439, #6627, #50411, .T. ) ;
#26710 = VECTOR ( 'NONE', #13780, 39.37007874015748143 ) ;
#26711 = LINE ( 'NONE', #42458, #32280 ) ;
#26712 = VECTOR ( 'NONE', #8376, 39.37007874015748143 ) ;
#26713 = VECTOR ( 'NONE', #18089, 39.37007874015748143 ) ;
#26714 = ORIENTED_EDGE ( 'NONE', *, *, #8366, .T. ) ;
#26715 = LINE ( 'NONE', #15099, #10033 ) ;
#26716 = FACE_OUTER_BOUND ( 'NONE', #38692, .T. ) ;
#26717 = DIRECTION ( 'NONE',  ( -0.01601477604151182663, 0.9998717552508123996, -0.000000000000000000 ) ) ;
#26718 = LINE ( 'NONE', #39104, #35739 ) ;
#26719 = DIRECTION ( 'NONE',  ( 0.8660254037844432595, 0.000000000000000000, 0.4999999999999920064 ) ) ;
#26720 = VECTOR ( 'NONE', #33849, 39.37007874015748143 ) ;
#26721 = EDGE_LOOP ( 'NONE', ( #48806, #22925, #36973, #20912 ) ) ;
#26722 = CARTESIAN_POINT ( 'NONE',  ( -0.3486774197067339376, 0.000000000000000000, 2.204724409448808764 ) ) ;
#26723 = ORIENTED_EDGE ( 'NONE', *, *, #47779, .T. ) ;
#26724 = FACE_BOUND ( 'NONE', #39569, .T. ) ;
#26725 = ADVANCED_FACE ( 'NONE', ( #23097 ), #18728, .F. ) ;
#26726 = LINE ( 'NONE', #42473, #25987 ) ;
#26727 = CARTESIAN_POINT ( 'NONE',  ( 0.8584932060599983483, 0.6447981115998610013, -1.427454079380622742 ) ) ;
#26728 = ADVANCED_FACE ( 'NONE', ( #39351 ), #3482, .F. ) ;
#26729 = ORIENTED_EDGE ( 'NONE', *, *, #7781, .F. ) ;
#26730 = ORIENTED_EDGE ( 'NONE', *, *, #6683, .T. ) ;
#26731 = CARTESIAN_POINT ( 'NONE',  ( 0.8329809839909849689, 1.496921813388997435, -2.833254665166554442 ) ) ;
#26732 = EDGE_CURVE ( 'NONE', #37481, #16476, #23342, .T. ) ;
#26733 = CARTESIAN_POINT ( 'NONE',  ( 0.5455278134075212115, 3.346456692913386100, -6.146657985744592735E-16 ) ) ;
#26734 = DIRECTION ( 'NONE',  ( 0.000000000000000000, 1.000000000000000000, 0.000000000000000000 ) ) ;
#26735 = CARTESIAN_POINT ( 'NONE',  ( -1.744243240276441398, 6.692913385826772199, 1.328042291889479642 ) ) ;
#26736 = LINE ( 'NONE', #50187, #45826 ) ;
#26737 = FACE_OUTER_BOUND ( 'NONE', #40147, .T. ) ;
#26738 = VERTEX_POINT ( 'NONE', #15100 ) ;
#26739 = CARTESIAN_POINT ( 'NONE',  ( -2.082617625631827174, 3.346456692913386100, -0.3149606299212589500 ) ) ;
#26740 = DIRECTION ( 'NONE',  ( -3.469446951953613696E-16, 0.000000000000000000, -1.000000000000000000 ) ) ;
#26741 = AXIS2_PLACEMENT_3D ( 'NONE', #20984, #20467, #36229 ) ;
#26742 = CARTESIAN_POINT ( 'NONE',  ( 3.927031490892378253E-16, 0.000000000000000000, 1.062992125984246083 ) ) ;
#26743 = VECTOR ( 'NONE', #34215, 39.37007874015748143 ) ;
#26744 = VERTEX_POINT ( 'NONE', #31105 ) ;
#26745 = DIRECTION ( 'NONE',  ( -1.000000000000000000, 0.000000000000000000, 0.000000000000000000 ) ) ;
#26746 = VECTOR ( 'NONE', #43790, 39.37007874015748854 ) ;
#26747 = VERTEX_POINT ( 'NONE', #19465 ) ;
#26748 = EDGE_LOOP ( 'NONE', ( #48099, #44631, #43149 ) ) ;
#26749 = VECTOR ( 'NONE', #41029, 39.37007874015748143 ) ;
#26750 = VECTOR ( 'NONE', #13140, 39.37007874015748143 ) ;
#26751 = VERTEX_POINT ( 'NONE', #26962 ) ;
#26752 = ORIENTED_EDGE ( 'NONE', *, *, #28395, .F. ) ;
#26753 = DIRECTION ( 'NONE',  ( -3.986037398843765983E-20, -1.000000000000000000, -1.160734090543304660E-16 ) ) ;
#26754 = VECTOR ( 'NONE', #44240, 39.37007874015748143 ) ;
#26755 = DIRECTION ( 'NONE',  ( -0.000000000000000000, 1.000000000000000000, -0.000000000000000000 ) ) ;
#26756 = CARTESIAN_POINT ( 'NONE',  ( 0.8182917201112819283, 0.000000000000000000, -1.299212598425193210 ) ) ;
#26757 = EDGE_CURVE ( 'NONE', #50819, #18885, #31445, .T. ) ;
#26758 = EDGE_CURVE ( 'NONE', #30631, #13474, #15605, .T. ) ;
#26759 = CARTESIAN_POINT ( 'NONE',  ( 2.318785432993162310, 1.755386055154334990, 1.828187805977548930 ) ) ;
#26760 = EDGE_CURVE ( 'NONE', #27229, #32984, #11725, .T. ) ;
#26761 = PLANE ( 'NONE',  #23678 ) ;
#26762 = CARTESIAN_POINT ( 'NONE',  ( -0.1692531782225912829, 0.000000000000000000, 0.3335283217915853138 ) ) ;
#26763 = ORIENTED_EDGE ( 'NONE', *, *, #6392, .T. ) ;
#26764 = CARTESIAN_POINT ( 'NONE',  ( 2.164658444855302122, 5.905511811023623991, -0.04795272066889885720 ) ) ;
#26765 = CARTESIAN_POINT ( 'NONE',  ( 0.7423782071083092626, 3.346456692913386100, 2.204724409448808764 ) ) ;
#26766 = DIRECTION ( 'NONE',  ( 1.734723475976806848E-16, -0.000000000000000000, 1.000000000000000000 ) ) ;
#26767 = PLANE ( 'NONE',  #12477 ) ;
#26768 = ORIENTED_EDGE ( 'NONE', *, *, #11352, .T. ) ;
#26769 = DIRECTION ( 'NONE',  ( -3.469446951953613696E-16, 0.000000000000000000, -1.000000000000000000 ) ) ;
#26770 = PLANE ( 'NONE',  #21999 ) ;
#26771 = ORIENTED_EDGE ( 'NONE', *, *, #9592, .T. ) ;
#26772 = DIRECTION ( 'NONE',  ( -1.000000000000000000, 0.000000000000000000, 1.734723475976806848E-16 ) ) ;
#26773 = DIRECTION ( 'NONE',  ( -0.000000000000000000, 0.000000000000000000, 1.000000000000000000 ) ) ;
#26774 = VECTOR ( 'NONE', #22516, 39.37007874015748143 ) ;
#26775 = AXIS2_PLACEMENT_3D ( 'NONE', #29958, #37971, #18337 ) ;
#26776 = DIRECTION ( 'NONE',  ( -0.000000000000000000, 0.000000000000000000, 1.000000000000000000 ) ) ;
#26777 = EDGE_CURVE ( 'NONE', #19545, #37274, #6849, .T. ) ;
#26778 = ORIENTED_EDGE ( 'NONE', *, *, #8111, .T. ) ;
#26779 = CARTESIAN_POINT ( 'NONE',  ( 0.7423782071083085965, 3.346456692913386100, 0.1181102362204701633 ) ) ;
#26780 = CONICAL_SURFACE ( 'NONE', #4537, 2.246510896728926010, 0.01601546068027819014 ) ;
#26781 = CARTESIAN_POINT ( 'NONE',  ( -1.546800823997126262, 1.683127104815683728, -1.546979550173933182 ) ) ;
#26782 = CARTESIAN_POINT ( 'NONE',  ( 1.363819533518803251, 0.000000000000000000, -0.9842519685039348154 ) ) ;
#26783 = ADVANCED_FACE ( 'NONE', ( #26716 ), #42462, .F. ) ;
#26784 = PLANE ( 'NONE',  #3677 ) ;
#26785 = LINE ( 'NONE', #42537, #8671 ) ;
#26786 = ORIENTED_EDGE ( 'NONE', *, *, #21441, .T. ) ;
#26787 = ADVANCED_FACE ( 'NONE', ( #24885 ), #22841, .T. ) ;
#26788 = CARTESIAN_POINT ( 'NONE',  ( -1.091055626815042645, 0.000000000000000000, -0.9448818897637760728 ) ) ;
#26789 = VECTOR ( 'NONE', #19879, 39.37007874015748143 ) ;
#26790 = EDGE_LOOP ( 'NONE', ( #39398, #46446, #9155, #40268 ) ) ;
#26791 = ORIENTED_EDGE ( 'NONE', *, *, #26364, .F. ) ;
#26792 = DIRECTION ( 'NONE',  ( 0.000000000000000000, 0.000000000000000000, 1.000000000000000000 ) ) ;
#26793 = ADVANCED_FACE ( 'NONE', ( #4496 ), #32384, .T. ) ;
#26794 = VERTEX_POINT ( 'NONE', #47820 ) ;
#26795 = FACE_OUTER_BOUND ( 'NONE', #25734, .T. ) ;
#26796 = CARTESIAN_POINT ( 'NONE',  ( -2.182111253630085290, 3.346456692913386100, -0.3149606299212589500 ) ) ;
#26797 = ORIENTED_EDGE ( 'NONE', *, *, #34288, .T. ) ;
#26798 = CARTESIAN_POINT ( 'NONE',  ( 1.271755610052043295, 3.267716535433071279, -2.086614173228339641 ) ) ;
#26799 = CARTESIAN_POINT ( 'NONE',  ( 0.000000000000000000, 3.346456692913386100, 0.000000000000000000 ) ) ;
#26800 = CARTESIAN_POINT ( 'NONE',  ( -0.1194579567165914291, 0.000000000000000000, 0.3504996250137321634 ) ) ;
#26801 = ORIENTED_EDGE ( 'NONE', *, *, #48239, .T. ) ;
#26802 = ORIENTED_EDGE ( 'NONE', *, *, #45928, .F. ) ;
#26803 = CARTESIAN_POINT ( 'NONE',  ( 0.1946711146504565004, 1.620088713232310518, -2.711980127628132120 ) ) ;
#26804 = FACE_BOUND ( 'NONE', #40467, .T. ) ;
#26805 = ORIENTED_EDGE ( 'NONE', *, *, #4647, .F. ) ;
#26806 = CARTESIAN_POINT ( 'NONE',  ( 2.164658444855302122, 5.905511811023623991, -0.04795272066889885720 ) ) ;
#26807 = VERTEX_POINT ( 'NONE', #35482 ) ;
#26808 = VERTEX_POINT ( 'NONE', #1123 ) ;
#26809 = DIRECTION ( 'NONE',  ( -1.000000000000000000, 0.000000000000000000, 1.734723475976806848E-16 ) ) ;
#26810 = VECTOR ( 'NONE', #25000, 39.37007874015748143 ) ;
#26811 = CARTESIAN_POINT ( 'NONE',  ( 0.000000000000000000, 0.000000000000000000, 0.000000000000000000 ) ) ;
#26812 = AXIS2_PLACEMENT_3D ( 'NONE', #37492, #1342, #17102 ) ;
#26813 = CONICAL_SURFACE ( 'NONE', #4567, 2.246510896728926010, 0.01601546068027819014 ) ;
#26814 = ORIENTED_EDGE ( 'NONE', *, *, #17152, .T. ) ;
#26815 = DIRECTION ( 'NONE',  ( -3.469446951953613696E-16, 0.000000000000000000, -1.000000000000000000 ) ) ;
#26816 = EDGE_LOOP ( 'NONE', ( #38210, #26053, #14173, #7059 ) ) ;
#26817 = DIRECTION ( 'NONE',  ( 0.000000000000000000, 0.000000000000000000, -1.000000000000000000 ) ) ;
#26818 = CARTESIAN_POINT ( 'NONE',  ( 1.909347346926324684, 0.000000000000000000, -0.4724409448818889246 ) ) ;
#26819 = DIRECTION ( 'NONE',  ( -3.469446951953613696E-16, 0.000000000000000000, -1.000000000000000000 ) ) ;
#26820 = VERTEX_POINT ( 'NONE', #102 ) ;
#26821 = ORIENTED_EDGE ( 'NONE', *, *, #40326, .T. ) ;
#26822 = EDGE_CURVE ( 'NONE', #7819, #25003, #19720, .T. ) ;
#26823 = VECTOR ( 'NONE', #30610, 39.37007874015748143 ) ;
#26824 = CARTESIAN_POINT ( 'NONE',  ( 0.1968503937007878568, 3.346456692913386100, 1.574803149606291974 ) ) ;
#26825 = CARTESIAN_POINT ( 'NONE',  ( -1.909347346926324906, 3.346456692913386100, -0.6692913385826758654 ) ) ;
#26826 = EDGE_CURVE ( 'NONE', #46112, #7183, #9132, .T. ) ;
#26827 = CARTESIAN_POINT ( 'NONE',  ( -1.166969139818015977, 3.346456692913386100, -1.732283464566922726 ) ) ;
#26828 = CARTESIAN_POINT ( 'NONE',  ( 0.8182917201112819283, 3.346456692913386100, -0.1574803149606301411 ) ) ;
#26829 = EDGE_CURVE ( 'NONE', #1980, #30932, #12333, .T. ) ;
#26830 = DIRECTION ( 'NONE',  ( -3.469446951953613696E-16, 0.000000000000000000, -1.000000000000000000 ) ) ;
#26831 = CARTESIAN_POINT ( 'NONE',  ( 2.042485253772177156, 1.205361022782829114E-17, 0.6118985000151695441 ) ) ;
#26832 = CARTESIAN_POINT ( 'NONE',  ( 0.002207914879453961969, 5.905511811023623991, 0.04916304461325442243 ) ) ;
#26833 = ORIENTED_EDGE ( 'NONE', *, *, #21998, .F. ) ;
#26834 = DIRECTION ( 'NONE',  ( -1.000000000000000000, -0.000000000000000000, -0.000000000000000000 ) ) ;
#26835 = CARTESIAN_POINT ( 'NONE',  ( -0.8182917201112814842, 3.346456692913386100, 1.102362204724404160 ) ) ;
#26836 = ORIENTED_EDGE ( 'NONE', *, *, #2056, .T. ) ;
#26837 = ORIENTED_EDGE ( 'NONE', *, *, #43048, .F. ) ;
#26838 = CARTESIAN_POINT ( 'NONE',  ( 0.2727639067037604392, 3.346456692913386100, -1.299212598425193210 ) ) ;
#26839 = DIRECTION ( 'NONE',  ( -0.000000000000000000, 1.000000000000000000, -0.000000000000000000 ) ) ;
#26840 = EDGE_CURVE ( 'NONE', #24696, #16316, #17093, .T. ) ;
#26841 = ORIENTED_EDGE ( 'NONE', *, *, #15085, .F. ) ;
#26842 = VECTOR ( 'NONE', #29592, 39.37007874015748143 ) ;
#26843 = ADVANCED_FACE ( 'NONE', ( #43462 ), #622, .F. ) ;
#26844 = ORIENTED_EDGE ( 'NONE', *, *, #19626, .F. ) ;
#26845 = CARTESIAN_POINT ( 'NONE',  ( 0.5455278134075208785, 3.267716535433071279, -2.034427629037600660 ) ) ;
#26846 = AXIS2_PLACEMENT_3D ( 'NONE', #9157, #44513, #19992 ) ;
#26847 = ORIENTED_EDGE ( 'NONE', *, *, #3477, .T. ) ;
#26848 = DIRECTION ( 'NONE',  ( 1.000000000000000000, 0.000000000000000000, 0.000000000000000000 ) ) ;
#26849 = DIRECTION ( 'NONE',  ( -0.9998717552508122886, -0.01601477604151180928, 0.000000000000000000 ) ) ;
#26850 = AXIS2_PLACEMENT_3D ( 'NONE', #9347, #40848, #5475 ) ;
#26851 = ORIENTED_EDGE ( 'NONE', *, *, #17947, .T. ) ;
#26852 = VECTOR ( 'NONE', #3936, 39.37007874015748143 ) ;
#26853 = LINE ( 'NONE', #39752, #20586 ) ;
#26854 = VERTEX_POINT ( 'NONE', #15847 ) ;
#26855 = ORIENTED_EDGE ( 'NONE', *, *, #39021, .T. ) ;
#26856 = CARTESIAN_POINT ( 'NONE',  ( -0.4350747367504789187, 5.905511811023623991, -2.121846421795420490 ) ) ;
#26857 = CARTESIAN_POINT ( 'NONE',  ( 0.002207914879453961535, -5.712274067634378313E-18, 0.04916304461325374242 ) ) ;
#26858 = CYLINDRICAL_SURFACE ( 'NONE', #23653, 2.165354330708661568 ) ;
#26859 = VERTEX_POINT ( 'NONE', #28229 ) ;
#26860 = CARTESIAN_POINT ( 'NONE',  ( -0.2727639067037607723, 3.267716535433071279, -0.7874015748031470974 ) ) ;
#26861 = CARTESIAN_POINT ( 'NONE',  ( 1.363819533518803251, 3.346456692913386100, -0.4724409448818889246 ) ) ;
#26862 = ORIENTED_EDGE ( 'NONE', *, *, #13225, .T. ) ;
#26863 = DIRECTION ( 'NONE',  ( -0.01601477604151182663, 0.9998717552508123996, -0.000000000000000000 ) ) ;
#26864 = ORIENTED_EDGE ( 'NONE', *, *, #37744, .T. ) ;
#26865 = VERTEX_POINT ( 'NONE', #20748 ) ;
#26866 = CARTESIAN_POINT ( 'NONE',  ( -2.482533714158320581, 30.85495225039662515, 71.79239159910525814 ) ) ;
#26867 = LINE ( 'NONE', #27630, #409 ) ;
#26868 = PLANE ( 'NONE',  #48054 ) ;
#26870 = LINE ( 'NONE', #37762, #9662 ) ;
#26869 = VECTOR ( 'NONE', #21506, 39.37007874015748143 ) ;
#26871 = CARTESIAN_POINT ( 'NONE',  ( -0.8182917201112814842, 3.346456692913386100, 1.732283464566921172 ) ) ;
#26872 = VERTEX_POINT ( 'NONE', #31606 ) ;
#26873 = ORIENTED_EDGE ( 'NONE', *, *, #12254, .F. ) ;
#26874 = EDGE_CURVE ( 'NONE', #1640, #25170, #7398, .T. ) ;
#26875 = VECTOR ( 'NONE', #31144, 39.37007874015748143 ) ;
#26876 = EDGE_CURVE ( 'NONE', #9734, #27371, #40686, .T. ) ;
#26877 = CIRCLE ( 'NONE', #49117, 2.164630168518208109 ) ;
#26878 = DIRECTION ( 'NONE',  ( -3.469446951953613696E-16, 0.000000000000000000, -1.000000000000000000 ) ) ;
#26879 = ORIENTED_EDGE ( 'NONE', *, *, #29921, .F. ) ;
#26880 = DIRECTION ( 'NONE',  ( 1.734723475976806848E-16, -0.000000000000000000, 1.000000000000000000 ) ) ;
#26881 = CARTESIAN_POINT ( 'NONE',  ( -0.5455278134075214336, 0.000000000000000000, -0.1968503937007883287 ) ) ;
#26882 = AXIS2_PLACEMENT_3D ( 'NONE', #30305, #11189, #39055 ) ;
#26883 = EDGE_CURVE ( 'NONE', #27703, #45433, #8024, .T. ) ;
#26884 = PRODUCT_RELATED_PRODUCT_CATEGORY ( 'part', '', ( #35980 ) ) ;
#26885 = VECTOR ( 'NONE', #21402, 39.37007874015748143 ) ;
#26886 = EDGE_CURVE ( 'NONE', #15755, #48506, #47566, .T. ) ;
#26887 = CARTESIAN_POINT ( 'NONE',  ( 2.136190583516914820, 1.205361022782829114E-17, -0.1451986319116555235 ) ) ;
#26888 = DIRECTION ( 'NONE',  ( -1.000000000000000000, 0.000000000000000000, 1.734723475976806848E-16 ) ) ;
#26889 = LINE ( 'NONE', #38030, #32001 ) ;
#26890 = AXIS2_PLACEMENT_3D ( 'NONE', #14874, #22368, #25729 ) ;
#26891 = ORIENTED_EDGE ( 'NONE', *, *, #4971, .T. ) ;
#26892 = CARTESIAN_POINT ( 'NONE',  ( 1.909347346926324684, 0.000000000000000000, -0.4724409448818889246 ) ) ;
#26893 = LINE ( 'NONE', #27147, #7076 ) ;
#26894 = CARTESIAN_POINT ( 'NONE',  ( -0.07591351300297340121, 3.267716535433071279, 0.2755905511810995412 ) ) ;
#26895 = EDGE_LOOP ( 'NONE', ( #28087, #43822, #37712, #2331 ) ) ;
#26896 = CARTESIAN_POINT ( 'NONE',  ( 0.5455278134075217666, 0.000000000000000000, 1.259842519685033357 ) ) ;
#26897 = DIRECTION ( 'NONE',  ( -0.9998717552508121775, -0.01601477604151182316, 0.000000000000000000 ) ) ;
#26898 = ADVANCED_FACE ( 'NONE', ( #16113 ), #28745, .F. ) ;
#26899 = CARTESIAN_POINT ( 'NONE',  ( 1.556712866041120247, 1.743522182421873401, 2.509548638715870084 ) ) ;
#26900 = VERTEX_POINT ( 'NONE', #40386 ) ;
#26901 = LINE ( 'NONE', #42652, #13533 ) ;
#26902 = EDGE_CURVE ( 'NONE', #37337, #23253, #31872, .T. ) ;
#26903 = ORIENTED_EDGE ( 'NONE', *, *, #37539, .F. ) ;
#26904 = LINE ( 'NONE', #34916, #20484 ) ;
#26905 = ORIENTED_EDGE ( 'NONE', *, *, #4226, .T. ) ;
#26906 = B_SPLINE_CURVE_WITH_KNOTS ( 'NONE', 3,
 ( #50628, #19432, #47537, #31579 ),
 .UNSPECIFIED., .F., .F.,
 ( 4, 4 ),
 ( 0.02719747141717294286, 0.02819803343359124012 ),
 .UNSPECIFIED. ) ;
#26907 = DIRECTION ( 'NONE',  ( -0.9998717552508122886, -0.01601477604151182316, 0.000000000000000000 ) ) ;
#26908 = VERTEX_POINT ( 'NONE', #8875 ) ;
#26909 = CARTESIAN_POINT ( 'NONE',  ( -1.636583440222564301, 3.267716535433071279, -0.3149606299212592275 ) ) ;
#26910 = FACE_OUTER_BOUND ( 'NONE', #46949, .T. ) ;
#26911 = DIRECTION ( 'NONE',  ( -1.000000000000000000, 0.000000000000000000, 1.734723475976806848E-16 ) ) ;
#26912 = EDGE_CURVE ( 'NONE', #47979, #24374, #40121, .T. ) ;
#26913 = AXIS2_PLACEMENT_3D ( 'NONE', #37084, #17962, #30093 ) ;
#26914 = VERTEX_POINT ( 'NONE', #24631 ) ;
#26915 = VERTEX_POINT ( 'NONE', #41395 ) ;
#26916 = VERTEX_POINT ( 'NONE', #17644 ) ;
#26917 = FACE_OUTER_BOUND ( 'NONE', #31855, .T. ) ;
#26918 = AXIS2_PLACEMENT_3D ( 'NONE', #3784, #3273, #3528 ) ;
#26919 = CARTESIAN_POINT ( 'NONE',  ( -0.5145850802035816240, 3.241398795825266355, -2.401574803149598036 ) ) ;
#26920 = VECTOR ( 'NONE', #41952, 39.37007874015748143 ) ;
#26921 = ORIENTED_EDGE ( 'NONE', *, *, #39480, .F. ) ;
#26922 = ORIENTED_EDGE ( 'NONE', *, *, #18510, .F. ) ;
#26923 = FACE_OUTER_BOUND ( 'NONE', #45845, .T. ) ;
#26924 = DIRECTION ( 'NONE',  ( 1.000000000000000000, 0.000000000000000000, 0.000000000000000000 ) ) ;
#26925 = FACE_OUTER_BOUND ( 'NONE', #12156, .T. ) ;
#26926 = EDGE_CURVE ( 'NONE', #30123, #34792, #6019, .T. ) ;
#26927 = VERTEX_POINT ( 'NONE', #33413 ) ;
#26928 = ORIENTED_EDGE ( 'NONE', *, *, #32925, .F. ) ;
#26929 = CARTESIAN_POINT ( 'NONE',  ( -1.909347346926324462, 3.346456692913386100, 0.9055118110236167750 ) ) ;
#26930 = CARTESIAN_POINT ( 'NONE',  ( -2.164823134740036181, 1.673236549936605977, -0.04796011690018290446 ) ) ;
#26931 = VECTOR ( 'NONE', #12538, 39.37007874015748143 ) ;
#26932 = FACE_OUTER_BOUND ( 'NONE', #40981, .T. ) ;
#26933 = VERTEX_POINT ( 'NONE', #30024 ) ;
#26934 = DIRECTION ( 'NONE',  ( -3.986037398843765983E-20, -1.000000000000000000, -1.160734090543304660E-16 ) ) ;
#26936 = VECTOR ( 'NONE', #16398, 39.37007874015748143 ) ;
#26935 = CARTESIAN_POINT ( 'NONE',  ( 1.091055626815042645, 0.000000000000000000, 0.3149606299212578953 ) ) ;
#26937 = EDGE_LOOP ( 'NONE', ( #50815, #31685, #18109, #35821 ) ) ;
#26938 = CARTESIAN_POINT ( 'NONE',  ( -0.8182917201112814842, 0.000000000000000000, 0.5905511811023582691 ) ) ;
#26939 = EDGE_LOOP ( 'NONE', ( #37004, #7496, #31343, #33747 ) ) ;
#26940 = ORIENTED_EDGE ( 'NONE', *, *, #25978, .F. ) ;
#26941 = DIRECTION ( 'NONE',  ( 1.000000000000000000, 0.000000000000000000, 0.000000000000000000 ) ) ;
#26942 = DIRECTION ( 'NONE',  ( -3.469446951953613696E-16, 0.000000000000000000, -1.000000000000000000 ) ) ;
#26943 = DIRECTION ( 'NONE',  ( 0.01601477604151182663, -0.9998717552508123996, 0.000000000000000000 ) ) ;
#26944 = FACE_OUTER_BOUND ( 'NONE', #42675, .T. ) ;
#26945 = CARTESIAN_POINT ( 'NONE',  ( -1.530693736245497316, 5.905511811023623991, -1.531579597454066688 ) ) ;
#26946 = ORIENTED_EDGE ( 'NONE', *, *, #8137, .F. ) ;
#26947 = ORIENTED_EDGE ( 'NONE', *, *, #27520, .T. ) ;
#26948 = CARTESIAN_POINT ( 'NONE',  ( -1.363819533518803473, 0.000000000000000000, -0.3543307086614174151 ) ) ;
#26949 = LINE ( 'NONE', #26450, #27581 ) ;
#26950 = EDGE_CURVE ( 'NONE', #7408, #2174, #10408, .T. ) ;
#26951 = EDGE_CURVE ( 'NONE', #814, #45623, #5254, .T. ) ;
#26952 = VECTOR ( 'NONE', #42207, 39.37007874015748143 ) ;
#26953 = ADVANCED_FACE ( 'NONE', ( #1637 ), #46710, .T. ) ;
#26954 = FACE_OUTER_BOUND ( 'NONE', #36846, .T. ) ;
#26955 = LINE ( 'NONE', #7352, #41877 ) ;
#26956 = VECTOR ( 'NONE', #11776, 39.37007874015748143 ) ;
#26957 = ORIENTED_EDGE ( 'NONE', *, *, #21064, .F. ) ;
#26958 = PLANE ( 'NONE',  #31628 ) ;
#26959 = DIRECTION ( 'NONE',  ( 1.000000000000000000, -0.000000000000000000, 0.000000000000000000 ) ) ;
#26960 = ORIENTED_EDGE ( 'NONE', *, *, #30405, .F. ) ;
#26961 = DIRECTION ( 'NONE',  ( -3.469446951953613696E-16, 0.000000000000000000, -1.000000000000000000 ) ) ;
#26962 = CARTESIAN_POINT ( 'NONE',  ( -0.8942052331142552601, 3.267716535433071279, -1.889763779527552146 ) ) ;
#26963 = CARTESIAN_POINT ( 'NONE',  ( -1.909347346926324462, 3.346456692913386100, 0.2755905511810996522 ) ) ;
#26964 = LINE ( 'NONE', #19219, #23430 ) ;
#26965 = DIRECTION ( 'NONE',  ( -3.469446951953613696E-16, 0.000000000000000000, -1.000000000000000000 ) ) ;
#26966 = DIRECTION ( 'NONE',  ( -0.9998717552508121775, -0.01601477604151182316, 0.000000000000000000 ) ) ;
#26967 = EDGE_LOOP ( 'NONE', ( #39071, #50239, #1335, #446 ) ) ;
#26968 = CARTESIAN_POINT ( 'NONE',  ( 0.7423782071083087075, 3.346456692913386100, -0.6299212598425181220 ) ) ;
#26969 = ORIENTED_EDGE ( 'NONE', *, *, #14702, .T. ) ;
#26970 = VECTOR ( 'NONE', #10262, 39.37007874015748143 ) ;
#26971 = DIRECTION ( 'NONE',  ( 1.000000000000000000, -0.000000000000000000, 0.000000000000000000 ) ) ;
#26972 = DIRECTION ( 'NONE',  ( -0.000000000000000000, 1.000000000000000000, -0.000000000000000000 ) ) ;
#26973 = CARTESIAN_POINT ( 'NONE',  ( -1.091055626815042645, 3.346456692913386100, -0.6299212598425177889 ) ) ;
#26974 = EDGE_CURVE ( 'NONE', #39762, #20325, #42505, .T. ) ;
#26975 = ORIENTED_EDGE ( 'NONE', *, *, #50962, .F. ) ;
#26976 = VERTEX_POINT ( 'NONE', #37022 ) ;
#26977 = FACE_OUTER_BOUND ( 'NONE', #8259, .T. ) ;
#26978 = CARTESIAN_POINT ( 'NONE',  ( 0.000000000000000000, 2.755905511811024056, 0.000000000000000000 ) ) ;
#26979 = CARTESIAN_POINT ( 'NONE',  ( -0.2727639067037610499, 3.346456692913386100, -2.047244094488181343 ) ) ;
#26980 = CARTESIAN_POINT ( 'NONE',  ( 0.6157060065419059924, 0.5249316497054298258, 1.780600057069692710 ) ) ;
#26981 = CARTESIAN_POINT ( 'NONE',  ( 0.000000000000000000, 3.267716535433071279, 1.220472440944875059 ) ) ;
#26982 = ADVANCED_FACE ( 'NONE', ( #32905 ), #41149, .F. ) ;
#26983 = CARTESIAN_POINT ( 'NONE',  ( 1.617022397669051870, 1.737311993599926607, 1.925629205347350492 ) ) ;
#26984 = ORIENTED_EDGE ( 'NONE', *, *, #4351, .T. ) ;
#26985 = ORIENTED_EDGE ( 'NONE', *, *, #30774, .T. ) ;
#26986 = DIRECTION ( 'NONE',  ( 0.000000000000000000, 0.000000000000000000, 1.000000000000000000 ) ) ;
#26987 = VECTOR ( 'NONE', #4204, 39.37007874015748143 ) ;
#26988 = ADVANCED_FACE ( 'NONE', ( #21011 ), #12143, .T. ) ;
#26989 = CIRCLE ( 'NONE', #18753, 2.165354330708661568 ) ;
#26990 = DIRECTION ( 'NONE',  ( -0.2660368455666826670, 0.000000000000000000, 0.9639628606958512425 ) ) ;
#26991 = ORIENTED_EDGE ( 'NONE', *, *, #38939, .F. ) ;
#26992 = ADVANCED_FACE ( 'NONE', ( #17899 ), #1896, .F. ) ;
#26993 = DIRECTION ( 'NONE',  ( -0.04486483035051863633, 1.288287287306305283E-16, 0.9989930665413144784 ) ) ;
#26994 = ORIENTED_EDGE ( 'NONE', *, *, #10772, .T. ) ;
#26995 = ORIENTED_EDGE ( 'NONE', *, *, #47070, .F. ) ;
#26996 = EDGE_CURVE ( 'NONE', #16457, #14773, #49598, .T. ) ;
#26997 = EDGE_LOOP ( 'NONE', ( #30574, #30483, #36118, #11262, #20317, #16928, #33226, #28239 ) ) ;
#26998 = EDGE_LOOP ( 'NONE', ( #37978, #34189, #38948, #38354 ) ) ;
#26999 = CARTESIAN_POINT ( 'NONE',  ( 0.5548376931676505253, 1.651171896322103150, -2.195393375338218878 ) ) ;
#27001 = PLANE ( 'NONE',  #1515 ) ;
#27000 = VECTOR ( 'NONE', #10208, 39.37007874015748143 ) ;
#27002 = LINE ( 'NONE', #46355, #41750 ) ;
#27003 = CARTESIAN_POINT ( 'NONE',  ( 2.112319093887386146, 0.000000000000000000, 0.3357951146312926904 ) ) ;
#27004 = EDGE_CURVE ( 'NONE', #27036, #4710, #45491, .T. ) ;
#27005 = FACE_OUTER_BOUND ( 'NONE', #43998, .T. ) ;
#27006 = ADVANCED_FACE ( 'NONE', ( #25642 ), #10150, .T. ) ;
#27007 = EDGE_CURVE ( 'NONE', #39256, #43417, #48836, .T. ) ;
#27008 = PLANE ( 'NONE',  #25343 ) ;
#27009 = CARTESIAN_POINT ( 'NONE',  ( -2.695799277629577162, 0.000000000000000000, -1.205759334241492509 ) ) ;
#27010 = ORIENTED_EDGE ( 'NONE', *, *, #49492, .T. ) ;
#27011 = DIRECTION ( 'NONE',  ( 1.606762707810401785E-15, -0.7071067811865483499, 0.7071067811865466846 ) ) ;
#27012 = CARTESIAN_POINT ( 'NONE',  ( -0.2727639067037602727, 3.346456692913386100, 0.5905511811023582691 ) ) ;
#27013 = CARTESIAN_POINT ( 'NONE',  ( 0.000000000000000000, 3.267716535433071279, -0.3149606299212593941 ) ) ;
#27014 = LINE ( 'NONE', #49970, #950 ) ;
#27015 = ORIENTED_EDGE ( 'NONE', *, *, #23277, .F. ) ;
#27016 = DIRECTION ( 'NONE',  ( -0.000000000000000000, 0.000000000000000000, 1.000000000000000000 ) ) ;
#27017 = LINE ( 'NONE', #42771, #18676 ) ;
#27018 = ORIENTED_EDGE ( 'NONE', *, *, #6503, .T. ) ;
#27019 = CARTESIAN_POINT ( 'NONE',  ( 1.971834065208952769, 1.205361022782829114E-17, 0.8963217522330182430 ) ) ;
#27020 = AXIS2_PLACEMENT_3D ( 'NONE', #22294, #6794, #14284 ) ;
#27021 = AXIS2_PLACEMENT_3D ( 'NONE', #26782, #22419, #18034 ) ;
#27022 = LINE ( 'NONE', #165, #10284 ) ;
#27023 = AXIS2_PLACEMENT_3D ( 'NONE', #42858, #31260, #46954 ) ;
#27024 = DIRECTION ( 'NONE',  ( -1.000000000000000000, 0.000000000000000000, 0.000000000000000000 ) ) ;
#27025 = ORIENTED_EDGE ( 'NONE', *, *, #43702, .F. ) ;
#27026 = CARTESIAN_POINT ( 'NONE',  ( 0.04921259842519613847, 5.905511811023623991, -2.165433070866141119 ) ) ;
#27027 = CARTESIAN_POINT ( 'NONE',  ( 0.1067246931122726866, 0.02962905676920215767, 0.000000000000000000 ) ) ;
#27029 = DIRECTION ( 'NONE',  ( 0.000000000000000000, 0.000000000000000000, 1.000000000000000000 ) ) ;
#27028 = VECTOR ( 'NONE', #36005, 39.37007874015748143 ) ;
#27030 = CARTESIAN_POINT ( 'NONE',  ( -2.878724150143177507, 0.000000000000000000, -0.6570500018395228903 ) ) ;
#27031 = DIRECTION ( 'NONE',  ( 0.000000000000000000, 0.000000000000000000, 1.000000000000000000 ) ) ;
#27032 = ORIENTED_EDGE ( 'NONE', *, *, #32761, .T. ) ;
#27033 = ADVANCED_FACE ( 'NONE', ( #17140 ), #25895, .F. ) ;
#27034 = AXIS2_PLACEMENT_3D ( 'NONE', #29938, #45653, #36670 ) ;
#27035 = B_SPLINE_CURVE_WITH_KNOTS ( 'NONE', 3,
 ( #3354, #30222, #42338, #7483 ),
 .UNSPECIFIED., .F., .F.,
 ( 4, 4 ),
 ( 2.136715943794443357E-07, 0.01735814470125059822 ),
 .UNSPECIFIED. ) ;
#27036 = VERTEX_POINT ( 'NONE', #40887 ) ;
#27037 = ORIENTED_EDGE ( 'NONE', *, *, #9130, .F. ) ;
#27038 = DIRECTION ( 'NONE',  ( -0.000000000000000000, 1.000000000000000000, -0.000000000000000000 ) ) ;
#27039 = ORIENTED_EDGE ( 'NONE', *, *, #5558, .T. ) ;
#27040 = CARTESIAN_POINT ( 'NONE',  ( 0.04921259842519675604, 1.019021312707606430, 2.584985224492306610 ) ) ;
#27041 = AXIS2_PLACEMENT_3D ( 'NONE', #5507, #14267, #21257 ) ;
#27042 = CARTESIAN_POINT ( 'NONE',  ( 0.1067246931122726866, 0.02962905676920215767, 0.000000000000000000 ) ) ;
#27043 = EDGE_LOOP ( 'NONE', ( #6513, #10045, #23618, #5032 ) ) ;
#27044 = EDGE_CURVE ( 'NONE', #19370, #25998, #2412, .T. ) ;
#27045 = CARTESIAN_POINT ( 'NONE',  ( 4.268512490100411402E-16, 0.000000000000000000, 0.9448818897637749625 ) ) ;
#27046 = EDGE_CURVE ( 'NONE', #47061, #22090, #15431, .T. ) ;
#27047 = ORIENTED_EDGE ( 'NONE', *, *, #8592, .F. ) ;
#27048 = DIRECTION ( 'NONE',  ( -0.000000000000000000, 1.000000000000000000, -0.000000000000000000 ) ) ;
#27049 = ADVANCED_FACE ( 'NONE', ( #29521 ), #42614, .T. ) ;
#27050 = ORIENTED_EDGE ( 'NONE', *, *, #24103, .F. ) ;
#27051 = ORIENTED_EDGE ( 'NONE', *, *, #49234, .F. ) ;
#27052 = DIRECTION ( 'NONE',  ( 0.6579387259397138088, 8.738534663690390683E-17, -0.7530714660036099684 ) ) ;
#27053 = ORIENTED_EDGE ( 'NONE', *, *, #12467, .F. ) ;
#27054 = LINE ( 'NONE', #18570, #44320 ) ;
#27055 = CIRCLE ( 'NONE', #4821, 2.106299212598425008 ) ;
#27056 = ORIENTED_EDGE ( 'NONE', *, *, #9263, .F. ) ;
#27057 = ORIENTED_EDGE ( 'NONE', *, *, #37328, .F. ) ;
#27058 = EDGE_CURVE ( 'NONE', #6407, #33053, #16639, .T. ) ;
#27059 = DIRECTION ( 'NONE',  ( 1.000000000000000000, -0.000000000000000000, 0.000000000000000000 ) ) ;
#27060 = CARTESIAN_POINT ( 'NONE',  ( -1.739002864725096353, 1.589738220721540696, 2.065247083924816263 ) ) ;
#27061 = VERTEX_POINT ( 'NONE', #42393 ) ;
#27062 = AXIS2_PLACEMENT_3D ( 'NONE', #3708, #19941, #39584 ) ;
#27063 = EDGE_CURVE ( 'NONE', #50666, #25092, #9224, .T. ) ;
#27064 = DIRECTION ( 'NONE',  ( 1.000000000000000000, 0.000000000000000000, 0.000000000000000000 ) ) ;
#27065 = ORIENTED_EDGE ( 'NONE', *, *, #40436, .T. ) ;
#27066 = LINE ( 'NONE', #31461, #3789 ) ;
#27067 = CARTESIAN_POINT ( 'NONE',  ( -1.909347346926324906, 3.267716535433071279, 1.220472440944875059 ) ) ;
#27068 = AXIS2_PLACEMENT_3D ( 'NONE', #49036, #21211, #40831 ) ;
#27069 = CARTESIAN_POINT ( 'NONE',  ( 0.1968503937007878568, 3.346456692913386100, 1.574803149606291974 ) ) ;
#27070 = EDGE_CURVE ( 'NONE', #1339, #36309, #39998, .T. ) ;
#27071 = VECTOR ( 'NONE', #48687, 39.37007874015748143 ) ;
#27072 = ORIENTED_EDGE ( 'NONE', *, *, #16505, .T. ) ;
#27073 = EDGE_LOOP ( 'NONE', ( #7559, #8903, #45650, #48986 ) ) ;
#27074 = CARTESIAN_POINT ( 'NONE',  ( -0.4788131938641533303, 1.613355999311305133, 2.914091152102185944 ) ) ;
#27075 = CARTESIAN_POINT ( 'NONE',  ( -2.950518648203841021, 1.673261099661152773, -0.1160872160806489667 ) ) ;
#27076 = EDGE_CURVE ( 'NONE', #5201, #41095, #40987, .T. ) ;
#27077 = CARTESIAN_POINT ( 'NONE',  ( -1.091055626815042645, 3.267716535433071279, -1.574803149606293529 ) ) ;
#27078 = VECTOR ( 'NONE', #39415, 39.37007874015748143 ) ;
#27079 = LINE ( 'NONE', #46923, #17757 ) ;
#27080 = DIRECTION ( 'NONE',  ( -0.9839295885986321100, -1.160734090543304660E-16, 0.1785568947986229116 ) ) ;
#27081 = B_SPLINE_CURVE_WITH_KNOTS ( 'NONE', 3,
 ( #3172, #33423, #13788, #45248 ),
 .UNSPECIFIED., .F., .F.,
 ( 4, 4 ),
 ( 3.689117391458506506E-07, 0.04851997785222408183 ),
 .UNSPECIFIED. ) ;
#27082 = VECTOR ( 'NONE', #28606, 39.37007874015748143 ) ;
#27083 = CARTESIAN_POINT ( 'NONE',  ( -2.430161915918442439, 3.241492618072995047, -0.3543307086614173040 ) ) ;
#27084 = DIRECTION ( 'NONE',  ( 1.000000000000000000, 0.000000000000000000, 0.000000000000000000 ) ) ;
#27085 = EDGE_LOOP ( 'NONE', ( #29426, #6979, #16151, #25958 ) ) ;
#27086 = CARTESIAN_POINT ( 'NONE',  ( 0.000000000000000000, 3.267716535433071279, -1.141732283464563791 ) ) ;
#27087 = B_SPLINE_CURVE_WITH_KNOTS ( 'NONE', 3,
 ( #35537, #38397, #15657, #15151 ),
 .UNSPECIFIED., .F., .F.,
 ( 4, 4 ),
 ( 2.895194837543627171E-07, 0.01651717637142990913 ),
 .UNSPECIFIED. ) ;
#27088 = EDGE_LOOP ( 'NONE', ( #267, #24609, #17719, #22161 ) ) ;
#27089 = ORIENTED_EDGE ( 'NONE', *, *, #22295, .F. ) ;
#27090 = LINE ( 'NONE', #39483, #21748 ) ;
#27091 = CARTESIAN_POINT ( 'NONE',  ( 2.378961647330872786, 3.346456692913386100, -0.5118110236220471121 ) ) ;
#27092 = VECTOR ( 'NONE', #121, 39.37007874015748143 ) ;
#27093 = VERTEX_POINT ( 'NONE', #42146 ) ;
#27094 = LINE ( 'NONE', #7736, #46038 ) ;
#27095 = ORIENTED_EDGE ( 'NONE', *, *, #35407, .T. ) ;
#27096 = DIRECTION ( 'NONE',  ( 1.000000000000000000, 0.000000000000000000, 0.000000000000000000 ) ) ;
#27097 = VERTEX_POINT ( 'NONE', #15038 ) ;
#27098 = AXIS2_PLACEMENT_3D ( 'NONE', #20973, #32607, #48292 ) ;
#27099 = AXIS2_PLACEMENT_3D ( 'NONE', #9023, #24771, #1273 ) ;
#27100 = CARTESIAN_POINT ( 'NONE',  ( -0.3742159057234073494, 0.02192591290182492950, 1.786486621533327712 ) ) ;
#27101 = CARTESIAN_POINT ( 'NONE',  ( -1.387241876633673598, 1.574803149606302854, 1.662624236931676824 ) ) ;
#27102 = EDGE_CURVE ( 'NONE', #9419, #8409, #46988, .T. ) ;
#27103 = B_SPLINE_CURVE_WITH_KNOTS ( 'NONE', 3,
 ( #18668, #26404, #22289, #22036 ),
 .UNSPECIFIED., .F., .F.,
 ( 4, 4 ),
 ( 2.396011864035455169E-07, 0.002500390292889080948 ),
 .UNSPECIFIED. ) ;
#27104 = VECTOR ( 'NONE', #28923, 39.37007874015748143 ) ;
#27105 = ORIENTED_EDGE ( 'NONE', *, *, #6758, .F. ) ;
#27106 = EDGE_CURVE ( 'NONE', #25849, #42, #22754, .T. ) ;
#27107 = CARTESIAN_POINT ( 'NONE',  ( 0.2727639067037604392, 3.267716535433071279, -0.6692913385826760875 ) ) ;
#27108 = EDGE_CURVE ( 'NONE', #9748, #2103, #7294, .T. ) ;
#27109 = ORIENTED_EDGE ( 'NONE', *, *, #33293, .T. ) ;
#27110 = ORIENTED_EDGE ( 'NONE', *, *, #27754, .F. ) ;
#27111 = DIRECTION ( 'NONE',  ( -1.045785279492548401E-16, -1.000000000000000000, 5.036236473261409814E-17 ) ) ;
#27112 = LINE ( 'NONE', #37046, #3424 ) ;
#27113 = FACE_OUTER_BOUND ( 'NONE', #5470, .T. ) ;
#27114 = VECTOR ( 'NONE', #11663, 39.37007874015748143 ) ;
#27115 = ORIENTED_EDGE ( 'NONE', *, *, #22322, .T. ) ;
#27116 = CARTESIAN_POINT ( 'NONE',  ( -0.2727639067037607168, 3.267716535433071279, 4.731699523581612206E-17 ) ) ;
#27117 = CARTESIAN_POINT ( 'NONE',  ( -1.091055626815042645, 3.267716535433071279, 1.892679809432644882E-16 ) ) ;
#27118 = ORIENTED_EDGE ( 'NONE', *, *, #7210, .T. ) ;
#27119 = CARTESIAN_POINT ( 'NONE',  ( 0.000000000000000000, 3.267716535433071279, 0.7480314960629872445 ) ) ;
#27120 = B_SPLINE_CURVE_WITH_KNOTS ( 'NONE', 3,
 ( #15381, #15629, #27745, #386 ),
 .UNSPECIFIED., .F., .F.,
 ( 4, 4 ),
 ( 2.008389810339514362E-07, 0.01780505990002694341 ),
 .UNSPECIFIED. ) ;
#27121 = ORIENTED_EDGE ( 'NONE', *, *, #41175, .T. ) ;
#27122 = ORIENTED_EDGE ( 'NONE', *, *, #44697, .T. ) ;
#27123 = EDGE_CURVE ( 'NONE', #43045, #21585, #35165, .T. ) ;
#27124 = VERTEX_POINT ( 'NONE', #19152 ) ;
#27125 = PLANE ( 'NONE',  #44913 ) ;
#27126 = CARTESIAN_POINT ( 'NONE',  ( -2.152441353505195387, 0.000000000000000000, -0.2419059403265113872 ) ) ;
#27127 = ADVANCED_FACE ( 'NONE', ( #15289 ), #15544, .F. ) ;
#27128 = VECTOR ( 'NONE', #2172, 39.37007874015748143 ) ;
#27129 = CARTESIAN_POINT ( 'NONE',  ( -1.091055626815042645, 0.000000000000000000, -2.086614173228339641 ) ) ;
#27130 = CARTESIAN_POINT ( 'NONE',  ( 0.7423782071083087075, 3.267716535433071279, 0.6299212598425161236 ) ) ;
#27131 = B_SPLINE_CURVE_WITH_KNOTS ( 'NONE', 3,
 ( #46344, #2249, #29619, #29870 ),
 .UNSPECIFIED., .F., .F.,
 ( 4, 4 ),
 ( 0.01379717137572002324, 0.03074487227025578251 ),
 .UNSPECIFIED. ) ;
#27132 = ORIENTED_EDGE ( 'NONE', *, *, #32751, .F. ) ;
#27133 = ORIENTED_EDGE ( 'NONE', *, *, #16465, .F. ) ;
#27134 = EDGE_CURVE ( 'NONE', #27935, #25931, #34412, .T. ) ;
#27135 = DIRECTION ( 'NONE',  ( 0.01601477604151182663, -0.9998717552508123996, 0.000000000000000000 ) ) ;
#27136 = EDGE_LOOP ( 'NONE', ( #30622, #46171, #20520, #34022 ) ) ;
#27137 = EDGE_CURVE ( 'NONE', #12624, #8046, #1174, .T. ) ;
#27138 = CARTESIAN_POINT ( 'NONE',  ( 2.592410251782301778, 1.759648616974466950, 1.413663899099648180 ) ) ;
#27139 = LINE ( 'NONE', #30771, #16922 ) ;
#27140 = AXIS2_PLACEMENT_3D ( 'NONE', #602, #32362, #20210 ) ;
#27141 = VECTOR ( 'NONE', #33918, 39.37007874015748143 ) ;
#27142 = CARTESIAN_POINT ( 'NONE',  ( 0.4696143004045484903, 3.346456692913386100, 2.047244094488179567 ) ) ;
#27143 = CARTESIAN_POINT ( 'NONE',  ( -0.8182917201112819283, 3.346456692913386100, -0.1574803149606301411 ) ) ;
#27144 = DIRECTION ( 'NONE',  ( 0.000000000000000000, 1.000000000000000000, 0.000000000000000000 ) ) ;
#27145 = ORIENTED_EDGE ( 'NONE', *, *, #38439, .F. ) ;
#27146 = LINE ( 'NONE', #26146, #48905 ) ;
#27147 = CARTESIAN_POINT ( 'NONE',  ( 0.000000000000000000, 3.267716535433071279, -1.929133858267710000 ) ) ;
#27148 = AXIS2_PLACEMENT_3D ( 'NONE', #28166, #40055, #20427 ) ;
#27149 = ORIENTED_EDGE ( 'NONE', *, *, #50803, .F. ) ;
#27150 = DIRECTION ( 'NONE',  ( -1.000000000000000000, -0.000000000000000000, -0.000000000000000000 ) ) ;
#27151 = CARTESIAN_POINT ( 'NONE',  ( -0.6089661318347402430, 1.603610328167266230, -2.391523368051897247 ) ) ;
#27152 = CARTESIAN_POINT ( 'NONE',  ( 1.472219874544873131, 1.742205712729733014, 2.560030851058970214 ) ) ;
#27153 = ORIENTED_EDGE ( 'NONE', *, *, #36299, .T. ) ;
#27154 = ORIENTED_EDGE ( 'NONE', *, *, #45460, .F. ) ;
#27155 = DIRECTION ( 'NONE',  ( -3.986037398843765983E-20, -1.000000000000000000, -1.160734090543304660E-16 ) ) ;
#27156 = ORIENTED_EDGE ( 'NONE', *, *, #42428, .F. ) ;
#27157 = B_SPLINE_CURVE_WITH_KNOTS ( 'NONE', 3,
 ( #11302, #20044, #31949, #47644 ),
 .UNSPECIFIED., .F., .F.,
 ( 4, 4 ),
 ( 0.1211775127643062860, 0.1625894504277921315 ),
 .UNSPECIFIED. ) ;
#27158 = DIRECTION ( 'NONE',  ( -3.469446951953613696E-16, 0.000000000000000000, -1.000000000000000000 ) ) ;
#27159 = ORIENTED_EDGE ( 'NONE', *, *, #15184, .T. ) ;
#27160 = DIRECTION ( 'NONE',  ( -0.000000000000000000, 0.000000000000000000, 1.000000000000000000 ) ) ;
#27161 = CARTESIAN_POINT ( 'NONE',  ( -0.2727639067037602172, 3.346456692913386100, 0.7874015748031456541 ) ) ;
#27162 = FACE_OUTER_BOUND ( 'NONE', #39843, .T. ) ;
#27163 = VECTOR ( 'NONE', #5148, 39.37007874015748143 ) ;
#27164 = EDGE_LOOP ( 'NONE', ( #50943, #32899, #21099, #19413 ) ) ;
#27165 = ADVANCED_FACE ( 'NONE', ( #50103 ), #46743, .F. ) ;
#27166 = ORIENTED_EDGE ( 'NONE', *, *, #14264, .T. ) ;
#27167 = EDGE_LOOP ( 'NONE', ( #26038, #12630, #30869, #18612 ) ) ;
#27168 = PLANE ( 'NONE',  #5931 ) ;
#27169 = DIRECTION ( 'NONE',  ( -0.01601477604151182663, 0.9998717552508123996, -0.000000000000000000 ) ) ;
#27170 = EDGE_CURVE ( 'NONE', #4133, #46268, #3665, .T. ) ;
#27171 = ORIENTED_EDGE ( 'NONE', *, *, #3770, .F. ) ;
#27172 = ORIENTED_EDGE ( 'NONE', *, *, #367, .F. ) ;
#27173 = CARTESIAN_POINT ( 'NONE',  ( 0.000000000000000000, 3.267716535433071279, -0.4724409448818889246 ) ) ;
#27174 = LINE ( 'NONE', #42168, #42558 ) ;
#27175 = CARTESIAN_POINT ( 'NONE',  ( 0.7308738700548027545, 6.692913385826772199, 2.087463732006447970 ) ) ;
#27176 = EDGE_CURVE ( 'NONE', #48689, #46386, #38539, .T. ) ;
#27177 = EDGE_CURVE ( 'NONE', #34110, #47282, #14790, .T. ) ;
#27178 = VECTOR ( 'NONE', #38019, 39.37007874015748143 ) ;
#27179 = ORIENTED_EDGE ( 'NONE', *, *, #22601, .T. ) ;
#27180 = ORIENTED_EDGE ( 'NONE', *, *, #10625, .F. ) ;
#27181 = PLANE ( 'NONE',  #20525 ) ;
#27182 = LINE ( 'NONE', #38569, #43941 ) ;
#27183 = CARTESIAN_POINT ( 'NONE',  ( 1.363819533518803251, 3.346456692913386100, -0.7874015748031473194 ) ) ;
#27184 = EDGE_CURVE ( 'NONE', #39372, #44367, #23282, .T. ) ;
#27185 = ORIENTED_EDGE ( 'NONE', *, *, #37063, .F. ) ;
#27186 = LINE ( 'NONE', #47022, #12520 ) ;
#27187 = CARTESIAN_POINT ( 'NONE',  ( 0.5455278134075216556, 0.000000000000000000, 1.377952755905504256 ) ) ;
#27188 = ORIENTED_EDGE ( 'NONE', *, *, #39204, .F. ) ;
#27189 = DIRECTION ( 'NONE',  ( -0.000000000000000000, 1.000000000000000000, -0.000000000000000000 ) ) ;
#27190 = ORIENTED_EDGE ( 'NONE', *, *, #44999, .T. ) ;
#27191 = VERTEX_POINT ( 'NONE', #32064 ) ;
#27192 = VECTOR ( 'NONE', #50116, 39.37007874015748143 ) ;
#27193 = DIRECTION ( 'NONE',  ( 0.000000000000000000, 1.000000000000000000, 0.000000000000000000 ) ) ;
#27194 = CARTESIAN_POINT ( 'NONE',  ( 2.013783482383322720, 1.740156378764222245, 1.139548688847630942 ) ) ;
#27195 = CARTESIAN_POINT ( 'NONE',  ( 2.052631463899902364, 3.267716535433071279, 0.4724409448818868706 ) ) ;
#27196 = EDGE_CURVE ( 'NONE', #8227, #16479, #7792, .T. ) ;
#27197 = CARTESIAN_POINT ( 'NONE',  ( -1.097585813245683273, 0.4349011127721510994, -0.9794755770252108196 ) ) ;
#27198 = DIRECTION ( 'NONE',  ( 1.734723475976806848E-16, -0.000000000000000000, 1.000000000000000000 ) ) ;
#27199 = VERTEX_POINT ( 'NONE', #47756 ) ;
#27200 = ORIENTED_EDGE ( 'NONE', *, *, #2010, .T. ) ;
#27201 = EDGE_CURVE ( 'NONE', #40666, #12335, #23530, .T. ) ;
#27202 = EDGE_LOOP ( 'NONE', ( #1465, #16064, #44820, #14586 ) ) ;
#27203 = CARTESIAN_POINT ( 'NONE',  ( -1.909347346926324462, 0.000000000000000000, 0.5905511811023582691 ) ) ;
#27204 = DIRECTION ( 'NONE',  ( -0.000000000000000000, 1.000000000000000000, -0.000000000000000000 ) ) ;
#27205 = B_SPLINE_CURVE_WITH_KNOTS ( 'NONE', 3,
 ( #25159, #5538, #35755, #384 ),
 .UNSPECIFIED., .F., .F.,
 ( 4, 4 ),
 ( 2.175031256469753215E-07, 0.01988369477650668918 ),
 .UNSPECIFIED. ) ;
#27206 = CARTESIAN_POINT ( 'NONE',  ( -1.723687301221637824, 6.692913385826772199, -1.311649477509824857 ) ) ;
#27207 = DIRECTION ( 'NONE',  ( 1.734723475976806848E-16, -0.000000000000000000, 1.000000000000000000 ) ) ;
#27208 = ORIENTED_EDGE ( 'NONE', *, *, #49799, .F. ) ;
#27209 = CARTESIAN_POINT ( 'NONE',  ( -1.721689136163420786, 1.040663155869206546, 1.895833630352641297 ) ) ;
#27210 = B_SPLINE_CURVE_WITH_KNOTS ( 'NONE', 3,
 ( #28462, #39078, #47289, #47799 ),
 .UNSPECIFIED., .F., .F.,
 ( 4, 4 ),
 ( 0.1211775127643062860, 0.1625773253007936625 ),
 .UNSPECIFIED. ) ;
#27211 = EDGE_CURVE ( 'NONE', #37648, #47182, #8559, .T. ) ;
#27212 = LINE ( 'NONE', #15351, #50343 ) ;
#27213 = VECTOR ( 'NONE', #10515, 39.37007874015748143 ) ;
#27214 = ORIENTED_EDGE ( 'NONE', *, *, #43191, .F. ) ;
#27215 = CARTESIAN_POINT ( 'NONE',  ( 0.002207914879453961535, -5.712274067634378313E-18, 0.04916304461325374242 ) ) ;
#27216 = VECTOR ( 'NONE', #40738, 39.37007874015748143 ) ;
#27217 = LINE ( 'NONE', #35231, #7179 ) ;
#27218 = CARTESIAN_POINT ( 'NONE',  ( 3.937007874015748143, 2.755905511811027164, 1.181102362204724088 ) ) ;
#27219 = CARTESIAN_POINT ( 'NONE',  ( 1.636583440222563857, 3.346456692913386100, 1.574803149606291974 ) ) ;
#27220 = LINE ( 'NONE', #38356, #23350 ) ;
#27221 = DIRECTION ( 'NONE',  ( 0.000000000000000000, 0.000000000000000000, -1.000000000000000000 ) ) ;
#27222 = ORIENTED_EDGE ( 'NONE', *, *, #188, .T. ) ;
#27223 = CARTESIAN_POINT ( 'NONE',  ( -1.236813753895213086, 1.699986652445209634, -2.681693691597581974 ) ) ;
#27224 = VECTOR ( 'NONE', #13162, 39.37007874015748143 ) ;
#27225 = ORIENTED_EDGE ( 'NONE', *, *, #36722, .T. ) ;
#27226 = DIRECTION ( 'NONE',  ( 0.000000000000000000, 0.000000000000000000, -1.000000000000000000 ) ) ;
#27227 = CARTESIAN_POINT ( 'NONE',  ( 1.363819533518803251, 3.346456692913386100, 0.5905511811023579360 ) ) ;
#27228 = LINE ( 'NONE', #30867, #36718 ) ;
#27229 = VERTEX_POINT ( 'NONE', #15785 ) ;
#27230 = ORIENTED_EDGE ( 'NONE', *, *, #9861, .F. ) ;
#27231 = LINE ( 'NONE', #35248, #34754 ) ;
#27232 = CARTESIAN_POINT ( 'NONE',  ( -1.091055626815042645, 3.346456692913386100, -0.3149606299212593941 ) ) ;
#27233 = EDGE_CURVE ( 'NONE', #4317, #1599, #559, .T. ) ;
#27234 = LINE ( 'NONE', #46827, #1958 ) ;
#27235 = CARTESIAN_POINT ( 'NONE',  ( -0.2042174104418111591, -0.6299212598425202314, -0.3133417129078099328 ) ) ;
#27236 = LINE ( 'NONE', #7630, #1366 ) ;
#27237 = EDGE_CURVE ( 'NONE', #28536, #21352, #39541, .T. ) ;
#27238 = DIRECTION ( 'NONE',  ( -1.000000000000000000, 0.000000000000000000, 1.734723475976806848E-16 ) ) ;
#27239 = EDGE_LOOP ( 'NONE', ( #34866, #6536, #10345, #43076 ) ) ;
#27240 = EDGE_CURVE ( 'NONE', #40680, #47575, #31546, .T. ) ;
#27241 = LINE ( 'NONE', #31905, #22152 ) ;
#27242 = LINE ( 'NONE', #34507, #24130 ) ;
#27243 = ADVANCED_FACE ( 'NONE', ( #23793 ), #47242, .F. ) ;
#27244 = LINE ( 'NONE', #15129, #14143 ) ;
#27245 = ORIENTED_EDGE ( 'NONE', *, *, #47370, .T. ) ;
#27246 = CARTESIAN_POINT ( 'NONE',  ( -1.642191404871911731, 0.000000000000000000, 0.5853255206279681655 ) ) ;
#27247 = VERTEX_POINT ( 'NONE', #47502 ) ;
#27248 = ORIENTED_EDGE ( 'NONE', *, *, #23545, .T. ) ;
#27249 = PLANE ( 'NONE',  #31652 ) ;
#27250 = VECTOR ( 'NONE', #14897, 39.37007874015748143 ) ;
#27251 = AXIS2_PLACEMENT_3D ( 'NONE', #172, #11794, #4065 ) ;
#27252 = EDGE_CURVE ( 'NONE', #44810, #28145, #20680, .T. ) ;
#27253 = ORIENTED_EDGE ( 'NONE', *, *, #2957, .T. ) ;
#27254 = ORIENTED_EDGE ( 'NONE', *, *, #23074, .T. ) ;
#27255 = CARTESIAN_POINT ( 'NONE',  ( 0.5455278134075217666, 3.346456692913386100, 2.204724409448808764 ) ) ;
#27256 = EDGE_LOOP ( 'NONE', ( #32591, #39927, #7818, #22823 ) ) ;
#27257 = ADVANCED_FACE ( 'NONE', ( #43655 ), #35929, .F. ) ;
#27258 = VECTOR ( 'NONE', #26239, 39.37007874015748143 ) ;
#27259 = CARTESIAN_POINT ( 'NONE',  ( 0.000000000000000000, 0.000000000000000000, 0.000000000000000000 ) ) ;
#27260 = DIRECTION ( 'NONE',  ( 1.000000000000000000, 0.000000000000000000, 0.000000000000000000 ) ) ;
#27261 = PLANE ( 'NONE',  #29179 ) ;
#27262 = EDGE_CURVE ( 'NONE', #13018, #49693, #20161, .T. ) ;
#27263 = DIRECTION ( 'NONE',  ( 1.000000000000000000, 0.000000000000000000, 0.000000000000000000 ) ) ;
#27264 = DIRECTION ( 'NONE',  ( -0.9998717552508122886, -0.01601477604151181275, 0.000000000000000000 ) ) ;
#27265 = DIRECTION ( 'NONE',  ( -3.469446951953613696E-16, 0.000000000000000000, -1.000000000000000000 ) ) ;
#27266 = ORIENTED_EDGE ( 'NONE', *, *, #3598, .F. ) ;
#27267 = DIRECTION ( 'NONE',  ( -0.000000000000000000, 1.000000000000000000, -0.000000000000000000 ) ) ;
#27268 = DIRECTION ( 'NONE',  ( -3.469446951953613696E-16, 0.000000000000000000, -1.000000000000000000 ) ) ;
#27269 = LINE ( 'NONE', #43009, #50673 ) ;
#27270 = ADVANCED_FACE ( 'NONE', ( #19654 ), #36444, .F. ) ;
#27271 = DIRECTION ( 'NONE',  ( 0.000000000000000000, 1.000000000000000000, 0.000000000000000000 ) ) ;
#27272 = ORIENTED_EDGE ( 'NONE', *, *, #43736, .F. ) ;
#27273 = CARTESIAN_POINT ( 'NONE',  ( 1.871568535323528293, 0.5220372540190395538, -1.294378953913108754 ) ) ;
#27274 = CARTESIAN_POINT ( 'NONE',  ( -0.8429824507881226170, 1.205361022782829114E-17, -1.637047627937372241 ) ) ;
#27275 = ORIENTED_EDGE ( 'NONE', *, *, #36350, .F. ) ;
#27276 = LINE ( 'NONE', #46622, #32901 ) ;
#27277 = CARTESIAN_POINT ( 'NONE',  ( -1.274276310699785864, 1.035612906144991907, 2.228729129513292495 ) ) ;
#27278 = EDGE_CURVE ( 'NONE', #46126, #23094, #35421, .T. ) ;
#27279 = CARTESIAN_POINT ( 'NONE',  ( 2.223067892362281750, 1.710700052957827788, 0.6705733560908055946 ) ) ;
#27280 = ORIENTED_EDGE ( 'NONE', *, *, #19656, .F. ) ;
#27281 = CARTESIAN_POINT ( 'NONE',  ( -1.909347346926324906, 3.267716535433071279, 3.312189666507128668E-16 ) ) ;
#27282 = ADVANCED_FACE ( 'NONE', ( #39 ), #12427, .F. ) ;
#27283 = CARTESIAN_POINT ( 'NONE',  ( 1.629751586730974422, 1.668388608423060138, -1.626288599946028590 ) ) ;
#27284 = VECTOR ( 'NONE', #33531, 39.37007874015748143 ) ;
#27285 = VECTOR ( 'NONE', #37491, 39.37007874015748143 ) ;
#27286 = DIRECTION ( 'NONE',  ( 3.586865599282270385E-17, -1.000000000000000000, 1.103923720497139891E-16 ) ) ;
#27287 = DIRECTION ( 'NONE',  ( -0.000000000000000000, 1.000000000000000000, -0.000000000000000000 ) ) ;
#27288 = ORIENTED_EDGE ( 'NONE', *, *, #32144, .T. ) ;
#27289 = ORIENTED_EDGE ( 'NONE', *, *, #31102, .T. ) ;
#27290 = ORIENTED_EDGE ( 'NONE', *, *, #32995, .T. ) ;
#27291 = LINE ( 'NONE', #20581, #19605 ) ;
#27292 = VERTEX_POINT ( 'NONE', #36190 ) ;
#27293 = CARTESIAN_POINT ( 'NONE',  ( -0.8190294238272288752, 1.698713383322939530, 2.322353365030251915 ) ) ;
#27294 = CIRCLE ( 'NONE', #19080, 2.165354330708661568 ) ;
#27295 = CARTESIAN_POINT ( 'NONE',  ( -1.363819533518803473, 3.346456692913386100, 1.732283464566920950 ) ) ;
#27296 = ORIENTED_EDGE ( 'NONE', *, *, #44772, .T. ) ;
#27297 = EDGE_CURVE ( 'NONE', #49569, #40529, #48272, .T. ) ;
#27298 = LINE ( 'NONE', #35825, #28073 ) ;
#27299 = AXIS2_PLACEMENT_3D ( 'NONE', #28297, #16694, #8683 ) ;
#27300 = EDGE_LOOP ( 'NONE', ( #37302, #39045 ) ) ;
#27301 = CARTESIAN_POINT ( 'NONE',  ( -0.3486774197067334935, 3.267716535433071279, 1.062992125984246083 ) ) ;
#27302 = EDGE_CURVE ( 'NONE', #11317, #30078, #24561, .T. ) ;
#27303 = ORIENTED_EDGE ( 'NONE', *, *, #36592, .F. ) ;
#27304 = ORIENTED_EDGE ( 'NONE', *, *, #27757, .T. ) ;
#27305 = PLANE ( 'NONE',  #37272 ) ;
#27306 = VERTEX_POINT ( 'NONE', #16046 ) ;
#27307 = DIRECTION ( 'NONE',  ( -0.000000000000000000, 1.000000000000000000, 0.000000000000000000 ) ) ;
#27308 = ORIENTED_EDGE ( 'NONE', *, *, #27878, .T. ) ;
#27309 = ORIENTED_EDGE ( 'NONE', *, *, #33529, .T. ) ;
#27310 = CARTESIAN_POINT ( 'NONE',  ( -0.9794755770252101534, 0.4349011127721510994, 1.097585813245683051 ) ) ;
#27311 = DIRECTION ( 'NONE',  ( 0.5773502691896245098, 0.5773502691896259531, -0.5773502691896270633 ) ) ;
#27312 = ORIENTED_EDGE ( 'NONE', *, *, #17875, .F. ) ;
#27313 = DIRECTION ( 'NONE',  ( -1.000000000000000000, 0.000000000000000000, -0.000000000000000000 ) ) ;
#27314 = ORIENTED_EDGE ( 'NONE', *, *, #43700, .T. ) ;
#27315 = CARTESIAN_POINT ( 'NONE',  ( 2.277873973731426638, 1.463603380278871713, 1.879489153247667632 ) ) ;
#27316 = VECTOR ( 'NONE', #47878, 39.37007874015748854 ) ;
#27317 = LINE ( 'NONE', #11082, #18433 ) ;
#27318 = CONICAL_SURFACE ( 'NONE', #5080, 2.244934639244524632, 1.554780866114618743 ) ;
#27319 = ADVANCED_FACE ( 'NONE', ( #31805 ), #40322, .F. ) ;
#27320 = FACE_OUTER_BOUND ( 'NONE', #38482, .T. ) ;
#27321 = ORIENTED_EDGE ( 'NONE', *, *, #21195, .F. ) ;
#27322 = ORIENTED_EDGE ( 'NONE', *, *, #31878, .T. ) ;
#27323 = AXIS2_PLACEMENT_3D ( 'NONE', #14870, #30613, #46331 ) ;
#27324 = PLANE ( 'NONE',  #17869 ) ;
#27325 = CARTESIAN_POINT ( 'NONE',  ( -0.07591351300297284610, 0.000000000000000000, 1.850393700787392293 ) ) ;
#27326 = LINE ( 'NONE', #18840, #6861 ) ;
#27327 = CIRCLE ( 'NONE', #5088, 2.165354330708661568 ) ;
#27328 = CARTESIAN_POINT ( 'NONE',  ( 2.808237744965994320, 0.000000000000000000, 0.9124517550441679781 ) ) ;
#27329 = EDGE_CURVE ( 'NONE', #48815, #36606, #37214, .T. ) ;
#27330 = FACE_OUTER_BOUND ( 'NONE', #39186, .T. ) ;
#27331 = VECTOR ( 'NONE', #36761, 39.37007874015748143 ) ;
#27332 = EDGE_CURVE ( 'NONE', #25208, #37754, #21461, .T. ) ;
#27333 = DIRECTION ( 'NONE',  ( -0.9998717552508122886, -0.01601477604151182316, 0.000000000000000000 ) ) ;
#27334 = ORIENTED_EDGE ( 'NONE', *, *, #9534, .T. ) ;
#27335 = EDGE_CURVE ( 'NONE', #41731, #19367, #32842, .T. ) ;
#27336 = DIRECTION ( 'NONE',  ( 0.6910626489868684219, 0.000000000000000000, -0.7227948638273878901 ) ) ;
#27337 = ORIENTED_EDGE ( 'NONE', *, *, #33400, .T. ) ;
#27338 = CARTESIAN_POINT ( 'NONE',  ( 2.823445274216730638, 1.205361022782829114E-17, 0.8656477926280680135 ) ) ;
#27339 = ORIENTED_EDGE ( 'NONE', *, *, #23407, .T. ) ;
#27340 = ORIENTED_EDGE ( 'NONE', *, *, #17975, .T. ) ;
#27341 = FACE_OUTER_BOUND ( 'NONE', #42407, .T. ) ;
#27342 = LINE ( 'NONE', #43082, #40236 ) ;
#27343 = EDGE_LOOP ( 'NONE', ( #41375, #8072, #46724, #31016 ) ) ;
#27344 = ADVANCED_FACE ( 'NONE', ( #33605 ), #1583, .F. ) ;
#27345 = CARTESIAN_POINT ( 'NONE',  ( -1.880560108260527885, 1.049866565067837598, -0.7502705391232876719 ) ) ;
#27346 = EDGE_LOOP ( 'NONE', ( #33860, #11396, #48798, #12856 ) ) ;
#27347 = CARTESIAN_POINT ( 'NONE',  ( 3.927031490892378253E-16, 3.346456692913386100, 1.692913385826762873 ) ) ;
#27348 = ORIENTED_EDGE ( 'NONE', *, *, #38710, .T. ) ;
#27349 = AXIS2_PLACEMENT_3D ( 'NONE', #50907, #47813, #20226 ) ;
#27350 = EDGE_CURVE ( 'NONE', #26630, #1152, #22123, .T. ) ;
#27351 = CARTESIAN_POINT ( 'NONE',  ( 0.4696143004045476022, 3.346456692913386100, -1.929133858267710000 ) ) ;
#27352 = LINE ( 'NONE', #43094, #13243 ) ;
#27353 = AXIS2_PLACEMENT_3D ( 'NONE', #35702, #330, #18944 ) ;
#27354 = ADVANCED_FACE ( 'NONE', ( #5715 ), #20946, .F. ) ;
#27355 = VERTEX_POINT ( 'NONE', #44675 ) ;
#27356 = VECTOR ( 'NONE', #43420, 39.37007874015748143 ) ;
#27357 = CARTESIAN_POINT ( 'NONE',  ( -1.363819533518803029, 3.346456692913386100, 0.4724409448818871482 ) ) ;
#27358 = ORIENTED_EDGE ( 'NONE', *, *, #49196, .T. ) ;
#27359 = VERTEX_POINT ( 'NONE', #5454 ) ;
#27360 = CARTESIAN_POINT ( 'NONE',  ( 0.5756566573088583993, 1.728235332270611879, 2.896516654582643291 ) ) ;
#27362 = DIRECTION ( 'NONE',  ( -3.469446951953613696E-16, 0.000000000000000000, -1.000000000000000000 ) ) ;
#27361 = VECTOR ( 'NONE', #41685, 39.37007874015748143 ) ;
#27363 = CARTESIAN_POINT ( 'NONE',  ( 0.000000000000000000, 3.267716535433071279, 1.102362204724404160 ) ) ;
#27364 = VECTOR ( 'NONE', #34293, 39.37007874015748143 ) ;
#27365 = EDGE_LOOP ( 'NONE', ( #32328, #3447, #5266, #38825 ) ) ;
#27366 = LINE ( 'NONE', #15005, #11375 ) ;
#27367 = DIRECTION ( 'NONE',  ( -3.469446951953613696E-16, 0.000000000000000000, -1.000000000000000000 ) ) ;
#27368 = ORIENTED_EDGE ( 'NONE', *, *, #26409, .T. ) ;
#27369 = CARTESIAN_POINT ( 'NONE',  ( -0.07591351300297333182, 3.346456692913386100, 2.362204724409437961 ) ) ;
#27370 = EDGE_LOOP ( 'NONE', ( #8265, #42961, #21142, #10256 ) ) ;
#27371 = VERTEX_POINT ( 'NONE', #9072 ) ;
#27372 = ORIENTED_EDGE ( 'NONE', *, *, #21310, .T. ) ;
#27373 = CARTESIAN_POINT ( 'NONE',  ( 0.002207914879453961535, -5.712274067634378313E-18, 0.04916304461325374242 ) ) ;
#27374 = CARTESIAN_POINT ( 'NONE',  ( -0.2727639067037608278, 3.346456692913386100, -0.9842519685039344823 ) ) ;
#27375 = DIRECTION ( 'NONE',  ( -0.000000000000000000, -1.000000000000000000, -0.000000000000000000 ) ) ;
#27376 = DIRECTION ( 'NONE',  ( 1.734723475976806848E-16, -0.000000000000000000, 1.000000000000000000 ) ) ;
#27377 = ORIENTED_EDGE ( 'NONE', *, *, #8108, .T. ) ;
#27378 = ORIENTED_EDGE ( 'NONE', *, *, #11354, .F. ) ;
#27379 = DIRECTION ( 'NONE',  ( -0.000000000000000000, 1.000000000000000000, -0.000000000000000000 ) ) ;
#27380 = ORIENTED_EDGE ( 'NONE', *, *, #29575, .F. ) ;
#27381 = DIRECTION ( 'NONE',  ( 0.000000000000000000, 0.000000000000000000, 1.000000000000000000 ) ) ;
#27382 = DIRECTION ( 'NONE',  ( 0.000000000000000000, 0.000000000000000000, 1.000000000000000000 ) ) ;
#27383 = CARTESIAN_POINT ( 'NONE',  ( 2.182111253630085290, 3.267716535433071279, 0.3149606299212573401 ) ) ;
#27384 = VECTOR ( 'NONE', #47469, 39.37007874015748143 ) ;
#27385 = EDGE_CURVE ( 'NONE', #30240, #30125, #20925, .T. ) ;
#27386 = EDGE_CURVE ( 'NONE', #13855, #33190, #33856, .T. ) ;
#27387 = CARTESIAN_POINT ( 'NONE',  ( -1.363819533518803473, 3.346456692913386100, -1.732283464566922726 ) ) ;
#27388 = EDGE_CURVE ( 'NONE', #31389, #23409, #50055, .T. ) ;
#27389 = CARTESIAN_POINT ( 'NONE',  ( 1.128560816269277955, 1.725977917706353670, 1.984842472008916170 ) ) ;
#27391 = DIRECTION ( 'NONE',  ( -0.000000000000000000, 1.000000000000000000, -0.000000000000000000 ) ) ;
#27390 = VECTOR ( 'NONE', #27809, 39.37007874015748143 ) ;
#27392 = ORIENTED_EDGE ( 'NONE', *, *, #38383, .T. ) ;
#27393 = CARTESIAN_POINT ( 'NONE',  ( 0.4506430153629077950, 0.03513753811042658048, -1.817852439337431569 ) ) ;
#27394 = CARTESIAN_POINT ( 'NONE',  ( -1.536664496436148184E-16, 3.267716535433071279, -0.5118110236220465570 ) ) ;
#27395 = B_SPLINE_CURVE_WITH_KNOTS ( 'NONE', 3,
 ( #49973, #34033, #49217, #14145 ),
 .UNSPECIFIED., .F., .F.,
 ( 4, 4 ),
 ( 0.0001198035261475026192, 0.0009683180137351917165 ),
 .UNSPECIFIED. ) ;
#27396 = VECTOR ( 'NONE', #47539, 39.37007874015748143 ) ;
#27397 = VERTEX_POINT ( 'NONE', #29458 ) ;
#27398 = AXIS2_PLACEMENT_3D ( 'NONE', #13130, #46977, #27381 ) ;
#27400 = ADVANCED_FACE ( 'NONE', ( #44430 ), #40569, .F. ) ;
#27399 = EDGE_LOOP ( 'NONE', ( #24002, #45952, #402, #5896 ) ) ;
#27401 = AXIS2_PLACEMENT_3D ( 'NONE', #20928, #12934, #44410 ) ;
#27402 = CARTESIAN_POINT ( 'NONE',  ( 0.000000000000000000, 1.574803149606302854, 0.000000000000000000 ) ) ;
#27403 = CARTESIAN_POINT ( 'NONE',  ( 1.037524086854322514, 0.000000000000000000, 2.764473043227584803 ) ) ;
#27404 = DIRECTION ( 'NONE',  ( 0.000000000000000000, 1.000000000000000000, 0.000000000000000000 ) ) ;
#27405 = VERTEX_POINT ( 'NONE', #33351 ) ;
#27406 = ORIENTED_EDGE ( 'NONE', *, *, #34331, .T. ) ;
#27407 = LINE ( 'NONE', #35677, #14706 ) ;
#27409 = VERTEX_POINT ( 'NONE', #21716 ) ;
#27408 = EDGE_CURVE ( 'NONE', #23850, #12580, #17084, .T. ) ;
#27410 = LINE ( 'NONE', #42899, #47634 ) ;
#27411 = VERTEX_POINT ( 'NONE', #28938 ) ;
#27412 = DIRECTION ( 'NONE',  ( 1.734723475976806848E-16, -0.000000000000000000, 1.000000000000000000 ) ) ;
#27413 = ADVANCED_FACE ( 'NONE', ( #40825 ), #13719, .F. ) ;
#27414 = CARTESIAN_POINT ( 'NONE',  ( 2.106197740627112402, 3.346456692913386100, -0.5026832550384014997 ) ) ;
#27415 = LINE ( 'NONE', #26662, #39209 ) ;
#27416 = EDGE_CURVE ( 'NONE', #19878, #47775, #9584, .T. ) ;
#27417 = VERTEX_POINT ( 'NONE', #10094 ) ;
#27418 = ORIENTED_EDGE ( 'NONE', *, *, #2777, .T. ) ;
#27419 = ORIENTED_EDGE ( 'NONE', *, *, #4544, .T. ) ;
#27420 = DIRECTION ( 'NONE',  ( -0.000000000000000000, 1.000000000000000000, -0.000000000000000000 ) ) ;
#27421 = DIRECTION ( 'NONE',  ( -0.000000000000000000, 1.000000000000000000, -0.000000000000000000 ) ) ;
#27423 = ORIENTED_EDGE ( 'NONE', *, *, #27137, .T. ) ;
#27422 = EDGE_CURVE ( 'NONE', #10879, #49655, #44861, .T. ) ;
#27424 = ORIENTED_EDGE ( 'NONE', *, *, #17978, .F. ) ;
#27425 = DIRECTION ( 'NONE',  ( 1.000000000000000000, -0.000000000000000000, 0.000000000000000000 ) ) ;
#27426 = CARTESIAN_POINT ( 'NONE',  ( -1.363819533518803473, 0.000000000000000000, -1.417322834645664109 ) ) ;
#27427 = CARTESIAN_POINT ( 'NONE',  ( -2.454875160333845674, 3.346456692913386100, 0.1574803149606286423 ) ) ;
#27428 = EDGE_CURVE ( 'NONE', #24184, #12127, #29715, .T. ) ;
#27429 = EDGE_LOOP ( 'NONE', ( #3109, #27653, #12147, #36226 ) ) ;
#27430 = ORIENTED_EDGE ( 'NONE', *, *, #44067, .F. ) ;
#27431 = DIRECTION ( 'NONE',  ( -3.469446951953613696E-16, 0.000000000000000000, -1.000000000000000000 ) ) ;
#27432 = DIRECTION ( 'NONE',  ( 1.734723475976806848E-16, 0.000000000000000000, 1.000000000000000000 ) ) ;
#27433 = CARTESIAN_POINT ( 'NONE',  ( 1.363819533518803251, 3.267716535433071279, -2.365849761790805487E-16 ) ) ;
#27434 = EDGE_LOOP ( 'NONE', ( #47293, #47710, #42896 ) ) ;
#27435 = CARTESIAN_POINT ( 'NONE',  ( -1.626937427625217314, 1.689925977444973304, -2.155561787858257361 ) ) ;
#27436 = AXIS2_PLACEMENT_3D ( 'NONE', #34192, #18941, #42427 ) ;
#27437 = LINE ( 'NONE', #4974, #12869 ) ;
#27438 = ORIENTED_EDGE ( 'NONE', *, *, #12488, .T. ) ;
#27439 = DIRECTION ( 'NONE',  ( -0.9998717552508122886, -0.01601477604151182316, 0.000000000000000000 ) ) ;
#27440 = ORIENTED_EDGE ( 'NONE', *, *, #40019, .F. ) ;
#27441 = ORIENTED_EDGE ( 'NONE', *, *, #22487, .F. ) ;
#27442 = CARTESIAN_POINT ( 'NONE',  ( 1.687984952120843207, 3.267716535433071279, -1.259842519685035800 ) ) ;
#27443 = DIRECTION ( 'NONE',  ( 3.586865599282270385E-17, -1.000000000000000000, 1.103923720497139891E-16 ) ) ;
#27444 = VECTOR ( 'NONE', #2384, 39.37007874015748143 ) ;
#27445 = CONICAL_SURFACE ( 'NONE', #47193, 3.033577403570480779, 1.554780866114618743 ) ;
#27446 = B_SPLINE_CURVE_WITH_KNOTS ( 'NONE', 3,
 ( #25317, #47998, #32309, #36953 ),
 .UNSPECIFIED., .F., .F.,
 ( 4, 4 ),
 ( 0.1211873102087489551, 0.1625992483279400380 ),
 .UNSPECIFIED. ) ;
#27447 = LINE ( 'NONE', #18953, #37120 ) ;
#27448 = CARTESIAN_POINT ( 'NONE',  ( -1.979793062125317693, 1.688404340953838068, 2.191257344206539504 ) ) ;
#27449 = LINE ( 'NONE', #27702, #37047 ) ;
#27450 = ORIENTED_EDGE ( 'NONE', *, *, #38437, .T. ) ;
#27451 = EDGE_LOOP ( 'NONE', ( #45607, #33752, #40045, #11941 ) ) ;
#27452 = CIRCLE ( 'NONE', #11791, 1.850107469027523432 ) ;
#27453 = ORIENTED_EDGE ( 'NONE', *, *, #39324, .F. ) ;
#27454 = CARTESIAN_POINT ( 'NONE',  ( 0.000000000000000000, 0.000000000000000000, -1.220472440944881942 ) ) ;
#27455 = ADVANCED_FACE ( 'NONE', ( #38235 ), #18605, .T. ) ;
#27456 = CYLINDRICAL_SURFACE ( 'NONE', #7107, 2.164630168518208109 ) ;
#27457 = CARTESIAN_POINT ( 'NONE',  ( 1.287906020515830141, 3.346456692913386100, -0.5118110236220471121 ) ) ;
#27458 = ORIENTED_EDGE ( 'NONE', *, *, #40456, .T. ) ;
#27459 = EDGE_CURVE ( 'NONE', #18566, #456, #26989, .T. ) ;
#27460 = CARTESIAN_POINT ( 'NONE',  ( 0.5756566573088586214, 1.205361022782829114E-17, 2.896516654582643291 ) ) ;
#27461 = DIRECTION ( 'NONE',  ( 1.000000000000000000, 0.000000000000000000, -3.469446951953613696E-16 ) ) ;
#27462 = EDGE_CURVE ( 'NONE', #17026, #6745, #30481, .T. ) ;
#27463 = VERTEX_POINT ( 'NONE', #10850 ) ;
#27464 = DIRECTION ( 'NONE',  ( -0.9510565162951500895, 0.000000000000000000, -0.3090169943749582204 ) ) ;
#27465 = CARTESIAN_POINT ( 'NONE',  ( 2.324843851831239760, 1.712330180919884315, -0.05514665559127426842 ) ) ;
#27466 = CARTESIAN_POINT ( 'NONE',  ( 0.8182917201112824834, 3.267716535433071279, 1.417322834645662777 ) ) ;
#27467 = EDGE_LOOP ( 'NONE', ( #37939, #39150, #47390, #38400 ) ) ;
#27468 = DIRECTION ( 'NONE',  ( 1.734723475976806848E-16, -0.000000000000000000, 1.000000000000000000 ) ) ;
#27469 = DIRECTION ( 'NONE',  ( -6.394449067488625930E-17, -1.000000000000000000, 9.687176266499597757E-17 ) ) ;
#27470 = CARTESIAN_POINT ( 'NONE',  ( -1.166969139818015533, 3.346456692913386100, 0.1574803149606287811 ) ) ;
#27471 = VECTOR ( 'NONE', #42859, 39.37007874015748143 ) ;
#27472 = ORIENTED_EDGE ( 'NONE', *, *, #37933, .F. ) ;
#27473 = AXIS2_PLACEMENT_3D ( 'NONE', #6726, #50290, #17392 ) ;
#27474 = DIRECTION ( 'NONE',  ( -0.000000000000000000, 1.000000000000000000, -0.000000000000000000 ) ) ;
#27475 = ORIENTED_EDGE ( 'NONE', *, *, #44190, .T. ) ;
#27476 = FACE_OUTER_BOUND ( 'NONE', #46596, .T. ) ;
#27477 = AXIS2_PLACEMENT_3D ( 'NONE', #38461, #19318, #10824 ) ;
#27478 = AXIS2_PLACEMENT_3D ( 'NONE', #9636, #1629, #17379 ) ;
#27479 = PLANE ( 'NONE',  #33410 ) ;
#27480 = ADVANCED_FACE ( 'NONE', ( #42835 ), #22728, .F. ) ;
#27481 = LINE ( 'NONE', #34990, #19369 ) ;
#27482 = VERTEX_POINT ( 'NONE', #22476 ) ;
#27483 = ORIENTED_EDGE ( 'NONE', *, *, #15333, .F. ) ;
#27484 = PLANE ( 'NONE',  #10860 ) ;
#27485 = AXIS2_PLACEMENT_3D ( 'NONE', #44731, #9381, #41388 ) ;
#27486 = DIRECTION ( 'NONE',  ( -0.000000000000000000, 1.000000000000000000, -0.000000000000000000 ) ) ;
#27487 = EDGE_CURVE ( 'NONE', #45462, #43417, #14728, .T. ) ;
#27488 = EDGE_CURVE ( 'NONE', #19566, #32968, #26589, .T. ) ;
#27489 = ORIENTED_EDGE ( 'NONE', *, *, #34769, .F. ) ;
#27490 = CARTESIAN_POINT ( 'NONE',  ( 0.000000000000000000, 6.692913385826772199, 0.000000000000000000 ) ) ;
#27491 = PLANE ( 'NONE',  #18653 ) ;
#27492 = LINE ( 'NONE', #7879, #23583 ) ;
#27493 = CARTESIAN_POINT ( 'NONE',  ( -1.112911385528784214, 0.4042499682059492172, -0.9948011493083117607 ) ) ;
#27494 = ORIENTED_EDGE ( 'NONE', *, *, #33792, .T. ) ;
#27495 = EDGE_LOOP ( 'NONE', ( #47822, #26670, #45240, #40995 ) ) ;
#27496 = DIRECTION ( 'NONE',  ( -0.000000000000000000, 1.000000000000000000, -0.000000000000000000 ) ) ;
#27497 = DIRECTION ( 'NONE',  ( 3.986037398843765983E-20, 1.000000000000000000, 1.160734090543304660E-16 ) ) ;
#27498 = ORIENTED_EDGE ( 'NONE', *, *, #6212, .T. ) ;
#27499 = DIRECTION ( 'NONE',  ( 0.000000000000000000, 0.000000000000000000, -1.000000000000000000 ) ) ;
#27500 = ORIENTED_EDGE ( 'NONE', *, *, #6394, .F. ) ;
#27501 = ORIENTED_EDGE ( 'NONE', *, *, #32940, .F. ) ;
#27502 = LINE ( 'NONE', #2310, #6924 ) ;
#27503 = ORIENTED_EDGE ( 'NONE', *, *, #33854, .T. ) ;
#27504 = ORIENTED_EDGE ( 'NONE', *, *, #23970, .T. ) ;
#27505 = CARTESIAN_POINT ( 'NONE',  ( -0.8942052331142547050, 3.267716535433071279, 0.4330708661417290162 ) ) ;
#27506 = ORIENTED_EDGE ( 'NONE', *, *, #2417, .F. ) ;
#27507 = VECTOR ( 'NONE', #1169, 39.37007874015748854 ) ;
#27508 = CONICAL_SURFACE ( 'NONE', #18468, 1.850107469027523210, 0.6386652850508578450 ) ;
#27509 = CARTESIAN_POINT ( 'NONE',  ( 4.200216290258821831E-16, 3.267716535433071279, 2.165354330708661568 ) ) ;
#27510 = LINE ( 'NONE', #24165, #11237 ) ;
#27511 = CARTESIAN_POINT ( 'NONE',  ( 0.4930719867878015084, 1.719503719051284074, 2.441437611110367278 ) ) ;
#27512 = VECTOR ( 'NONE', #21539, 39.37007874015748143 ) ;
#27513 = VECTOR ( 'NONE', #13960, 39.37007874015748143 ) ;
#27514 = CARTESIAN_POINT ( 'NONE',  ( 0.8182917201112821504, 3.267716535433071279, -1.419509857074483539E-16 ) ) ;
#27515 = EDGE_CURVE ( 'NONE', #47004, #11192, #27035, .T. ) ;
#27516 = CARTESIAN_POINT ( 'NONE',  ( -0.3486774197067343262, 3.267716535433071279, -2.401574803149598036 ) ) ;
#27517 = CARTESIAN_POINT ( 'NONE',  ( 1.393175312147112432, 0.000000000000000000, 1.048074961516293202 ) ) ;
#27518 = CONICAL_SURFACE ( 'NONE', #25069, 3.033577403570480779, 1.554780866114618743 ) ;
#27519 = ORIENTED_EDGE ( 'NONE', *, *, #30405, .T. ) ;
#27520 = EDGE_CURVE ( 'NONE', #36182, #27786, #14471, .T. ) ;
#27521 = CARTESIAN_POINT ( 'NONE',  ( 0.000000000000000000, 3.267716535433071279, -0.3149606299212596716 ) ) ;
#27522 = FACE_OUTER_BOUND ( 'NONE', #48846, .T. ) ;
#27523 = DIRECTION ( 'NONE',  ( -1.000000000000000000, 0.000000000000000000, 0.000000000000000000 ) ) ;
#27524 = EDGE_CURVE ( 'NONE', #4242, #3379, #49536, .T. ) ;
#27525 = ORIENTED_EDGE ( 'NONE', *, *, #16352, .F. ) ;
#27526 = CARTESIAN_POINT ( 'NONE',  ( 0.4696143004045476022, 3.267716535433071279, -1.929133858267710000 ) ) ;
#27527 = ADVANCED_FACE ( 'NONE', ( #29968 ), #42595, .F. ) ;
#27528 = DIRECTION ( 'NONE',  ( 0.000000000000000000, -1.000000000000000000, -0.000000000000000000 ) ) ;
#27529 = ORIENTED_EDGE ( 'NONE', *, *, #255, .F. ) ;
#27530 = CARTESIAN_POINT ( 'NONE',  ( -2.182111253630085290, 3.267716535433071279, 0.6299212598425164567 ) ) ;
#27531 = EDGE_CURVE ( 'NONE', #29523, #22090, #23222, .T. ) ;
#27532 = CARTESIAN_POINT ( 'NONE',  ( 0.04921259842519669359, 1.610264983814881479, 2.246280244424690320 ) ) ;
#27533 = CARTESIAN_POINT ( 'NONE',  ( -2.952069331832154919, 2.755905511811027164, 1.181102362204724088 ) ) ;
#27534 = CARTESIAN_POINT ( 'NONE',  ( -1.712496953225537633, 3.267716535433071279, -0.9842519685039344823 ) ) ;
#27535 = ORIENTED_EDGE ( 'NONE', *, *, #34491, .T. ) ;
#27536 = CARTESIAN_POINT ( 'NONE',  ( 0.07982360342473591996, 1.709180471932028711, 0.000000000000000000 ) ) ;
#27537 = DIRECTION ( 'NONE',  ( 1.734723475976806848E-16, -0.000000000000000000, 1.000000000000000000 ) ) ;
#27538 = B_SPLINE_CURVE_WITH_KNOTS ( 'NONE', 3,
 ( #24998, #43836, #23974, #12357 ),
 .UNSPECIFIED., .F., .F.,
 ( 4, 4 ),
 ( 0.01409236801188419770, 0.03074671883294705782 ),
 .UNSPECIFIED. ) ;
#27539 = CARTESIAN_POINT ( 'NONE',  ( 2.708693820787337891, 1.761460031494409550, -1.175591050816825023 ) ) ;
#27540 = ADVANCED_FACE ( 'NONE', ( #3610 ), #3102, .T. ) ;
#27541 = FACE_OUTER_BOUND ( 'NONE', #17223, .T. ) ;
#27542 = ORIENTED_EDGE ( 'NONE', *, *, #48244, .F. ) ;
#27543 = ORIENTED_EDGE ( 'NONE', *, *, #16564, .T. ) ;
#27544 = ORIENTED_EDGE ( 'NONE', *, *, #49540, .T. ) ;
#27545 = AXIS2_PLACEMENT_3D ( 'NONE', #19630, #31783, #17 ) ;
#27546 = CARTESIAN_POINT ( 'NONE',  ( 0.000000000000000000, 3.346456692913386100, 0.000000000000000000 ) ) ;
#27547 = ORIENTED_EDGE ( 'NONE', *, *, #34593, .T. ) ;
#27548 = ADVANCED_FACE ( 'NONE', ( #45939 ), #26093, .F. ) ;
#27549 = CARTESIAN_POINT ( 'NONE',  ( 0.04921259842519670746, 1.514263714023589502, 2.952755905511811108 ) ) ;
#27550 = DIRECTION ( 'NONE',  ( -0.01601477604151182663, 0.9998717552508123996, -0.000000000000000000 ) ) ;
#27551 = ORIENTED_EDGE ( 'NONE', *, *, #18587, .T. ) ;
#27552 = AXIS2_PLACEMENT_3D ( 'NONE', #49479, #41280, #10286 ) ;
#27553 = VECTOR ( 'NONE', #31675, 39.37007874015748143 ) ;
#27554 = CARTESIAN_POINT ( 'NONE',  ( 1.277153579995027988, 3.261691961121675920, -2.086614173228339641 ) ) ;
#27555 = ORIENTED_EDGE ( 'NONE', *, *, #34206, .F. ) ;
#27556 = EDGE_CURVE ( 'NONE', #32615, #19355, #15230, .T. ) ;
#27557 = LINE ( 'NONE', #22935, #3463 ) ;
#27558 = DIRECTION ( 'NONE',  ( -3.469446951953613696E-16, 0.000000000000000000, -1.000000000000000000 ) ) ;
#27559 = VECTOR ( 'NONE', #17773, 39.37007874015748143 ) ;
#27560 = ORIENTED_EDGE ( 'NONE', *, *, #45027, .T. ) ;
#27561 = EDGE_LOOP ( 'NONE', ( #22178, #4887, #35163, #24921 ) ) ;
#27562 = CARTESIAN_POINT ( 'NONE',  ( -1.299212598425205423, 3.346456692913386100, -1.732283464566922726 ) ) ;
#27563 = EDGE_LOOP ( 'NONE', ( #19728, #21935, #16523, #44103 ) ) ;
#27564 = EDGE_CURVE ( 'NONE', #36460, #12460, #46688, .T. ) ;
#27565 = CARTESIAN_POINT ( 'NONE',  ( 1.921114995622270172, 0.9943725288147066133, -1.768687470589421995 ) ) ;
#27566 = ORIENTED_EDGE ( 'NONE', *, *, #48197, .F. ) ;
#27567 = ORIENTED_EDGE ( 'NONE', *, *, #18395, .F. ) ;
#27568 = DIRECTION ( 'NONE',  ( 1.000000000000000000, 0.000000000000000000, 0.000000000000000000 ) ) ;
#27569 = DIRECTION ( 'NONE',  ( -0.000000000000000000, 1.000000000000000000, -0.000000000000000000 ) ) ;
#27570 = ORIENTED_EDGE ( 'NONE', *, *, #16930, .T. ) ;
#27571 = CARTESIAN_POINT ( 'NONE',  ( -2.454875160333845674, 3.232777166330581320, -0.1574803149606298636 ) ) ;
#27572 = ORIENTED_EDGE ( 'NONE', *, *, #40317, .T. ) ;
#27573 = CARTESIAN_POINT ( 'NONE',  ( 1.662320194739497659, 0.000000000000000000, -1.388601395075552025 ) ) ;
#27574 = DIRECTION ( 'NONE',  ( 1.000000000000000000, 0.000000000000000000, 0.000000000000000000 ) ) ;
#27575 = CARTESIAN_POINT ( 'NONE',  ( 2.106197740627111514, 3.267716535433071279, -1.102362204724406602 ) ) ;
#27576 = ORIENTED_EDGE ( 'NONE', *, *, #2955, .F. ) ;
#27577 = VERTEX_POINT ( 'NONE', #27091 ) ;
#27578 =( REPRESENTATION_RELATIONSHIP ('NONE','NONE', #50198, #36385 ) REPRESENTATION_RELATIONSHIP_WITH_TRANSFORMATION ( #47983 )SHAPE_REPRESENTATION_RELATIONSHIP( ) );
#27579 = FACE_OUTER_BOUND ( 'NONE', #9239, .T. ) ;
#27580 = DIRECTION ( 'NONE',  ( 1.000000000000000000, -0.000000000000000000, 0.000000000000000000 ) ) ;
#27581 = VECTOR ( 'NONE', #15595, 39.37007874015748143 ) ;
#27582 = CARTESIAN_POINT ( 'NONE',  ( 1.006250229852934774, 3.267716535433071279, 1.850393700787392293 ) ) ;
#27583 = AXIS2_PLACEMENT_3D ( 'NONE', #14519, #29754, #33895 ) ;
#27584 = DIRECTION ( 'NONE',  ( -3.469446951953613696E-16, 0.000000000000000000, -1.000000000000000000 ) ) ;
#27585 = CONICAL_SURFACE ( 'NONE', #8619, 2.246510896728926010, 0.01601546068027819014 ) ;
#27586 = DIRECTION ( 'NONE',  ( -0.01601477604151182663, 0.9998717552508123996, -0.000000000000000000 ) ) ;
#27587 = EDGE_CURVE ( 'NONE', #37294, #48631, #19343, .T. ) ;
#27588 = CARTESIAN_POINT ( 'NONE',  ( 1.083598637574782364, 1.205361022782829114E-17, 2.747180975113346246 ) ) ;
#27589 = ORIENTED_EDGE ( 'NONE', *, *, #46916, .T. ) ;
#27590 = EDGE_CURVE ( 'NONE', #31865, #5433, #36942, .T. ) ;
#27591 = DIRECTION ( 'NONE',  ( -0.01601477604151182663, 0.9998717552508123996, -0.000000000000000000 ) ) ;
#27592 = VECTOR ( 'NONE', #32294, 39.37007874015748143 ) ;
#27593 = ORIENTED_EDGE ( 'NONE', *, *, #18071, .F. ) ;
#27594 = DIRECTION ( 'NONE',  ( 1.000000000000000000, 0.000000000000000000, -3.469446951953613696E-16 ) ) ;
#27595 = VERTEX_POINT ( 'NONE', #2599 ) ;
#27596 = DIRECTION ( 'NONE',  ( -0.9639628606958550172, 1.288287287306305283E-16, 0.2660368455666688448 ) ) ;
#27597 = DIRECTION ( 'NONE',  ( -0.3513748240813434620, 0.000000000000000000, 0.9362348706397368714 ) ) ;
#27598 = ORIENTED_EDGE ( 'NONE', *, *, #4523, .F. ) ;
#27599 = DIRECTION ( 'NONE',  ( -3.469446951953613696E-16, 0.000000000000000000, -1.000000000000000000 ) ) ;
#27600 = ORIENTED_EDGE ( 'NONE', *, *, #50660, .T. ) ;
#27601 = CARTESIAN_POINT ( 'NONE',  ( -0.2727639067037611054, 0.000000000000000000, -2.244094488188968395 ) ) ;
#27602 = ORIENTED_EDGE ( 'NONE', *, *, #28273, .F. ) ;
#27603 = CARTESIAN_POINT ( 'NONE',  ( -2.106299212598425008, 3.346456692913386100, -6.146657985744592735E-16 ) ) ;
#27604 = DIRECTION ( 'NONE',  ( 1.000000000000000000, -0.000000000000000000, 0.000000000000000000 ) ) ;
#27605 = ADVANCED_FACE ( 'NONE', ( #3863 ), #39383, .T. ) ;
#27606 = ORIENTED_EDGE ( 'NONE', *, *, #23702, .T. ) ;
#27607 = CARTESIAN_POINT ( 'NONE',  ( -1.083598637574821222, 5.905511811023623103, 2.747180975113331147 ) ) ;
#27608 = VECTOR ( 'NONE', #16290, 39.37007874015748143 ) ;
#27609 = ORIENTED_EDGE ( 'NONE', *, *, #46266, .F. ) ;
#27610 = VERTEX_POINT ( 'NONE', #15485 ) ;
#27611 = VECTOR ( 'NONE', #12135, 39.37007874015748143 ) ;
#27612 = AXIS2_PLACEMENT_3D ( 'NONE', #36374, #27843, #4363 ) ;
#27613 = CARTESIAN_POINT ( 'NONE',  ( -2.145573069066419425, 1.685811222653325059, -2.028682512764306445 ) ) ;
#27614 = LINE ( 'NONE', #15502, #19875 ) ;
#27615 = DIRECTION ( 'NONE',  ( 1.734723475976806848E-16, -0.000000000000000000, 1.000000000000000000 ) ) ;
#27616 = EDGE_CURVE ( 'NONE', #47811, #27355, #44111, .T. ) ;
#27617 = ORIENTED_EDGE ( 'NONE', *, *, #17584, .F. ) ;
#27618 = FACE_OUTER_BOUND ( 'NONE', #43675, .T. ) ;
#27619 = PLANE ( 'NONE',  #29960 ) ;
#27620 = ADVANCED_FACE ( 'NONE', ( #31484 ), #35614, .F. ) ;
#27621 = ORIENTED_EDGE ( 'NONE', *, *, #40523, .F. ) ;
#27622 = DIRECTION ( 'NONE',  ( 0.000000000000000000, 0.000000000000000000, 1.000000000000000000 ) ) ;
#27623 = VECTOR ( 'NONE', #38117, 39.37007874015748143 ) ;
#27624 = EDGE_CURVE ( 'NONE', #23841, #18859, #28107, .T. ) ;
#27625 = ORIENTED_EDGE ( 'NONE', *, *, #6836, .F. ) ;
#27626 = ORIENTED_EDGE ( 'NONE', *, *, #3873, .F. ) ;
#27627 = SHAPE_DEFINITION_REPRESENTATION ( #16614, #36385 ) ;
#27629 = EDGE_CURVE ( 'NONE', #4171, #50731, #23711, .T. ) ;
#27628 = ORIENTED_EDGE ( 'NONE', *, *, #5746, .T. ) ;
#27630 = CARTESIAN_POINT ( 'NONE',  ( 0.8182917201112819283, 0.000000000000000000, -0.4724409448818889246 ) ) ;
#27631 = CARTESIAN_POINT ( 'NONE',  ( -0.5455278134075214336, 0.000000000000000000, -1.771653543307081025 ) ) ;
#27632 = CARTESIAN_POINT ( 'NONE',  ( 0.000000000000000000, 0.000000000000000000, 0.000000000000000000 ) ) ;
#27633 = DIRECTION ( 'NONE',  ( -1.000000000000000000, 0.000000000000000000, -0.000000000000000000 ) ) ;
#27634 = ORIENTED_EDGE ( 'NONE', *, *, #5465, .T. ) ;
#27635 = ORIENTED_EDGE ( 'NONE', *, *, #12638, .T. ) ;
#27636 = DIRECTION ( 'NONE',  ( 1.000000000000000000, 0.000000000000000000, -3.469446951953613696E-16 ) ) ;
#27637 = ORIENTED_EDGE ( 'NONE', *, *, #36248, .F. ) ;
#27638 = LINE ( 'NONE', #31530, #35043 ) ;
#27639 = CARTESIAN_POINT ( 'NONE',  ( 0.2727639067037609943, 0.000000000000000000, 2.165354330708650910 ) ) ;
#27640 = EDGE_CURVE ( 'NONE', #11147, #388, #35869, .T. ) ;
#27641 = EDGE_CURVE ( 'NONE', #18496, #21759, #35104, .T. ) ;
#27642 = DIRECTION ( 'NONE',  ( -3.469446951953613696E-16, 0.000000000000000000, -1.000000000000000000 ) ) ;
#27643 = CARTESIAN_POINT ( 'NONE',  ( -0.8942052331142552601, 0.000000000000000000, -0.3149606299212593941 ) ) ;
#27644 = CARTESIAN_POINT ( 'NONE',  ( 0.8339530007628703778, 0.5232038923981141565, 2.082002554611946721 ) ) ;
#27645 = ORIENTED_EDGE ( 'NONE', *, *, #46571, .F. ) ;
#27646 = AXIS2_PLACEMENT_3D ( 'NONE', #13891, #6142, #10266 ) ;
#27647 = EDGE_CURVE ( 'NONE', #12822, #10269, #4627, .T. ) ;
#27648 = CARTESIAN_POINT ( 'NONE',  ( -0.07591351300297333182, 3.346456692913386100, 0.1574803149606283648 ) ) ;
#27649 = SURFACE_SIDE_STYLE ('',( #43138 ) ) ;
#27650 = AXIS2_PLACEMENT_3D ( 'NONE', #23195, #46665, #26817 ) ;
#27651 = VERTEX_POINT ( 'NONE', #8751 ) ;
#27652 = AXIS2_PLACEMENT_3D ( 'NONE', #26660, #18921, #34675 ) ;
#27653 = ORIENTED_EDGE ( 'NONE', *, *, #43668, .F. ) ;
#27654 = CARTESIAN_POINT ( 'NONE',  ( -1.091055626815042645, 3.346456692913386100, -1.574803149606293529 ) ) ;
#27655 = DIRECTION ( 'NONE',  ( 0.000000000000000000, 0.000000000000000000, -1.000000000000000000 ) ) ;
#27656 = DIRECTION ( 'NONE',  ( -0.000000000000000000, 1.000000000000000000, -0.000000000000000000 ) ) ;
#27657 = AXIS2_PLACEMENT_3D ( 'NONE', #7000, #22748, #23493 ) ;
#27658 = ORIENTED_EDGE ( 'NONE', *, *, #46475, .F. ) ;
#27659 = AXIS2_PLACEMENT_3D ( 'NONE', #2045, #20443, #39553 ) ;
#27660 = ORIENTED_EDGE ( 'NONE', *, *, #40943, .F. ) ;
#27661 = CARTESIAN_POINT ( 'NONE',  ( -1.091055626815042645, 3.346456692913386100, -1.141732283464563569 ) ) ;
#27662 = ORIENTED_EDGE ( 'NONE', *, *, #42287, .F. ) ;
#27663 = DIRECTION ( 'NONE',  ( -1.045785279492548401E-16, -1.000000000000000000, 5.036236473261409814E-17 ) ) ;
#27664 = VERTEX_POINT ( 'NONE', #24253 ) ;
#27665 = CARTESIAN_POINT ( 'NONE',  ( -1.636583440222563857, 3.267716535433071279, 2.839019714148966584E-16 ) ) ;
#27666 = LINE ( 'NONE', #4185, #2487 ) ;
#27667 = FACE_OUTER_BOUND ( 'NONE', #12394, .T. ) ;
#27668 = EDGE_CURVE ( 'NONE', #35509, #45901, #19594, .T. ) ;
#27669 = B_SPLINE_CURVE_WITH_KNOTS ( 'NONE', 3,
 ( #20273, #47858, #21305, #658 ),
 .UNSPECIFIED., .F., .F.,
 ( 4, 4 ),
 ( 1.741267681540161096E-05, 0.002517424578720645068 ),
 .UNSPECIFIED. ) ;
#27670 = ORIENTED_EDGE ( 'NONE', *, *, #48125, .F. ) ;
#27671 = ORIENTED_EDGE ( 'NONE', *, *, #27762, .F. ) ;
#27672 = ORIENTED_EDGE ( 'NONE', *, *, #20623, .T. ) ;
#27673 = CARTESIAN_POINT ( 'NONE',  ( 0.03944455730724595599, 0.000000000000000000, -0.07558709797372036021 ) ) ;
#27674 = DIRECTION ( 'NONE',  ( 1.000000000000000000, 0.000000000000000000, -3.469446951953613696E-16 ) ) ;
#27675 = ORIENTED_EDGE ( 'NONE', *, *, #45061, .T. ) ;
#27676 = ORIENTED_EDGE ( 'NONE', *, *, #10267, .T. ) ;
#27677 = CARTESIAN_POINT ( 'NONE',  ( 1.091055626815043311, 0.000000000000000000, 1.574803149606291974 ) ) ;
#27678 = PLANE ( 'NONE',  #49956 ) ;
#27679 = DIRECTION ( 'NONE',  ( -0.9998717552508122886, -0.01601477604151181275, 0.000000000000000000 ) ) ;
#27680 = ORIENTED_EDGE ( 'NONE', *, *, #6282, .T. ) ;
#27681 = ADVANCED_FACE ( 'NONE', ( #24508 ), #35363, .F. ) ;
#27682 = LINE ( 'NONE', #39572, #40319 ) ;
#27683 = CARTESIAN_POINT ( 'NONE',  ( -0.9526633209967887428, 0.000000000000000000, 1.562355641993038669 ) ) ;
#27684 = CARTESIAN_POINT ( 'NONE',  ( 1.363819533518803029, 0.000000000000000000, -1.417322834645665219 ) ) ;
#27685 = EDGE_CURVE ( 'NONE', #43930, #31646, #20370, .T. ) ;
#27686 = VECTOR ( 'NONE', #48068, 39.37007874015748143 ) ;
#27687 = ORIENTED_EDGE ( 'NONE', *, *, #33648, .F. ) ;
#27688 = FACE_OUTER_BOUND ( 'NONE', #3399, .T. ) ;
#27689 = EDGE_CURVE ( 'NONE', #16904, #5663, #27342, .T. ) ;
#27690 = CARTESIAN_POINT ( 'NONE',  ( 2.755905511811024056, 2.913385826771657250, 1.023622047244094446 ) ) ;
#27691 = CIRCLE ( 'NONE', #42512, 1.850107469027523432 ) ;
#27692 = VERTEX_POINT ( 'NONE', #36128 ) ;
#27693 = VECTOR ( 'NONE', #16161, 39.37007874015748143 ) ;
#27694 = CARTESIAN_POINT ( 'NONE',  ( -1.985260859929298016, 3.346456692913386100, -0.6299212598425177889 ) ) ;
#27695 = ORIENTED_EDGE ( 'NONE', *, *, #32273, .F. ) ;
#27696 = VERTEX_POINT ( 'NONE', #32258 ) ;
#27697 = CARTESIAN_POINT ( 'NONE',  ( 0.07982360342473591996, 1.709180471932028711, 0.000000000000000000 ) ) ;
#27698 = VECTOR ( 'NONE', #4257, 39.37007874015748143 ) ;
#27699 = CARTESIAN_POINT ( 'NONE',  ( -0.5756566573089004768, 1.710292258889409833, 2.896516654582634853 ) ) ;
#27700 = VECTOR ( 'NONE', #37158, 39.37007874015748143 ) ;
#27701 = CARTESIAN_POINT ( 'NONE',  ( -0.5455278134075208785, 3.346456692913386100, 1.574803149606291974 ) ) ;
#27702 = CARTESIAN_POINT ( 'NONE',  ( 1.091055626815042423, 0.000000000000000000, -1.574803149606294417 ) ) ;
#27703 = VERTEX_POINT ( 'NONE', #32004 ) ;
#27704 = VERTEX_POINT ( 'NONE', #230 ) ;
#27705 = AXIS2_PLACEMENT_3D ( 'NONE', #29611, #14622, #33751 ) ;
#27706 = EDGE_CURVE ( 'NONE', #29934, #32006, #12118, .T. ) ;
#27707 = ORIENTED_EDGE ( 'NONE', *, *, #41818, .T. ) ;
#27708 = DIRECTION ( 'NONE',  ( 0.000000000000000000, 0.000000000000000000, 1.000000000000000000 ) ) ;
#27709 = CARTESIAN_POINT ( 'NONE',  ( -1.014069264286641570, 0.4235180831842794702, 1.062992125984251635 ) ) ;
#27710 = EDGE_CURVE ( 'NONE', #21459, #25499, #11856, .T. ) ;
#27711 = EDGE_CURVE ( 'NONE', #35391, #4326, #16508, .T. ) ;
#27712 = CARTESIAN_POINT ( 'NONE',  ( -0.5455278134075214336, 0.000000000000000000, -0.5118110236220467790 ) ) ;
#27713 = LINE ( 'NONE', #32637, #21239 ) ;
#27714 = EDGE_LOOP ( 'NONE', ( #20537, #25714, #17396 ) ) ;
#27715 = CARTESIAN_POINT ( 'NONE',  ( -2.152441353505195387, 5.905511811023623991, -0.2419059403265106933 ) ) ;
#27716 = EDGE_CURVE ( 'NONE', #3654, #16745, #47440, .T. ) ;
#27717 = DIRECTION ( 'NONE',  ( -0.9998717552508122886, -0.01601477604151180928, 0.000000000000000000 ) ) ;
#27718 = ORIENTED_EDGE ( 'NONE', *, *, #50317, .F. ) ;
#27719 = DIRECTION ( 'NONE',  ( 0.000000000000000000, 0.000000000000000000, 1.000000000000000000 ) ) ;
#27720 = DIRECTION ( 'NONE',  ( 0.000000000000000000, 0.000000000000000000, 1.000000000000000000 ) ) ;
#27721 = CARTESIAN_POINT ( 'NONE',  ( -1.536664496436148184E-16, 3.267716535433071279, -1.456692913385822630 ) ) ;
#27722 = EDGE_LOOP ( 'NONE', ( #9853, #19714, #23428, #15063 ) ) ;
#27723 = VECTOR ( 'NONE', #22348, 39.37007874015748143 ) ;
#27724 = CARTESIAN_POINT ( 'NONE',  ( -1.503187667631459279, 0.5249316497054297148, 1.135806887463298942 ) ) ;
#27725 = CARTESIAN_POINT ( 'NONE',  ( 1.287906020515830141, 0.000000000000000000, -1.141732283464564013 ) ) ;
#27726 = CARTESIAN_POINT ( 'NONE',  ( 0.000000000000000000, 0.000000000000000000, 0.000000000000000000 ) ) ;
#27727 = CONICAL_SURFACE ( 'NONE', #15361, 3.033577403570480779, 1.554780866114618743 ) ;
#27728 = AXIS2_PLACEMENT_3D ( 'NONE', #607, #3974, #3721 ) ;
#27729 = ORIENTED_EDGE ( 'NONE', *, *, #40449, .T. ) ;
#27730 = LINE ( 'NONE', #371, #27028 ) ;
#27731 = ORIENTED_EDGE ( 'NONE', *, *, #33665, .T. ) ;
#27732 = DIRECTION ( 'NONE',  ( -0.8090169943749422332, 1.288287287306305283E-16, -0.5877852522924802425 ) ) ;
#27733 = VECTOR ( 'NONE', #61, 39.37007874015748143 ) ;
#27734 = CARTESIAN_POINT ( 'NONE',  ( -2.182111253630085290, 0.000000000000000000, 0.9448818897637749625 ) ) ;
#27735 = FACE_OUTER_BOUND ( 'NONE', #6541, .T. ) ;
#27736 = CARTESIAN_POINT ( 'NONE',  ( 1.909347346926324684, 0.000000000000000000, 0.7874015748031456541 ) ) ;
#27737 = AXIS2_PLACEMENT_3D ( 'NONE', #2287, #6670, #11046 ) ;
#27738 = ORIENTED_EDGE ( 'NONE', *, *, #1824, .T. ) ;
#27739 = ORIENTED_EDGE ( 'NONE', *, *, #4953, .F. ) ;
#27740 = CARTESIAN_POINT ( 'NONE',  ( -0.07591351300297305427, 3.267716535433071279, 2.633779063002558971E-17 ) ) ;
#27741 = DIRECTION ( 'NONE',  ( -1.000000000000000000, -0.000000000000000000, -0.000000000000000000 ) ) ;
#27742 = ORIENTED_EDGE ( 'NONE', *, *, #22281, .T. ) ;
#27743 = CARTESIAN_POINT ( 'NONE',  ( 0.000000000000000000, 1.574803149606302854, 0.000000000000000000 ) ) ;
#27744 = CARTESIAN_POINT ( 'NONE',  ( -1.091055626815042645, 3.346456692913386100, 2.204724409448808764 ) ) ;
#27745 = CARTESIAN_POINT ( 'NONE',  ( 0.2718136966839837521, 1.715997676552674323, -2.471090629072964173 ) ) ;
#27746 = CARTESIAN_POINT ( 'NONE',  ( -2.182111253630085734, 3.346456692913386100, -0.9448818897637762948 ) ) ;
#27747 = ORIENTED_EDGE ( 'NONE', *, *, #22724, .F. ) ;
#27748 = VERTEX_POINT ( 'NONE', #23989 ) ;
#27749 = EDGE_CURVE ( 'NONE', #34275, #49325, #5654, .T. ) ;
#27750 = LINE ( 'NONE', #19241, #42737 ) ;
#27751 = LINE ( 'NONE', #392, #47186 ) ;
#27752 = CARTESIAN_POINT ( 'NONE',  ( 1.363819533518803251, 3.346456692913386100, -0.7874015748031473194 ) ) ;
#27753 = DIRECTION ( 'NONE',  ( 1.000000000000000000, 0.000000000000000000, 0.000000000000000000 ) ) ;
#27754 = EDGE_CURVE ( 'NONE', #13831, #11518, #12889, .T. ) ;
#27755 = FACE_BOUND ( 'NONE', #19159, .T. ) ;
#27756 = ORIENTED_EDGE ( 'NONE', *, *, #21384, .F. ) ;
#27757 = EDGE_CURVE ( 'NONE', #30054, #25781, #33283, .T. ) ;
#27758 = LINE ( 'NONE', #23633, #46333 ) ;
#27759 = EDGE_LOOP ( 'NONE', ( #23223, #29690, #39775, #33726 ) ) ;
#27760 = EDGE_LOOP ( 'NONE', ( #5139, #33482, #15957, #45430 ) ) ;
#27761 = DIRECTION ( 'NONE',  ( -3.981026654148627524E-17, 1.000000000000000000, 1.225234019452863932E-16 ) ) ;
#27762 = EDGE_CURVE ( 'NONE', #25457, #31775, #36383, .T. ) ;
#27763 = AXIS2_PLACEMENT_3D ( 'NONE', #16954, #28298, #24440 ) ;
#27764 = ORIENTED_EDGE ( 'NONE', *, *, #48624, .T. ) ;
#27765 = ORIENTED_EDGE ( 'NONE', *, *, #4041, .T. ) ;
#27766 = DIRECTION ( 'NONE',  ( -0.9989930665413144784, 5.247434042673083099E-18, -0.04486483035051863633 ) ) ;
#27767 = ORIENTED_EDGE ( 'NONE', *, *, #40026, .T. ) ;
#27768 = CIRCLE ( 'NONE', #12113, 0.3937007874015748254 ) ;
#27769 = EDGE_CURVE ( 'NONE', #17176, #11883, #24488, .T. ) ;
#27770 = CARTESIAN_POINT ( 'NONE',  ( 0.8182917201112819283, 3.346456692913386100, -0.03937007874015881204 ) ) ;
#27771 = PLANE ( 'NONE',  #24434 ) ;
#27772 = CARTESIAN_POINT ( 'NONE',  ( 0.000000000000000000, 3.267716535433071279, 0.7480314960629874665 ) ) ;
#27773 = EDGE_CURVE ( 'NONE', #13787, #3556, #45373, .T. ) ;
#27774 = VECTOR ( 'NONE', #17371, 39.37007874015748143 ) ;
#27775 = CARTESIAN_POINT ( 'NONE',  ( -1.514466370293032993, 0.000000000000000000, 2.534789744887398388 ) ) ;
#27776 = DIRECTION ( 'NONE',  ( 1.000000000000000000, -0.000000000000000000, 0.000000000000000000 ) ) ;
#27777 = CARTESIAN_POINT ( 'NONE',  ( 0.3820226255272446414, 0.03403845698394380309, 1.829505193364920679 ) ) ;
#27778 = EDGE_LOOP ( 'NONE', ( #25685, #10148, #38682, #44005 ) ) ;
#27779 = CARTESIAN_POINT ( 'NONE',  ( 0.1067246931122726866, 0.02962905676920215767, 0.000000000000000000 ) ) ;
#27780 = ADVANCED_FACE ( 'NONE', ( #10034 ), #5900, .F. ) ;
#27781 = DIRECTION ( 'NONE',  ( 1.734723475976806848E-16, -0.000000000000000000, 1.000000000000000000 ) ) ;
#27782 = DIRECTION ( 'NONE',  ( 1.734723475976806848E-16, -0.000000000000000000, 1.000000000000000000 ) ) ;
#27783 = ORIENTED_EDGE ( 'NONE', *, *, #46050, .T. ) ;
#27784 = DIRECTION ( 'NONE',  ( -1.000000000000000000, 0.000000000000000000, 0.000000000000000000 ) ) ;
#27785 = DIRECTION ( 'NONE',  ( 0.000000000000000000, 0.000000000000000000, 1.000000000000000000 ) ) ;
#27786 = VERTEX_POINT ( 'NONE', #24763 ) ;
#27787 = DIRECTION ( 'NONE',  ( -0.9998717552508122886, -0.01601477604151185785, 0.000000000000000000 ) ) ;
#27788 = CARTESIAN_POINT ( 'NONE',  ( 1.951523201471517588, 0.05917688107560774985, -0.1369052102211298083 ) ) ;
#27789 = DIRECTION ( 'NONE',  ( 0.9989930665413151445, 0.000000000000000000, -0.04486483035050446017 ) ) ;
#27790 = LINE ( 'NONE', #5075, #6785 ) ;
#27791 = ORIENTED_EDGE ( 'NONE', *, *, #37067, .F. ) ;
#27792 = DIRECTION ( 'NONE',  ( 1.734723475976806848E-16, -0.000000000000000000, 1.000000000000000000 ) ) ;
#27793 = CARTESIAN_POINT ( 'NONE',  ( -1.091055626815042201, 3.267716535433071279, 1.574803149606291974 ) ) ;
#27794 = CARTESIAN_POINT ( 'NONE',  ( -2.734482843737247038, 1.205361022782829114E-17, -1.115254632218711794 ) ) ;
#27795 = CARTESIAN_POINT ( 'NONE',  ( 1.363819533518803251, 3.346456692913386100, -0.4724409448818889246 ) ) ;
#27796 = ORIENTED_EDGE ( 'NONE', *, *, #26592, .T. ) ;
#27797 = VECTOR ( 'NONE', #30313, 39.37007874015748143 ) ;
#27798 = VECTOR ( 'NONE', #37340, 39.37007874015748143 ) ;
#27799 = VECTOR ( 'NONE', #48134, 39.37007874015748143 ) ;
#27800 = ORIENTED_EDGE ( 'NONE', *, *, #38239, .T. ) ;
#27801 = EDGE_LOOP ( 'NONE', ( #25527, #50825, #6496, #64 ) ) ;
#27802 = DIRECTION ( 'NONE',  ( 0.000000000000000000, 1.000000000000000000, 0.000000000000000000 ) ) ;
#27803 = VERTEX_POINT ( 'NONE', #48972 ) ;
#27804 = LINE ( 'NONE', #31436, #44392 ) ;
#27805 = LINE ( 'NONE', #39437, #12838 ) ;
#27806 = ORIENTED_EDGE ( 'NONE', *, *, #47854, .F. ) ;
#27807 = DIRECTION ( 'NONE',  ( -0.3930250316539147803, 0.000000000000000000, -0.9195277725514544587 ) ) ;
#27808 = VERTEX_POINT ( 'NONE', #36643 ) ;
#27809 = DIRECTION ( 'NONE',  ( -3.469446951953613696E-16, 0.000000000000000000, -1.000000000000000000 ) ) ;
#27810 = DIRECTION ( 'NONE',  ( 1.734723475976806848E-16, 0.000000000000000000, 1.000000000000000000 ) ) ;
#27811 = EDGE_CURVE ( 'NONE', #11675, #29343, #29427, .T. ) ;
#27812 = VERTEX_POINT ( 'NONE', #17276 ) ;
#27813 = EDGE_CURVE ( 'NONE', #6103, #35018, #42693, .T. ) ;
#27814 = DIRECTION ( 'NONE',  ( 1.000000000000000000, 0.000000000000000000, 0.000000000000000000 ) ) ;
#27815 = ORIENTED_EDGE ( 'NONE', *, *, #12609, .T. ) ;
#27816 = VECTOR ( 'NONE', #10718, 39.37007874015748143 ) ;
#27817 = EDGE_CURVE ( 'NONE', #50859, #5041, #40768, .T. ) ;
#27818 = FACE_OUTER_BOUND ( 'NONE', #15512, .T. ) ;
#27820 = EDGE_LOOP ( 'NONE', ( #40066, #16672, #29519, #49823 ) ) ;
#27819 = EDGE_CURVE ( 'NONE', #22703, #32862, #49228, .T. ) ;
#27821 = ORIENTED_EDGE ( 'NONE', *, *, #8752, .T. ) ;
#27822 = DIRECTION ( 'NONE',  ( 0.000000000000000000, -1.000000000000000000, 0.000000000000000000 ) ) ;
#27823 = PLANE ( 'NONE',  #22922 ) ;
#27824 = VERTEX_POINT ( 'NONE', #44614 ) ;
#27825 = B_SPLINE_CURVE_WITH_KNOTS ( 'NONE', 3,
 ( #29044, #48879, #13565, #7705 ),
 .UNSPECIFIED., .F., .F.,
 ( 4, 4 ),
 ( 0.01334467773481458862, 0.03074214098855171384 ),
 .UNSPECIFIED. ) ;
#27826 = CARTESIAN_POINT ( 'NONE',  ( 0.000000000000000000, 3.267716535433071279, -1.929133858267710666 ) ) ;
#27827 = ORIENTED_EDGE ( 'NONE', *, *, #34088, .F. ) ;
#27828 = CARTESIAN_POINT ( 'NONE',  ( 1.015142113812069313, 0.000000000000000000, 1.102362204724403938 ) ) ;
#27829 = DIRECTION ( 'NONE',  ( 0.000000000000000000, 0.000000000000000000, 1.000000000000000000 ) ) ;
#27830 = EDGE_CURVE ( 'NONE', #33278, #10643, #9267, .T. ) ;
#27831 = CIRCLE ( 'NONE', #3112, 1.181102362204723200 ) ;
#27832 = AXIS2_PLACEMENT_3D ( 'NONE', #11662, #26650, #19397 ) ;
#27833 = CARTESIAN_POINT ( 'NONE',  ( 0.000000000000000000, 3.267716535433071279, -0.1968503937007880511 ) ) ;
#27834 = VERTEX_POINT ( 'NONE', #41525 ) ;
#27835 = VERTEX_POINT ( 'NONE', #21145 ) ;
#27836 = LINE ( 'NONE', #8995, #20328 ) ;
#27837 = DIRECTION ( 'NONE',  ( -3.469446951953613696E-16, 0.000000000000000000, -1.000000000000000000 ) ) ;
#27838 = LINE ( 'NONE', #50520, #35711 ) ;
#27839 = EDGE_CURVE ( 'NONE', #25226, #9823, #46787, .T. ) ;
#27840 = VECTOR ( 'NONE', #13423, 39.37007874015748143 ) ;
#27841 = LINE ( 'NONE', #484, #30137 ) ;
#27842 = FACE_OUTER_BOUND ( 'NONE', #4539, .T. ) ;
#27843 = DIRECTION ( 'NONE',  ( 0.000000000000000000, -1.000000000000000000, 0.000000000000000000 ) ) ;
#27844 = VERTEX_POINT ( 'NONE', #36902 ) ;
#27845 = CARTESIAN_POINT ( 'NONE',  ( -1.712496953225537411, 3.267716535433071279, 5.941417334598190051E-16 ) ) ;
#27846 = VECTOR ( 'NONE', #30700, 39.37007874015748143 ) ;
#27847 = ORIENTED_EDGE ( 'NONE', *, *, #26324, .T. ) ;
#27848 = CARTESIAN_POINT ( 'NONE',  ( 0.000000000000000000, 0.4724409448818898127, 1.014069264286641570 ) ) ;
#27849 = AXIS2_PLACEMENT_3D ( 'NONE', #32509, #20874, #5382 ) ;
#27850 = ORIENTED_EDGE ( 'NONE', *, *, #1471, .T. ) ;
#27851 = EDGE_CURVE ( 'NONE', #21208, #50444, #32522, .T. ) ;
#27852 = CARTESIAN_POINT ( 'NONE',  ( 2.878724150143186833, 0.000000000000000000, -0.6570500018394808128 ) ) ;
#27853 = CARTESIAN_POINT ( 'NONE',  ( -0.8182917201112819283, 0.000000000000000000, -0.9842519685039342603 ) ) ;
#27854 = FACE_OUTER_BOUND ( 'NONE', #9850, .T. ) ;
#27855 = ORIENTED_EDGE ( 'NONE', *, *, #25968, .F. ) ;
#27856 = PLANE ( 'NONE',  #43571 ) ;
#27857 = ORIENTED_EDGE ( 'NONE', *, *, #6585, .F. ) ;
#27858 = LINE ( 'NONE', #46939, #24573 ) ;
#27859 = ORIENTED_EDGE ( 'NONE', *, *, #15999, .F. ) ;
#27860 = DIRECTION ( 'NONE',  ( -3.469446951953613696E-16, 0.000000000000000000, -1.000000000000000000 ) ) ;
#27861 = DIRECTION ( 'NONE',  ( -3.469446951953613696E-16, 0.000000000000000000, -1.000000000000000000 ) ) ;
#27862 = VECTOR ( 'NONE', #32327, 39.37007874015748143 ) ;
#27863 = ORIENTED_EDGE ( 'NONE', *, *, #20802, .T. ) ;
#27864 = B_SPLINE_CURVE_WITH_KNOTS ( 'NONE', 3,
 ( #22417, #49727, #33542, #6159 ),
 .UNSPECIFIED., .F., .F.,
 ( 4, 4 ),
 ( 0.1211873102087489551, 0.1625992483279400380 ),
 .UNSPECIFIED. ) ;
#27865 = DIRECTION ( 'NONE',  ( -3.469446951953613696E-16, 0.000000000000000000, -1.000000000000000000 ) ) ;
#27866 = EDGE_LOOP ( 'NONE', ( #2581, #4127, #18525, #27598 ) ) ;
#27867 = ORIENTED_EDGE ( 'NONE', *, *, #46102, .T. ) ;
#27868 = CARTESIAN_POINT ( 'NONE',  ( 1.300279662861326013, 0.04874602395362847423, 1.413491677621213860 ) ) ;
#27869 = CARTESIAN_POINT ( 'NONE',  ( 1.091055626815043311, 3.346456692913386100, 1.574803149606291974 ) ) ;
#27870 = CARTESIAN_POINT ( 'NONE',  ( 0.000000000000000000, 0.000000000000000000, 0.000000000000000000 ) ) ;
#27871 = CONICAL_SURFACE ( 'NONE', #11413, 2.244934639244524632, 1.554780866114618743 ) ;
#27872 = EDGE_CURVE ( 'NONE', #24676, #29929, #44871, .T. ) ;
#27874 = ORIENTED_EDGE ( 'NONE', *, *, #28828, .F. ) ;
#27873 = VECTOR ( 'NONE', #17168, 39.37007874015748143 ) ;
#27875 = FACE_OUTER_BOUND ( 'NONE', #19273, .T. ) ;
#27876 = LINE ( 'NONE', #43621, #6885 ) ;
#27877 = EDGE_CURVE ( 'NONE', #33984, #18859, #23858, .T. ) ;
#27878 = EDGE_CURVE ( 'NONE', #15242, #27924, #9523, .T. ) ;
#27879 = ORIENTED_EDGE ( 'NONE', *, *, #14103, .T. ) ;
#27880 = VECTOR ( 'NONE', #17249, 39.37007874015748143 ) ;
#27881 = CARTESIAN_POINT ( 'NONE',  ( 2.052631463899902364, 3.346456692913386100, 0.4724409448818868706 ) ) ;
#27882 = EDGE_LOOP ( 'NONE', ( #13475, #37513, #48929, #809, #43994, #31687, #17310, #17758, #28193, #7915, #30744, #40273, #6107, #41817, #1712, #37894, #13207, #23814, #751, #406, #17242, #8603, #11469, #44824, #9092, #19267, #12013, #3313, #17735, #49896, #37750, #47244, #27047, #14043, #26593, #171, #19075, #2892, #32668, #15703, #28907, #13856, #46183, #2314, #5361, #38660, #24461, #22549, #15894, #6866, #45827, #19097, #47424, #1090, #23310, #28086, #1894, #33274, #25244, #32824, #34722, #15439, #16515, #41182, #21556, #19961, #11763, #47066, #43969, #25361, #31377, #45180, #46505, #10966, #1070, #45561, #38879, #27718, #3451, #13658, #22874, #49154, #50315, #20516 ) ) ;
#27883 = ORIENTED_EDGE ( 'NONE', *, *, #28489, .T. ) ;
#27884 = PRODUCT_CONTEXT ( 'NONE', #17724, 'mechanical' ) ;
#27885 = VECTOR ( 'NONE', #687, 39.37007874015748143 ) ;
#27886 = ORIENTED_EDGE ( 'NONE', *, *, #14496, .T. ) ;
#27887 = DIRECTION ( 'NONE',  ( -1.000000000000000000, 0.000000000000000000, 0.000000000000000000 ) ) ;
#27888 = CARTESIAN_POINT ( 'NONE',  ( 0.08139965876239094178, 1.610780518492231694, 0.000000000000000000 ) ) ;
#27889 = ADVANCED_FACE ( 'NONE', ( #10540 ), #6916, .F. ) ;
#27890 = CARTESIAN_POINT ( 'NONE',  ( 0.2178414669595446496, 0.5249316497054297148, -1.871410041920607004 ) ) ;
#27891 = LINE ( 'NONE', #12407, #10686 ) ;
#27892 = ORIENTED_EDGE ( 'NONE', *, *, #8204, .F. ) ;
#27893 = ORIENTED_EDGE ( 'NONE', *, *, #28389, .F. ) ;
#27894 = DIRECTION ( 'NONE',  ( -3.469446951953613696E-16, 0.000000000000000000, -1.000000000000000000 ) ) ;
#27895 = CARTESIAN_POINT ( 'NONE',  ( -0.7381027496704858359, 0.000000000000000000, -2.859439394060923512 ) ) ;
#27896 = EDGE_CURVE ( 'NONE', #4293, #17674, #49258, .T. ) ;
#27897 = ORIENTED_EDGE ( 'NONE', *, *, #6385, .T. ) ;
#27898 = DIRECTION ( 'NONE',  ( 1.000000000000000000, 0.000000000000000000, -3.469446951953613696E-16 ) ) ;
#27899 = CARTESIAN_POINT ( 'NONE',  ( 0.000000000000000000, 3.267716535433071279, 1.062992125984246083 ) ) ;
#27900 = CARTESIAN_POINT ( 'NONE',  ( -0.8182917201112815953, 3.267716535433071279, 1.419509857074482553E-16 ) ) ;
#27901 = CONICAL_SURFACE ( 'NONE', #10604, 1.850107469027523210, 0.6386652850508578450 ) ;
#27902 = ADVANCED_FACE ( 'NONE', ( #45877 ), #26287, .F. ) ;
#27903 = LINE ( 'NONE', #16037, #6081 ) ;
#27904 = CARTESIAN_POINT ( 'NONE',  ( 0.3543214468173200293, 1.713577057256821190, 2.228085083314873316 ) ) ;
#27905 = ORIENTED_EDGE ( 'NONE', *, *, #39185, .T. ) ;
#27906 = CARTESIAN_POINT ( 'NONE',  ( 1.770012363201889594, 3.346456692913386100, -1.141732283464564013 ) ) ;
#27907 = CARTESIAN_POINT ( 'NONE',  ( 1.574803149606299746, 1.172985819482486702, -1.033098100527919830E-16 ) ) ;
#27908 = VERTEX_POINT ( 'NONE', #38420 ) ;
#27909 = EDGE_CURVE ( 'NONE', #196, #23904, #32545, .T. ) ;
#27910 = ORIENTED_EDGE ( 'NONE', *, *, #45242, .F. ) ;
#27911 = AXIS2_PLACEMENT_3D ( 'NONE', #42426, #66, #47275 ) ;
#27913 = DIRECTION ( 'NONE',  ( 1.000000000000000000, 0.000000000000000000, -3.469446951953613696E-16 ) ) ;
#27912 = VECTOR ( 'NONE', #14041, 39.37007874015748143 ) ;
#27914 = CARTESIAN_POINT ( 'NONE',  ( 2.559055118110236560, 0.000000000000000000, -4.133858267716535195 ) ) ;
#27915 = CARTESIAN_POINT ( 'NONE',  ( -1.909347346926324462, 0.000000000000000000, 0.4724409448818871482 ) ) ;
#27916 = ORIENTED_EDGE ( 'NONE', *, *, #23648, .F. ) ;
#27917 = VECTOR ( 'NONE', #43888, 39.37007874015748143 ) ;
#27918 = EDGE_CURVE ( 'NONE', #29175, #14008, #42032, .T. ) ;
#27919 = ORIENTED_EDGE ( 'NONE', *, *, #40487, .T. ) ;
#27920 = DIRECTION ( 'NONE',  ( 1.734723475976806848E-16, -0.000000000000000000, 1.000000000000000000 ) ) ;
#27921 = ORIENTED_EDGE ( 'NONE', *, *, #40616, .T. ) ;
#27922 = AXIS2_PLACEMENT_3D ( 'NONE', #2660, #18409, #2154 ) ;
#27923 = LINE ( 'NONE', #18919, #2350 ) ;
#27924 = VERTEX_POINT ( 'NONE', #2285 ) ;
#27925 = ADVANCED_FACE ( 'NONE', ( #14920 ), #34796, .F. ) ;
#27926 = CARTESIAN_POINT ( 'NONE',  ( 0.7521025634872258170, 1.621523052975431867, 2.144027383376515328 ) ) ;
#27927 = DIRECTION ( 'NONE',  ( 0.000000000000000000, -1.000000000000000000, 0.000000000000000000 ) ) ;
#27928 = CARTESIAN_POINT ( 'NONE',  ( 0.8182917201112819283, 3.267716535433071279, -1.299212598425193210 ) ) ;
#27929 = ORIENTED_EDGE ( 'NONE', *, *, #50604, .F. ) ;
#27930 = ORIENTED_EDGE ( 'NONE', *, *, #20237, .T. ) ;
#27931 = ORIENTED_EDGE ( 'NONE', *, *, #27769, .T. ) ;
#27932 = DIRECTION ( 'NONE',  ( -1.206139481778036182E-16, 1.000000000000000000, -4.526717189434842013E-17 ) ) ;
#27933 = LINE ( 'NONE', #50862, #42797 ) ;
#27934 = EDGE_LOOP ( 'NONE', ( #14538, #32907, #7199, #26821 ) ) ;
#27935 = VERTEX_POINT ( 'NONE', #30668 ) ;
#27936 = LINE ( 'NONE', #48034, #14886 ) ;
#27937 = CARTESIAN_POINT ( 'NONE',  ( -0.5455278134075208785, 0.000000000000000000, 1.889763779527550369 ) ) ;
#27938 = DIRECTION ( 'NONE',  ( 1.000000000000000000, 0.000000000000000000, 0.000000000000000000 ) ) ;
#27939 = ADVANCED_FACE ( 'NONE', ( #14413 ), #31166, .F. ) ;
#27940 = ORIENTED_EDGE ( 'NONE', *, *, #45530, .T. ) ;
#27941 = ORIENTED_EDGE ( 'NONE', *, *, #48899, .T. ) ;
#27942 = DIRECTION ( 'NONE',  ( -1.000000000000000000, 0.000000000000000000, -0.000000000000000000 ) ) ;
#27943 = CARTESIAN_POINT ( 'NONE',  ( -0.8987785766980536106, 1.205361022782829114E-17, 1.600251783270283390 ) ) ;
#27944 = AXIS2_PLACEMENT_3D ( 'NONE', #14229, #26606, #10617 ) ;
#27945 = LINE ( 'NONE', #23823, #4739 ) ;
#27946 = ADVANCED_FACE ( 'NONE', ( #37667 ), #10285, .T. ) ;
#27947 = EDGE_CURVE ( 'NONE', #45649, #34423, #15496, .T. ) ;
#27948 = ORIENTED_EDGE ( 'NONE', *, *, #21837, .T. ) ;
#27949 = DIRECTION ( 'NONE',  ( -0.000000000000000000, -1.000000000000000000, -0.000000000000000000 ) ) ;
#27950 = CARTESIAN_POINT ( 'NONE',  ( 1.833433833923351353, 0.000000000000000000, -1.161035397307311917E-15 ) ) ;
#27951 = VERTEX_POINT ( 'NONE', #21911 ) ;
#27952 = CARTESIAN_POINT ( 'NONE',  ( -0.2727639067037602727, 3.267716535433071279, 1.220472440944875281 ) ) ;
#27953 = ORIENTED_EDGE ( 'NONE', *, *, #38939, .T. ) ;
#27954 = ORIENTED_EDGE ( 'NONE', *, *, #20009, .T. ) ;
#27955 = FACE_OUTER_BOUND ( 'NONE', #28696, .T. ) ;
#27956 = LINE ( 'NONE', #39585, #38298 ) ;
#27957 = VECTOR ( 'NONE', #37037, 39.37007874015748143 ) ;
#27958 = CARTESIAN_POINT ( 'NONE',  ( 0.000000000000000000, 6.692913385826772199, 0.000000000000000000 ) ) ;
#27959 = CARTESIAN_POINT ( 'NONE',  ( 0.3545323396393251780, 1.647963639598186036, 2.229247198548944375 ) ) ;
#27961 = VECTOR ( 'NONE', #48592, 39.37007874015748143 ) ;
#27960 = CARTESIAN_POINT ( 'NONE',  ( 1.636583440222563857, 3.267716535433071279, 1.417869535855831975 ) ) ;
#27962 = ORIENTED_EDGE ( 'NONE', *, *, #184, .F. ) ;
#27963 = ORIENTED_EDGE ( 'NONE', *, *, #6068, .F. ) ;
#27964 = CONICAL_SURFACE ( 'NONE', #36197, 2.089297179032357121, 0.2617993877991570129 ) ;
#27965 = VERTEX_POINT ( 'NONE', #34044 ) ;
#27966 = CARTESIAN_POINT ( 'NONE',  ( -0.5756566573089003658, 0.000000000000000000, 2.896516654582634853 ) ) ;
#27967 = DIRECTION ( 'NONE',  ( -0.000000000000000000, 1.000000000000000000, -0.000000000000000000 ) ) ;
#27968 = EDGE_CURVE ( 'NONE', #39361, #45523, #46133, .T. ) ;
#27969 = DIRECTION ( 'NONE',  ( 1.000000000000000000, -0.000000000000000000, 0.000000000000000000 ) ) ;
#27970 = CARTESIAN_POINT ( 'NONE',  ( -0.8949303405208608453, 1.574803149606302854, -1.971765468592543202 ) ) ;
#27971 = ORIENTED_EDGE ( 'NONE', *, *, #4905, .F. ) ;
#27972 = DIRECTION ( 'NONE',  ( -1.000000000000000000, 0.000000000000000000, 0.000000000000000000 ) ) ;
#27973 = CARTESIAN_POINT ( 'NONE',  ( 2.555365368299595323E-16, 1.585169487999011917, 2.086614173228346303 ) ) ;
#27974 = EDGE_CURVE ( 'NONE', #34792, #47654, #3292, .T. ) ;
#27975 = VERTEX_POINT ( 'NONE', #41780 ) ;
#27976 = LINE ( 'NONE', #47817, #14156 ) ;
#27977 = EDGE_CURVE ( 'NONE', #904, #41852, #18544, .T. ) ;
#27978 = DIRECTION ( 'NONE',  ( -0.01601477604151182663, 0.9998717552508123996, -0.000000000000000000 ) ) ;
#27979 = CARTESIAN_POINT ( 'NONE',  ( -0.4842960162298967641, 0.000000000000000000, -1.816169684210588331 ) ) ;
#27981 = EDGE_CURVE ( 'NONE', #49063, #46927, #49984, .T. ) ;
#27980 = ORIENTED_EDGE ( 'NONE', *, *, #27762, .T. ) ;
#27982 = CARTESIAN_POINT ( 'NONE',  ( 0.000000000000000000, 2.755905511811022723, 0.000000000000000000 ) ) ;
#27983 = DIRECTION ( 'NONE',  ( 2.842176228468331432E-14, 0.000000000000000000, 1.000000000000000000 ) ) ;
#27984 = CARTESIAN_POINT ( 'NONE',  ( -1.363819533518803029, 3.346456692913386100, 0.9055118110236167750 ) ) ;
#27985 = ORIENTED_EDGE ( 'NONE', *, *, #6503, .F. ) ;
#27986 = DIRECTION ( 'NONE',  ( -0.000000000000000000, 1.000000000000000000, -0.000000000000000000 ) ) ;
#27987 = CARTESIAN_POINT ( 'NONE',  ( 0.000000000000000000, 6.692913385826772199, 0.000000000000000000 ) ) ;
#27988 = VERTEX_POINT ( 'NONE', #6418 ) ;
#27989 = FACE_OUTER_BOUND ( 'NONE', #46595, .T. ) ;
#27990 = VECTOR ( 'NONE', #3141, 39.37007874015748143 ) ;
#27991 = CARTESIAN_POINT ( 'NONE',  ( 0.8515791614234311524, 0.000000000000000000, 1.521253268579216167 ) ) ;
#27992 = CARTESIAN_POINT ( 'NONE',  ( 2.378961647330872786, 3.346456692913386100, -1.161035397307311917E-15 ) ) ;
#27993 = DIRECTION ( 'NONE',  ( -0.9998717552508122886, -0.01601477604151182316, 0.000000000000000000 ) ) ;
#27994 = EDGE_CURVE ( 'NONE', #21949, #3678, #49728, .T. ) ;
#27995 = ORIENTED_EDGE ( 'NONE', *, *, #20568, .F. ) ;
#27996 = ORIENTED_EDGE ( 'NONE', *, *, #39939, .T. ) ;
#27997 = DIRECTION ( 'NONE',  ( 1.000000000000000000, -0.000000000000000000, 0.000000000000000000 ) ) ;
#27998 = CARTESIAN_POINT ( 'NONE',  ( 1.856205413694107520, 1.642665920110450317, -1.706627555837983090 ) ) ;
#27999 = EDGE_LOOP ( 'NONE', ( #43856, #27500, #44074, #7870 ) ) ;
#28000 = CARTESIAN_POINT ( 'NONE',  ( -1.985260859929297794, 3.267716535433071279, -0.5118110236220464460 ) ) ;
#28001 = DIRECTION ( 'NONE',  ( -3.981026654148627524E-17, 1.000000000000000000, 1.225234019452863932E-16 ) ) ;
#28002 = AXIS2_PLACEMENT_3D ( 'NONE', #12689, #32065, #16306 ) ;
#28003 = CARTESIAN_POINT ( 'NONE',  ( 1.472219874544873131, 1.643743200001983151, 2.560030851058970214 ) ) ;
#28004 = EDGE_CURVE ( 'NONE', #14797, #2445, #1495, .T. ) ;
#28005 = CARTESIAN_POINT ( 'NONE',  ( 1.833433833923351353, 0.000000000000000000, -0.1968503937007886062 ) ) ;
#28006 = EDGE_LOOP ( 'NONE', ( #34977, #8397, #17739, #11556 ) ) ;
#28007 = ORIENTED_EDGE ( 'NONE', *, *, #16035, .F. ) ;
#28008 = DIRECTION ( 'NONE',  ( -3.986037398843765983E-20, -1.000000000000000000, -1.160734090543304660E-16 ) ) ;
#28009 = CARTESIAN_POINT ( 'NONE',  ( -1.862188077367287642, 3.346456692913386100, -0.9842519685039344823 ) ) ;
#28010 = CARTESIAN_POINT ( 'NONE',  ( -0.8182917201112814842, 0.000000000000000000, 0.7874015748031456541 ) ) ;
#28011 = EDGE_CURVE ( 'NONE', #3260, #11491, #33797, .T. ) ;
#28012 = EDGE_CURVE ( 'NONE', #24400, #3300, #523, .T. ) ;
#28013 = CARTESIAN_POINT ( 'NONE',  ( -2.793030215715272213, 1.675725205278408403, 0.9592557174602281966 ) ) ;
#28014 = FACE_BOUND ( 'NONE', #32207, .T. ) ;
#28015 = VERTEX_POINT ( 'NONE', #32912 ) ;
#28016 = EDGE_CURVE ( 'NONE', #26276, #8950, #44497, .T. ) ;
#28017 = ADVANCED_FACE ( 'NONE', ( #24380 ), #12500, .F. ) ;
#28018 = CARTESIAN_POINT ( 'NONE',  ( 0.9914495361338625523, 1.734714548371065312, 2.781765111341823360 ) ) ;
#28019 = ORIENTED_EDGE ( 'NONE', *, *, #197, .F. ) ;
#28020 = EDGE_LOOP ( 'NONE', ( #1857, #38138, #33619, #46576 ) ) ;
#28021 = DIRECTION ( 'NONE',  ( 0.000000000000000000, 0.000000000000000000, -1.000000000000000000 ) ) ;
#28022 = VECTOR ( 'NONE', #50133, 39.37007874015748143 ) ;
#28023 = VERTEX_POINT ( 'NONE', #47830 ) ;
#28024 = EDGE_LOOP ( 'NONE', ( #4375, #22533, #23714, #51016, #36208, #40035 ) ) ;
#28025 = CARTESIAN_POINT ( 'NONE',  ( -0.6214413264104945434, 3.346456692913386100, -1.732283464566922726 ) ) ;
#28026 = ORIENTED_EDGE ( 'NONE', *, *, #49067, .T. ) ;
#28027 = CARTESIAN_POINT ( 'NONE',  ( 0.000000000000000000, 0.000000000000000000, 0.000000000000000000 ) ) ;
#28028 = DIRECTION ( 'NONE',  ( 1.000000000000000000, -0.000000000000000000, 0.000000000000000000 ) ) ;
#28029 = CARTESIAN_POINT ( 'NONE',  ( 0.000000000000000000, 3.267716535433071279, 0.2755905511810996522 ) ) ;
#28030 = VECTOR ( 'NONE', #23967, 39.37007874015748143 ) ;
#28031 = VECTOR ( 'NONE', #39838, 39.37007874015748143 ) ;
#28032 = DIRECTION ( 'NONE',  ( -0.000000000000000000, 1.000000000000000000, -0.000000000000000000 ) ) ;
#28033 = CARTESIAN_POINT ( 'NONE',  ( -0.2134117707794043750, 0.02450148541315291459, -1.822192086320855164 ) ) ;
#28034 = CARTESIAN_POINT ( 'NONE',  ( -0.2727639067037607723, 3.267716535433071279, 2.362204724409437961 ) ) ;
#28035 = ORIENTED_EDGE ( 'NONE', *, *, #47626, .T. ) ;
#28036 = DIRECTION ( 'NONE',  ( -1.000000000000000000, 0.000000000000000000, 1.734723475976806848E-16 ) ) ;
#28037 = VECTOR ( 'NONE', #22799, 39.37007874015748143 ) ;
#28038 = CARTESIAN_POINT ( 'NONE',  ( 0.000000000000000000, 2.755905511811023612, -0.8858267716535433989 ) ) ;
#28039 = CARTESIAN_POINT ( 'NONE',  ( 1.083598637574781920, 5.905511811023623991, 2.747180975113346246 ) ) ;
#28040 = ORIENTED_EDGE ( 'NONE', *, *, #1670, .T. ) ;
#28041 = DIRECTION ( 'NONE',  ( -3.469446951953613696E-16, 0.000000000000000000, -1.000000000000000000 ) ) ;
#28042 = EDGE_CURVE ( 'NONE', #30813, #16270, #1133, .T. ) ;
#28043 = CARTESIAN_POINT ( 'NONE',  ( 0.5455278134075217666, 0.000000000000000000, 2.204724409448808764 ) ) ;
#28044 = ORIENTED_EDGE ( 'NONE', *, *, #12221, .F. ) ;
#28045 = DIRECTION ( 'NONE',  ( -0.9510565162951500895, 0.000000000000000000, -0.3090169943749582204 ) ) ;
#28046 = DIRECTION ( 'NONE',  ( -3.469446951953613696E-16, 0.000000000000000000, -1.000000000000000000 ) ) ;
#28047 = EDGE_CURVE ( 'NONE', #41410, #38137, #1394, .T. ) ;
#28048 = DIRECTION ( 'NONE',  ( 0.000000000000000000, -1.000000000000000000, 0.000000000000000000 ) ) ;
#28049 = CARTESIAN_POINT ( 'NONE',  ( -2.182111253630085290, 0.000000000000000000, 0.3149606299212578953 ) ) ;
#28050 = ORIENTED_EDGE ( 'NONE', *, *, #26336, .F. ) ;
#28051 = DIRECTION ( 'NONE',  ( 1.734723475976806848E-16, -0.000000000000000000, 1.000000000000000000 ) ) ;
#28052 = DIRECTION ( 'NONE',  ( -0.000000000000000000, 1.000000000000000000, -0.000000000000000000 ) ) ;
#28053 = CARTESIAN_POINT ( 'NONE',  ( -1.909347346926324462, 3.346456692913386100, 0.1574803149606286423 ) ) ;
#28054 = DIRECTION ( 'NONE',  ( 8.902872254220023478E-17, 1.000000000000000000, -9.311674343991161395E-17 ) ) ;
#28055 = ORIENTED_EDGE ( 'NONE', *, *, #29307, .T. ) ;
#28056 = ORIENTED_EDGE ( 'NONE', *, *, #15996, .F. ) ;
#28057 = LINE ( 'NONE', #15931, #42726 ) ;
#28058 = ORIENTED_EDGE ( 'NONE', *, *, #37602, .T. ) ;
#28059 = ADVANCED_FACE ( 'NONE', ( #48341 ), #38584, .T. ) ;
#28060 = DIRECTION ( 'NONE',  ( -3.981026654148627524E-17, 1.000000000000000000, 1.225234019452863932E-16 ) ) ;
#28061 = ORIENTED_EDGE ( 'NONE', *, *, #1473, .F. ) ;
#28062 = CIRCLE ( 'NONE', #15720, 2.165354330708661568 ) ;
#28063 = DIRECTION ( 'NONE',  ( 0.000000000000000000, 0.000000000000000000, 1.000000000000000000 ) ) ;
#28064 = EDGE_CURVE ( 'NONE', #22637, #39017, #3113, .T. ) ;
#28065 = ORIENTED_EDGE ( 'NONE', *, *, #42060, .F. ) ;
#28066 = CARTESIAN_POINT ( 'NONE',  ( -1.909347346926324462, 0.000000000000000000, 0.1574803149606286423 ) ) ;
#28067 = EDGE_CURVE ( 'NONE', #27692, #29609, #20832, .T. ) ;
#28068 = DIRECTION ( 'NONE',  ( 0.000000000000000000, 1.000000000000000000, 0.000000000000000000 ) ) ;
#28069 = ORIENTED_EDGE ( 'NONE', *, *, #46673, .T. ) ;
#28070 = EDGE_CURVE ( 'NONE', #12066, #24845, #5014, .T. ) ;
#28071 = CARTESIAN_POINT ( 'NONE',  ( 1.015142113812069979, 0.000000000000000000, 1.535433070866133898 ) ) ;
#28072 = EDGE_LOOP ( 'NONE', ( #11845, #7141, #19887, #47734 ) ) ;
#28073 = VECTOR ( 'NONE', #189, 39.37007874015748143 ) ;
#28074 = ADVANCED_FACE ( 'NONE', ( #20507 ), #21019, .F. ) ;
#28075 = CARTESIAN_POINT ( 'NONE',  ( 1.833433833923350909, 0.000000000000000000, -1.456692913385823296 ) ) ;
#28076 = ORIENTED_EDGE ( 'NONE', *, *, #8915, .T. ) ;
#28077 = EDGE_LOOP ( 'NONE', ( #41803, #49575, #39303, #10753 ) ) ;
#28078 = DIRECTION ( 'NONE',  ( 0.04486483035050446017, -1.160734090543304660E-16, 0.9989930665413151445 ) ) ;
#28079 = DIRECTION ( 'NONE',  ( -0.000000000000000000, 1.000000000000000000, -0.000000000000000000 ) ) ;
#28080 = ORIENTED_EDGE ( 'NONE', *, *, #34645, .F. ) ;
#28081 = CARTESIAN_POINT ( 'NONE',  ( -0.3498457532482182053, 1.702298530840201662, 2.203421978946157989 ) ) ;
#28082 = VERTEX_POINT ( 'NONE', #885 ) ;
#28083 = CARTESIAN_POINT ( 'NONE',  ( -3.927031490892378253E-16, 3.267716535433071279, -2.204724409448811429 ) ) ;
#28084 = CYLINDRICAL_SURFACE ( 'NONE', #21750, 2.164630168518208109 ) ;
#28085 = PLANE ( 'NONE',  #46147 ) ;
#28086 = ORIENTED_EDGE ( 'NONE', *, *, #26222, .T. ) ;
#28087 = ORIENTED_EDGE ( 'NONE', *, *, #2326, .T. ) ;
#28088 = CARTESIAN_POINT ( 'NONE',  ( -1.363819533518803029, 3.346456692913386100, 0.4724409448818871482 ) ) ;
#28089 = CARTESIAN_POINT ( 'NONE',  ( 1.129748414438405124, 1.627571742414081202, 1.986830176535870907 ) ) ;
#28090 = LINE ( 'NONE', #36368, #34901 ) ;
#28091 = CARTESIAN_POINT ( 'NONE',  ( 1.064963178929838161, 0.01474687883001544499, 1.686498296765969407 ) ) ;
#28092 = LINE ( 'NONE', #28610, #39646 ) ;
#28093 = VECTOR ( 'NONE', #14748, 39.37007874015748143 ) ;
#28094 = CARTESIAN_POINT ( 'NONE',  ( -0.9360721529196992519, 0.000000000000000000, 1.470771056236103158 ) ) ;
#28095 = VERTEX_POINT ( 'NONE', #16643 ) ;
#28096 = DIRECTION ( 'NONE',  ( 0.000000000000000000, 0.000000000000000000, -1.000000000000000000 ) ) ;
#28097 = EDGE_CURVE ( 'NONE', #30125, #24532, #18360, .T. ) ;
#28098 = DIMENSIONAL_EXPONENTS ( 1.000000000000000000, 0.000000000000000000, 0.000000000000000000, 0.000000000000000000, 0.000000000000000000, 0.000000000000000000, 0.000000000000000000 ) ;
#28099 = VERTEX_POINT ( 'NONE', #8885 ) ;
#28100 = CARTESIAN_POINT ( 'NONE',  ( 0.000000000000000000, 3.267716535433071279, -1.299212598425194320 ) ) ;
#28101 = EDGE_CURVE ( 'NONE', #2103, #43399, #24122, .T. ) ;
#28102 = VECTOR ( 'NONE', #31381, 39.37007874015748143 ) ;
#28103 = ORIENTED_EDGE ( 'NONE', *, *, #32930, .T. ) ;
#28104 = EDGE_CURVE ( 'NONE', #13984, #4136, #24640, .T. ) ;
#28105 = CARTESIAN_POINT ( 'NONE',  ( 0.5286458662987441048, 1.205361022782829114E-17, 2.100489422084715230 ) ) ;
#28106 = AXIS2_PLACEMENT_3D ( 'NONE', #17961, #49160, #48390 ) ;
#28107 = LINE ( 'NONE', #19847, #46748 ) ;
#28108 = DIRECTION ( 'NONE',  ( 1.000000000000000000, -0.000000000000000000, -0.000000000000000000 ) ) ;
#28109 = VERTEX_POINT ( 'NONE', #36770 ) ;
#28110 = CARTESIAN_POINT ( 'NONE',  ( -1.636583440222564301, 3.346456692913386100, -1.574803149606293307 ) ) ;
#28111 = DIRECTION ( 'NONE',  ( 1.734723475976806848E-16, -0.000000000000000000, 1.000000000000000000 ) ) ;
#28112 = VERTEX_POINT ( 'NONE', #47574 ) ;
#28113 = FACE_OUTER_BOUND ( 'NONE', #2019, .T. ) ;
#28114 = ORIENTED_EDGE ( 'NONE', *, *, #40882, .T. ) ;
#28115 = DIRECTION ( 'NONE',  ( -1.000000000000000000, -0.000000000000000000, -0.000000000000000000 ) ) ;
#28116 = CARTESIAN_POINT ( 'NONE',  ( -1.636583440222563635, 3.346456692913386100, 0.4330708661417290162 ) ) ;
#28117 = ADVANCED_FACE ( 'NONE', ( #13277 ), #8121, .T. ) ;
#28118 = DIRECTION ( 'NONE',  ( -0.01601477604151182663, 0.9998717552508123996, -0.000000000000000000 ) ) ;
#28119 = VERTEX_POINT ( 'NONE', #4244 ) ;
#28120 = ORIENTED_EDGE ( 'NONE', *, *, #43600, .T. ) ;
#28121 = EDGE_CURVE ( 'NONE', #344, #37003, #46047, .T. ) ;
#28122 = PRODUCT ( 'Front Cover', 'Front Cover', '', ( #47726 ) ) ;
#28123 = LINE ( 'NONE', #250, #25175 ) ;
#28124 = DIRECTION ( 'NONE',  ( 1.000000000000000000, 0.000000000000000000, 0.000000000000000000 ) ) ;
#28125 = FACE_BOUND ( 'NONE', #22457, .T. ) ;
#28126 = VECTOR ( 'NONE', #35332, 39.37007874015748854 ) ;
#28127 = VECTOR ( 'NONE', #18725, 39.37007874015748143 ) ;
#28128 = AXIS2_PLACEMENT_3D ( 'NONE', #50942, #23892, #39638 ) ;
#28129 = PLANE ( 'NONE',  #4790 ) ;
#28130 = DIRECTION ( 'NONE',  ( -3.469446951953613696E-16, 0.000000000000000000, -1.000000000000000000 ) ) ;
#28131 = EDGE_LOOP ( 'NONE', ( #40094, #27742, #35513, #42711 ) ) ;
#28132 = CARTESIAN_POINT ( 'NONE',  ( -2.182111253630085290, 0.000000000000000000, -0.5118110236220464460 ) ) ;
#28133 = VECTOR ( 'NONE', #37806, 39.37007874015748143 ) ;
#28134 = ORIENTED_EDGE ( 'NONE', *, *, #7190, .T. ) ;
#28135 = ORIENTED_EDGE ( 'NONE', *, *, #3540, .T. ) ;
#28136 = VECTOR ( 'NONE', #21170, 39.37007874015748143 ) ;
#28137 = APPLICATION_PROTOCOL_DEFINITION ( 'draft international standard', 'automotive_design', 1998, #17724 ) ;
#28138 = EDGE_CURVE ( 'NONE', #903, #20943, #20240, .T. ) ;
#28139 = VERTEX_POINT ( 'NONE', #5525 ) ;
#28140 = LINE ( 'NONE', #32553, #7008 ) ;
#28141 = AXIS2_PLACEMENT_3D ( 'NONE', #49910, #41711, #3480 ) ;
#28142 = DIRECTION ( 'NONE',  ( 1.000000000000000000, -0.000000000000000000, 0.000000000000000000 ) ) ;
#28143 = DIRECTION ( 'NONE',  ( -0.000000000000000000, 0.000000000000000000, 1.000000000000000000 ) ) ;
#28144 = LINE ( 'NONE', #39520, #24695 ) ;
#28145 = VERTEX_POINT ( 'NONE', #9397 ) ;
#28146 = ORIENTED_EDGE ( 'NONE', *, *, #49335, .F. ) ;
#28147 = CARTESIAN_POINT ( 'NONE',  ( 0.1155636338427008941, -0.5222242541845523167, 0.000000000000000000 ) ) ;
#28148 = PLANE ( 'NONE',  #37871 ) ;
#28149 = DIRECTION ( 'NONE',  ( -0.000000000000000000, 1.000000000000000000, -0.000000000000000000 ) ) ;
#28150 = ORIENTED_EDGE ( 'NONE', *, *, #30294, .T. ) ;
#28151 = CARTESIAN_POINT ( 'NONE',  ( -0.5455278134075214336, 3.346456692913386100, -1.456692913385822630 ) ) ;
#28152 = DIRECTION ( 'NONE',  ( -0.000000000000000000, 1.000000000000000000, -0.000000000000000000 ) ) ;
#28153 = DIRECTION ( 'NONE',  ( -0.000000000000000000, 1.000000000000000000, -0.000000000000000000 ) ) ;
#28154 = DIRECTION ( 'NONE',  ( -0.000000000000000000, -1.000000000000000000, -0.000000000000000000 ) ) ;
#28155 = PLANE ( 'NONE',  #38438 ) ;
#28156 = ORIENTED_EDGE ( 'NONE', *, *, #36175, .T. ) ;
#28157 = DIRECTION ( 'NONE',  ( -1.000000000000000000, 0.000000000000000000, 1.734723475976806848E-16 ) ) ;
#28158 = EDGE_CURVE ( 'NONE', #28712, #14290, #2420, .T. ) ;
#28159 = ORIENTED_EDGE ( 'NONE', *, *, #42498, .F. ) ;
#28160 = EDGE_CURVE ( 'NONE', #18938, #36157, #41656, .T. ) ;
#28161 = AXIS2_PLACEMENT_3D ( 'NONE', #98, #15844, #871 ) ;
#28162 = ORIENTED_EDGE ( 'NONE', *, *, #38439, .T. ) ;
#28163 = PLANE ( 'NONE',  #19114 ) ;
#28164 = VECTOR ( 'NONE', #43109, 39.37007874015748143 ) ;
#28165 = DIRECTION ( 'NONE',  ( -1.000000000000000000, 0.000000000000000000, -0.000000000000000000 ) ) ;
#28166 = CARTESIAN_POINT ( 'NONE',  ( 0.000000000000000000, 1.574803149606302854, 0.000000000000000000 ) ) ;
#28167 = EDGE_CURVE ( 'NONE', #49749, #23247, #37794, .T. ) ;
#28168 = EDGE_LOOP ( 'NONE', ( #3904, #19061, #12994, #35798 ) ) ;
#28169 = EDGE_CURVE ( 'NONE', #30932, #22707, #25650, .T. ) ;
#28170 = VECTOR ( 'NONE', #29674, 39.37007874015748143 ) ;
#28171 = EDGE_LOOP ( 'NONE', ( #34710, #290, #14979, #6800 ) ) ;
#28172 = DIRECTION ( 'NONE',  ( 0.000000000000000000, 0.000000000000000000, 1.000000000000000000 ) ) ;
#28173 = VECTOR ( 'NONE', #27814, 39.37007874015748143 ) ;
#28174 = ORIENTED_EDGE ( 'NONE', *, *, #6454, .T. ) ;
#28175 = CARTESIAN_POINT ( 'NONE',  ( 0.1968503937007873017, 0.000000000000000000, -0.9448818897637765168 ) ) ;
#28176 = ORIENTED_EDGE ( 'NONE', *, *, #15173, .T. ) ;
#28177 = AXIS2_PLACEMENT_3D ( 'NONE', #28486, #1636, #29520 ) ;
#28178 = CARTESIAN_POINT ( 'NONE',  ( -1.166969139818016199, 3.267716535433071279, -0.6692913385826760875 ) ) ;
#28179 = CARTESIAN_POINT ( 'NONE',  ( 1.686111637834603938, 0.05492582915004715072, 0.9632209503012270080 ) ) ;
#28180 = LINE ( 'NONE', #24322, #6274 ) ;
#28181 = EDGE_CURVE ( 'NONE', #49388, #19556, #33421, .T. ) ;
#28182 = VERTEX_POINT ( 'NONE', #29529 ) ;
#28183 = ORIENTED_EDGE ( 'NONE', *, *, #19086, .T. ) ;
#28184 = ORIENTED_EDGE ( 'NONE', *, *, #9664, .T. ) ;
#28185 = LINE ( 'NONE', #33362, #46891 ) ;
#28186 = VERTEX_POINT ( 'NONE', #44745 ) ;
#28187 = ORIENTED_EDGE ( 'NONE', *, *, #20765, .T. ) ;
#28188 = ADVANCED_FACE ( 'NONE', ( #21783 ), #45002, .T. ) ;
#28189 = CARTESIAN_POINT ( 'NONE',  ( -2.159071745913425655, 1.046027471231291139, -1.366223401065049581 ) ) ;
#28190 = CARTESIAN_POINT ( 'NONE',  ( 0.07982360342473591996, 1.709180471932028711, 0.000000000000000000 ) ) ;
#28191 = CARTESIAN_POINT ( 'NONE',  ( -1.091055626815042645, 3.267716535433071279, -1.889763779527552146 ) ) ;
#28192 = B_SPLINE_CURVE_WITH_KNOTS ( 'NONE', 3,
 ( #13230, #36725, #17103, #32865 ),
 .UNSPECIFIED., .F., .F.,
 ( 4, 4 ),
 ( 0.01468254673471047073, 0.03075083447507073742 ),
 .UNSPECIFIED. ) ;
#28193 = ORIENTED_EDGE ( 'NONE', *, *, #19596, .F. ) ;
#28194 = CARTESIAN_POINT ( 'NONE',  ( -0.1184164328040565317, -0.6299212598425202314, -0.3547750388873516791 ) ) ;
#28195 = CARTESIAN_POINT ( 'NONE',  ( -2.422455304366706752, 1.574882862795218275, -0.1580547953490660518 ) ) ;
#28196 = EDGE_CURVE ( 'NONE', #14792, #39458, #6292, .T. ) ;
#28197 = CARTESIAN_POINT ( 'NONE',  ( -0.8942052331142552601, 3.267716535433071279, -0.3149606299212593941 ) ) ;
#28198 = ORIENTED_EDGE ( 'NONE', *, *, #19147, .F. ) ;
#28199 = CARTESIAN_POINT ( 'NONE',  ( 0.8291286199751974895, 1.205361022782829114E-17, -1.835126787948130556 ) ) ;
#28200 = CARTESIAN_POINT ( 'NONE',  ( -0.8942052331142552601, 0.000000000000000000, 1.889763779527550147 ) ) ;
#28201 = ORIENTED_EDGE ( 'NONE', *, *, #16552, .T. ) ;
#28202 = CARTESIAN_POINT ( 'NONE',  ( -0.9914495361339012991, 1.703811331058339373, 2.781765111341808705 ) ) ;
#28203 = ORIENTED_EDGE ( 'NONE', *, *, #16629, .T. ) ;
#28204 = EDGE_LOOP ( 'NONE', ( #29896, #13501, #24979, #38616, #41194, #41197, #16678, #24759, #37366, #21972, #20232 ) ) ;
#28205 = CARTESIAN_POINT ( 'NONE',  ( -0.2727639067037608278, 0.000000000000000000, -0.3543307086614175816 ) ) ;
#28206 = EDGE_CURVE ( 'NONE', #47575, #8060, #14282, .T. ) ;
#28208 = CIRCLE ( 'NONE', #47147, 2.165354330708661568 ) ;
#28207 = DIRECTION ( 'NONE',  ( -1.000000000000000000, 0.000000000000000000, 1.734723475976806848E-16 ) ) ;
#28209 = CARTESIAN_POINT ( 'NONE',  ( -1.905671854841497481, 1.689559879305088996, 2.256015092822653223 ) ) ;
#28210 = CARTESIAN_POINT ( 'NONE',  ( 0.8182917201112824834, 0.000000000000000000, 1.850393700787392293 ) ) ;
#28211 = ORIENTED_EDGE ( 'NONE', *, *, #17621, .F. ) ;
#28212 = ORIENTED_EDGE ( 'NONE', *, *, #7890, .F. ) ;
#28213 = VECTOR ( 'NONE', #2746, 39.37007874015748143 ) ;
#28214 = EDGE_CURVE ( 'NONE', #7202, #47691, #22040, .T. ) ;
#28215 = CIRCLE ( 'NONE', #5965, 2.086614173228346303 ) ;
#28216 = ORIENTED_EDGE ( 'NONE', *, *, #7310, .T. ) ;
#28217 = LINE ( 'NONE', #43958, #25278 ) ;
#28218 = CARTESIAN_POINT ( 'NONE',  ( 0.000000000000000000, 6.692913385826772199, 0.000000000000000000 ) ) ;
#28219 = VECTOR ( 'NONE', #12686, 39.37007874015748143 ) ;
#28220 = FACE_OUTER_BOUND ( 'NONE', #19822, .T. ) ;
#28221 = CARTESIAN_POINT ( 'NONE',  ( 0.8182917201112819283, 3.267716535433071279, -0.03937007874015881204 ) ) ;
#28222 = LINE ( 'NONE', #47298, #4799 ) ;
#28223 = ORIENTED_EDGE ( 'NONE', *, *, #3257, .T. ) ;
#28224 = DIRECTION ( 'NONE',  ( 1.734723475976806848E-16, 0.000000000000000000, 1.000000000000000000 ) ) ;
#28225 = CARTESIAN_POINT ( 'NONE',  ( -1.091055626815042645, 3.346456692913386100, -1.574803149606293529 ) ) ;
#28226 = EDGE_CURVE ( 'NONE', #18884, #2388, #1903, .T. ) ;
#28227 = ORIENTED_EDGE ( 'NONE', *, *, #35690, .F. ) ;
#28228 = CARTESIAN_POINT ( 'NONE',  ( 0.000000000000000000, 0.000000000000000000, -2.952755905511811552 ) ) ;
#28229 = CARTESIAN_POINT ( 'NONE',  ( 0.2156685157584260770, 1.722625337188476546, -2.945280361644574185 ) ) ;
#28230 = CARTESIAN_POINT ( 'NONE',  ( -0.8182917201112814842, 3.346456692913386100, 1.220472440944875281 ) ) ;
#28231 = EDGE_LOOP ( 'NONE', ( #28942, #7299, #22172, #31361 ) ) ;
#28232 = CARTESIAN_POINT ( 'NONE',  ( -1.393175312147127531, 0.000000000000000000, 1.048074961516273218 ) ) ;
#28233 = LINE ( 'NONE', #39611, #39016 ) ;
#28234 = EDGE_CURVE ( 'NONE', #21109, #38547, #41139, .T. ) ;
#28235 = CARTESIAN_POINT ( 'NONE',  ( 0.4696143004045479352, 3.267716535433071279, -0.1574803149606298636 ) ) ;
#28236 = ORIENTED_EDGE ( 'NONE', *, *, #2899, .F. ) ;
#28237 = PLANE ( 'NONE',  #18098 ) ;
#28238 = DIRECTION ( 'NONE',  ( -0.000000000000000000, 1.000000000000000000, -0.000000000000000000 ) ) ;
#28239 = ORIENTED_EDGE ( 'NONE', *, *, #3358, .T. ) ;
#28240 = CARTESIAN_POINT ( 'NONE',  ( 0.5786196242795136335, 3.267716535433071279, -2.086614173228340086 ) ) ;
#28241 = VECTOR ( 'NONE', #18574, 39.37007874015748143 ) ;
#28242 = FACE_OUTER_BOUND ( 'NONE', #515, .T. ) ;
#28243 = CARTESIAN_POINT ( 'NONE',  ( 0.07982360342473591996, 1.709180471932028711, 0.000000000000000000 ) ) ;
#28244 = CARTESIAN_POINT ( 'NONE',  ( 0.6150616064519864867, 0.03777100275179151589, 1.778883059170359493 ) ) ;
#28245 = VECTOR ( 'NONE', #6313, 39.37007874015748143 ) ;
#28246 = ORIENTED_EDGE ( 'NONE', *, *, #32502, .T. ) ;
#28247 = ORIENTED_EDGE ( 'NONE', *, *, #11756, .F. ) ;
#28248 = CARTESIAN_POINT ( 'NONE',  ( 1.636583440222563857, 0.000000000000000000, 0.1181102362204701633 ) ) ;
#28249 = FACE_OUTER_BOUND ( 'NONE', #40052, .T. ) ;
#28250 = ORIENTED_EDGE ( 'NONE', *, *, #8488, .F. ) ;
#28251 = VECTOR ( 'NONE', #21746, 39.37007874015748854 ) ;
#28252 = CARTESIAN_POINT ( 'NONE',  ( -0.6214413264104945434, 3.346456692913386100, -0.1574803149606301411 ) ) ;
#28253 = LINE ( 'NONE', #4775, #47449 ) ;
#28254 = CARTESIAN_POINT ( 'NONE',  ( -1.405314191946755997, 1.685393272164901646, 1.683309666213049560 ) ) ;
#28255 = CIRCLE ( 'NONE', #22483, 2.106299212598425008 ) ;
#28256 = CARTESIAN_POINT ( 'NONE',  ( -0.6214413264104945434, 3.346456692913386100, -0.9842519685039342603 ) ) ;
#28257 = VECTOR ( 'NONE', #24294, 39.37007874015748143 ) ;
#28258 = ORIENTED_EDGE ( 'NONE', *, *, #7820, .T. ) ;
#28259 = ORIENTED_EDGE ( 'NONE', *, *, #36794, .T. ) ;
#28260 = CARTESIAN_POINT ( 'NONE',  ( -0.8942052331142552601, 3.346456692913386100, -1.574803149606293529 ) ) ;
#28261 = DIRECTION ( 'NONE',  ( 1.000000000000000000, -0.000000000000000000, 0.000000000000000000 ) ) ;
#28262 = EDGE_CURVE ( 'NONE', #19788, #7819, #50300, .T. ) ;
#28263 = DIRECTION ( 'NONE',  ( 0.000000000000000000, 0.000000000000000000, 1.000000000000000000 ) ) ;
#28264 = CARTESIAN_POINT ( 'NONE',  ( 0.000000000000000000, 3.267716535433071279, -0.6692913385826758654 ) ) ;
#28265 = FACE_BOUND ( 'NONE', #47499, .T. ) ;
#28266 = CONICAL_SURFACE ( 'NONE', #34074, 2.244934639244524632, 1.554780866114618743 ) ;
#28267 = VERTEX_POINT ( 'NONE', #41158 ) ;
#28268 = CARTESIAN_POINT ( 'NONE',  ( 0.000000000000000000, 6.692913385826772199, 0.000000000000000000 ) ) ;
#28269 = ORIENTED_EDGE ( 'NONE', *, *, #47229, .T. ) ;
#28270 = ORIENTED_EDGE ( 'NONE', *, *, #20423, .F. ) ;
#28271 = CARTESIAN_POINT ( 'NONE',  ( -2.867773316779185677, 1.576133919414932638, -0.7050287376752426560 ) ) ;
#28272 = ADVANCED_FACE ( 'NONE', ( #49100 ), #45246, .F. ) ;
#28273 = EDGE_CURVE ( 'NONE', #25449, #5602, #36944, .T. ) ;
#28274 = EDGE_CURVE ( 'NONE', #30462, #42563, #427, .T. ) ;
#28275 = ORIENTED_EDGE ( 'NONE', *, *, #1423, .T. ) ;
#28276 = ORIENTED_EDGE ( 'NONE', *, *, #39649, .F. ) ;
#28277 = CARTESIAN_POINT ( 'NONE',  ( 1.181102362204724532, 0.5905511811023621549, 1.062992125984251413 ) ) ;
#28278 = UNCERTAINTY_MEASURE_WITH_UNIT (LENGTH_MEASURE( 1.000000000000000082E-05 ), #8809, 'distance_accuracy_value', 'NONE');
#28279 = EDGE_LOOP ( 'NONE', ( #35263, #41185, #21860, #21486 ) ) ;
#28280 = EDGE_CURVE ( 'NONE', #25218, #47368, #35908, .T. ) ;
#28281 = CARTESIAN_POINT ( 'NONE',  ( 0.8182917201112819283, 3.346456692913386100, 0.1574803149606286423 ) ) ;
#28282 = DIRECTION ( 'NONE',  ( -0.000000000000000000, 1.000000000000000000, -0.000000000000000000 ) ) ;
#28283 = DIRECTION ( 'NONE',  ( -0.000000000000000000, 0.000000000000000000, 1.000000000000000000 ) ) ;
#28284 = EDGE_CURVE ( 'NONE', #30522, #41853, #12789, .T. ) ;
#28285 = DIRECTION ( 'NONE',  ( 1.000000000000000000, 0.000000000000000000, -3.469446951953613696E-16 ) ) ;
#28286 = AXIS2_PLACEMENT_3D ( 'NONE', #4460, #35450, #27432 ) ;
#28287 = DIRECTION ( 'NONE',  ( 0.000000000000000000, 1.000000000000000000, 0.000000000000000000 ) ) ;
#28288 = DIRECTION ( 'NONE',  ( -0.000000000000000000, 1.000000000000000000, -0.000000000000000000 ) ) ;
#28289 = VERTEX_POINT ( 'NONE', #39777 ) ;
#28290 = CARTESIAN_POINT ( 'NONE',  ( -0.8942052331142547050, 3.346456692913386100, 1.259842519685033357 ) ) ;
#28291 = AXIS2_PLACEMENT_3D ( 'NONE', #19220, #34982, #11729 ) ;
#28292 = CARTESIAN_POINT ( 'NONE',  ( -1.905671854841497481, 1.555429617898292705, 2.256015092822653667 ) ) ;
#28293 = CARTESIAN_POINT ( 'NONE',  ( 1.950008968278537091, 5.905511811023623991, 0.9934589848971188131 ) ) ;
#28294 = AXIS2_PLACEMENT_3D ( 'NONE', #43881, #48502, #44404 ) ;
#28295 = ADVANCED_FACE ( 'NONE', ( #16803 ), #24802, .T. ) ;
#28296 = VERTEX_POINT ( 'NONE', #9055 ) ;
#28297 = CARTESIAN_POINT ( 'NONE',  ( -1.091055626815042645, 0.000000000000000000, 2.204724409448808764 ) ) ;
#28298 = DIRECTION ( 'NONE',  ( -1.000000000000000000, 0.000000000000000000, 1.734723475976806848E-16 ) ) ;
#28299 = ORIENTED_EDGE ( 'NONE', *, *, #17299, .F. ) ;
#28300 = LINE ( 'NONE', #32195, #10624 ) ;
#28301 = LINE ( 'NONE', #44045, #48049 ) ;
#28302 = EDGE_CURVE ( 'NONE', #54, #9880, #36170, .T. ) ;
#28303 = DIRECTION ( 'NONE',  ( -0.000000000000000000, -1.000000000000000000, -0.000000000000000000 ) ) ;
#28304 = VECTOR ( 'NONE', #28990, 39.37007874015748143 ) ;
#28305 = ORIENTED_EDGE ( 'NONE', *, *, #37514, .F. ) ;
#28306 = DIRECTION ( 'NONE',  ( -0.9989930665413151445, -0.000000000000000000, 0.04486483035050446017 ) ) ;
#28307 = VERTEX_POINT ( 'NONE', #4409 ) ;
#28308 = CARTESIAN_POINT ( 'NONE',  ( 0.8182917201112817063, 0.000000000000000000, -1.732283464566923614 ) ) ;
#28309 = DIRECTION ( 'NONE',  ( -1.000000000000000000, 0.000000000000000000, 1.734723475976806848E-16 ) ) ;
#28310 = CARTESIAN_POINT ( 'NONE',  ( 0.2727639067037610499, 0.000000000000000000, 2.362204724409437961 ) ) ;
#28311 = DIRECTION ( 'NONE',  ( 1.734723475976806848E-16, -0.000000000000000000, 1.000000000000000000 ) ) ;
#28312 = VERTEX_POINT ( 'NONE', #21189 ) ;
#28313 = ORIENTED_EDGE ( 'NONE', *, *, #11822, .T. ) ;
#28314 = CARTESIAN_POINT ( 'NONE',  ( 0.000000000000000000, 3.267716535433071279, -1.889763779527552146 ) ) ;
#28315 = EDGE_LOOP ( 'NONE', ( #8572, #17411, #21747, #13471, #806, #7113, #2946, #11992, #21179, #19795, #2256 ) ) ;
#28316 = CARTESIAN_POINT ( 'NONE',  ( 0.3136974817028395091, 1.508467219206862664, -2.936457595020219635 ) ) ;
#28317 = ORIENTED_EDGE ( 'NONE', *, *, #23122, .F. ) ;
#28318 = DIRECTION ( 'NONE',  ( -3.469446951953613696E-16, 0.000000000000000000, -1.000000000000000000 ) ) ;
#28319 = ORIENTED_EDGE ( 'NONE', *, *, #49585, .F. ) ;
#28320 = FACE_OUTER_BOUND ( 'NONE', #47403, .T. ) ;
#28321 = CONICAL_SURFACE ( 'NONE', #9356, 2.165354330708661568, 0.2617993877991570129 ) ;
#28322 = FACE_OUTER_BOUND ( 'NONE', #29660, .T. ) ;
#28323 = ORIENTED_EDGE ( 'NONE', *, *, #21703, .F. ) ;
#28324 = CARTESIAN_POINT ( 'NONE',  ( 2.708693820785017525, 1.662986522273777412, -1.175591050822254457 ) ) ;
#28325 = VECTOR ( 'NONE', #35613, 39.37007874015748143 ) ;
#28326 = ORIENTED_EDGE ( 'NONE', *, *, #15655, .T. ) ;
#28327 = VECTOR ( 'NONE', #24394, 39.37007874015748143 ) ;
#28328 = VECTOR ( 'NONE', #22519, 39.37007874015748143 ) ;
#28329 = CARTESIAN_POINT ( 'NONE',  ( 1.015142113812069313, 3.267716535433071279, -3.521981712565032882E-16 ) ) ;
#28330 = EDGE_CURVE ( 'NONE', #15665, #35860, #36425, .T. ) ;
#28331 = ADVANCED_FACE ( 'NONE', ( #32302 ), #28667, .T. ) ;
#28332 = ORIENTED_EDGE ( 'NONE', *, *, #29410, .T. ) ;
#28333 = ORIENTED_EDGE ( 'NONE', *, *, #44186, .T. ) ;
#28334 = CARTESIAN_POINT ( 'NONE',  ( 2.715141060683428531, 0.000000000000000000, -1.160506983230063405 ) ) ;
#28335 = ADVANCED_FACE ( 'NONE', ( #48252 ), #47736, .F. ) ;
#28336 = CIRCLE ( 'NONE', #14349, 2.246510896728926010 ) ;
#28337 = ORIENTED_EDGE ( 'NONE', *, *, #11979, .F. ) ;
#28338 = CARTESIAN_POINT ( 'NONE',  ( 2.106197740627111514, 3.346456692913386100, -0.7874015748031473194 ) ) ;
#28339 = ORIENTED_EDGE ( 'NONE', *, *, #10492, .F. ) ;
#28340 = CARTESIAN_POINT ( 'NONE',  ( 1.574803149606299524, 1.172985819482486924, -0.9842519685039369248 ) ) ;
#28341 = LINE ( 'NONE', #24484, #39874 ) ;
#28342 = CARTESIAN_POINT ( 'NONE',  ( -1.735586374879336757, 5.905511811023623991, -2.388829707800050883 ) ) ;
#28343 = ORIENTED_EDGE ( 'NONE', *, *, #36353, .F. ) ;
#28344 = EDGE_LOOP ( 'NONE', ( #16087, #18465, #15929, #7334 ) ) ;
#28345 = CARTESIAN_POINT ( 'NONE',  ( -1.661821349926434932, 1.574803149606302854, 1.388203579611951843 ) ) ;
#28346 = CARTESIAN_POINT ( 'NONE',  ( 2.309000164489917406, 1.744884814208895296, 0.2631132722234555410 ) ) ;
#28347 = FACE_OUTER_BOUND ( 'NONE', #35457, .T. ) ;
#28348 = CARTESIAN_POINT ( 'NONE',  ( -1.909347346926324906, 3.346456692913386100, -1.102362204724405492 ) ) ;
#28349 = ADVANCED_FACE ( 'NONE', ( #13191 ), #24958, .T. ) ;
#28350 = LINE ( 'NONE', #48953, #10350 ) ;
#28351 = CARTESIAN_POINT ( 'NONE',  ( 2.793030215715258446, 1.451280567205322836, 0.9592557174602683867 ) ) ;
#28352 = ADVANCED_FACE ( 'NONE', ( #20665 ), #48761, .F. ) ;
#28353 = DIRECTION ( 'NONE',  ( -1.000000000000000000, 0.000000000000000000, 0.000000000000000000 ) ) ;
#28354 = ORIENTED_EDGE ( 'NONE', *, *, #45134, .T. ) ;
#28355 = DIRECTION ( 'NONE',  ( 0.000000000000000000, 1.000000000000000000, 0.000000000000000000 ) ) ;
#28356 = EDGE_CURVE ( 'NONE', #23316, #38999, #20410, .T. ) ;
#28357 = CIRCLE ( 'NONE', #10206, 2.165354330708661568 ) ;
#28358 = EDGE_LOOP ( 'NONE', ( #42074, #22265, #48059, #6365 ) ) ;
#28359 = DIRECTION ( 'NONE',  ( 0.000000000000000000, -1.000000000000000000, 0.000000000000000000 ) ) ;
#28360 = AXIS2_PLACEMENT_3D ( 'NONE', #41066, #9564, #36679 ) ;
#28361 = EDGE_CURVE ( 'NONE', #41060, #38999, #34727, .T. ) ;
#28362 = VECTOR ( 'NONE', #25370, 39.37007874015748143 ) ;
#28363 = ORIENTED_EDGE ( 'NONE', *, *, #30297, .F. ) ;
#28364 = AXIS2_PLACEMENT_3D ( 'NONE', #27726, #23602, #8118 ) ;
#28366 = VECTOR ( 'NONE', #35918, 39.37007874015748143 ) ;
#28365 = DIRECTION ( 'NONE',  ( 1.000000000000000000, 0.000000000000000000, 0.000000000000000000 ) ) ;
#28367 = DIRECTION ( 'NONE',  ( 1.000000000000000000, 0.000000000000000000, 0.000000000000000000 ) ) ;
#28368 = FACE_OUTER_BOUND ( 'NONE', #34041, .T. ) ;
#28369 = CARTESIAN_POINT ( 'NONE',  ( 1.363819533518803029, 3.267716535433071279, -1.417322834645665219 ) ) ;
#28370 = ORIENTED_EDGE ( 'NONE', *, *, #31430, .F. ) ;
#28371 = LINE ( 'NONE', #33040, #43905 ) ;
#28372 = CONICAL_SURFACE ( 'NONE', #20979, 1.850107469027523210, 0.6386652850508578450 ) ;
#28373 = CARTESIAN_POINT ( 'NONE',  ( 1.979793062125284608, 1.750113821271474857, 2.191257344206569257 ) ) ;
#28374 = VERTEX_POINT ( 'NONE', #44658 ) ;
#28375 = CARTESIAN_POINT ( 'NONE',  ( -1.909347346926324906, 3.346456692913386100, 1.220472440944875059 ) ) ;
#28376 = VERTEX_POINT ( 'NONE', #40301 ) ;
#28377 = FACE_OUTER_BOUND ( 'NONE', #6603, .T. ) ;
#28378 = CARTESIAN_POINT ( 'NONE',  ( 1.636583440222563857, 3.346456692913386100, -1.161035397307311917E-15 ) ) ;
#28379 = CARTESIAN_POINT ( 'NONE',  ( -0.8182917201112814842, 3.346456692913386100, 0.5905511811023582691 ) ) ;
#28380 = ORIENTED_EDGE ( 'NONE', *, *, #34603, .T. ) ;
#28381 = ORIENTED_EDGE ( 'NONE', *, *, #41481, .F. ) ;
#28382 = CARTESIAN_POINT ( 'NONE',  ( 0.1968503937007877735, 3.267716535433071279, 0.7480314960629874665 ) ) ;
#28383 = CARTESIAN_POINT ( 'NONE',  ( -2.182111253630085290, 0.000000000000000000, 0.6299212598425164567 ) ) ;
#28384 = CARTESIAN_POINT ( 'NONE',  ( 0.2727639067037602172, 3.346456692913386100, -1.732283464566922726 ) ) ;
#28385 = CARTESIAN_POINT ( 'NONE',  ( 0.000000000000000000, 3.267716535433071279, 0.9448818897637749625 ) ) ;
#28386 = CARTESIAN_POINT ( 'NONE',  ( -1.439733046521776361, 3.267716535433071279, 0.7480314960629874665 ) ) ;
#28387 = VERTEX_POINT ( 'NONE', #25056 ) ;
#28388 = CARTESIAN_POINT ( 'NONE',  ( -1.695772546416001836, 5.905511811023623991, -2.417756147381374010 ) ) ;
#28389 = EDGE_CURVE ( 'NONE', #3623, #28112, #40811, .T. ) ;
#28390 = VECTOR ( 'NONE', #18143, 39.37007874015748143 ) ;
#28391 = ADVANCED_FACE ( 'NONE', ( #44914 ), #37200, .F. ) ;
#28392 = VERTEX_POINT ( 'NONE', #45665 ) ;
#28393 = VECTOR ( 'NONE', #40559, 39.37007874015748143 ) ;
#28394 = ORIENTED_EDGE ( 'NONE', *, *, #31857, .F. ) ;
#28395 = EDGE_CURVE ( 'NONE', #43099, #30730, #33330, .T. ) ;
#28396 = VECTOR ( 'NONE', #44560, 39.37007874015748143 ) ;
#28397 = ORIENTED_EDGE ( 'NONE', *, *, #48118, .T. ) ;
#28398 = CARTESIAN_POINT ( 'NONE',  ( 2.339241080213585899, 1.755713673067765379, 1.802537235681918037 ) ) ;
#28399 = VECTOR ( 'NONE', #28355, 39.37007874015748143 ) ;
#28400 = CARTESIAN_POINT ( 'NONE',  ( -0.2480359799030329715, 2.755905511811024056, 0.2799391584775194342 ) ) ;
#28401 = DIRECTION ( 'NONE',  ( -0.9998717552508122886, -0.01601477604151182316, 0.000000000000000000 ) ) ;
#28402 = CARTESIAN_POINT ( 'NONE',  ( 0.000000000000000000, 3.267716535433071279, 0.000000000000000000 ) ) ;
#28403 = EDGE_LOOP ( 'NONE', ( #34194, #15845, #28058, #23279 ) ) ;
#28404 = EDGE_LOOP ( 'NONE', ( #38045, #49971, #10920, #16027 ) ) ;
#28405 = CIRCLE ( 'NONE', #39989, 1.743387098533651480 ) ;
#28406 = DIRECTION ( 'NONE',  ( 0.000000000000000000, -1.000000000000000000, 0.000000000000000000 ) ) ;
#28407 = LINE ( 'NONE', #9057, #24990 ) ;
#28408 = FACE_OUTER_BOUND ( 'NONE', #14676, .T. ) ;
#28409 = DIRECTION ( 'NONE',  ( -0.6427876096865403621, -0.7660444431189770143, 0.000000000000000000 ) ) ;
#28410 = EDGE_CURVE ( 'NONE', #13181, #45498, #21697, .T. ) ;
#28411 = DIRECTION ( 'NONE',  ( 1.000000000000000000, 0.000000000000000000, -3.469446951953613696E-16 ) ) ;
#28412 = LINE ( 'NONE', #13708, #12715 ) ;
#28413 = PLANE ( 'NONE',  #36816 ) ;
#28414 = ORIENTED_EDGE ( 'NONE', *, *, #40394, .T. ) ;
#28415 = DIRECTION ( 'NONE',  ( 0.7071067811865463515, 0.000000000000000000, -0.7071067811865487940 ) ) ;
#28416 = LINE ( 'NONE', #35666, #44972 ) ;
#28417 = EDGE_CURVE ( 'NONE', #329, #6620, #22459, .T. ) ;
#28418 = ORIENTED_EDGE ( 'NONE', *, *, #27590, .F. ) ;
#28419 = ORIENTED_EDGE ( 'NONE', *, *, #14414, .F. ) ;
#28420 = CARTESIAN_POINT ( 'NONE',  ( 1.091055626815042645, 0.000000000000000000, 1.062992125984246083 ) ) ;
#28421 = DIRECTION ( 'NONE',  ( -0.000000000000000000, 1.000000000000000000, -0.000000000000000000 ) ) ;
#28422 = DIRECTION ( 'NONE',  ( -3.469446951953613696E-16, 0.000000000000000000, -1.000000000000000000 ) ) ;
#28423 = ORIENTED_EDGE ( 'NONE', *, *, #12176, .F. ) ;
#28424 = AXIS2_PLACEMENT_3D ( 'NONE', #18334, #10335, #37966 ) ;
#28425 = VERTEX_POINT ( 'NONE', #17822 ) ;
#28426 = VECTOR ( 'NONE', #28353, 39.37007874015748143 ) ;
#28427 = CARTESIAN_POINT ( 'NONE',  ( 2.164658444855302122, 5.905511811023623991, -0.04795272066889885720 ) ) ;
#28428 = ORIENTED_EDGE ( 'NONE', *, *, #45054, .F. ) ;
#28429 = CARTESIAN_POINT ( 'NONE',  ( -0.07591351300297333182, 3.267716535433071279, -1.732283464566922726 ) ) ;
#28430 = VECTOR ( 'NONE', #34489, 39.37007874015748143 ) ;
#28431 = ORIENTED_EDGE ( 'NONE', *, *, #50619, .F. ) ;
#28432 = DIRECTION ( 'NONE',  ( 1.734723475976806848E-16, 0.000000000000000000, 1.000000000000000000 ) ) ;
#28433 = FACE_OUTER_BOUND ( 'NONE', #6426, .T. ) ;
#28434 = LINE ( 'NONE', #4438, #34290 ) ;
#28435 = ORIENTED_EDGE ( 'NONE', *, *, #17457, .F. ) ;
#28436 = ORIENTED_EDGE ( 'NONE', *, *, #25100, .F. ) ;
#28437 = ORIENTED_EDGE ( 'NONE', *, *, #6581, .T. ) ;
#28438 = VECTOR ( 'NONE', #36269, 39.37007874015748854 ) ;
#28439 = DIRECTION ( 'NONE',  ( 1.734723475976806848E-16, -0.000000000000000000, 1.000000000000000000 ) ) ;
#28440 = ORIENTED_EDGE ( 'NONE', *, *, #45460, .T. ) ;
#28441 = ORIENTED_EDGE ( 'NONE', *, *, #49031, .F. ) ;
#28442 = PLANE ( 'NONE',  #36339 ) ;
#28443 = CARTESIAN_POINT ( 'NONE',  ( 1.091055626815042645, 0.000000000000000000, -1.141732283464564013 ) ) ;
#28444 = CARTESIAN_POINT ( 'NONE',  ( 2.312113436335841321, 1.646509482104762334, 0.2635349935491774209 ) ) ;
#28445 = ORIENTED_EDGE ( 'NONE', *, *, #27624, .F. ) ;
#28446 = LINE ( 'NONE', #24593, #42767 ) ;
#28447 = CARTESIAN_POINT ( 'NONE',  ( -0.9788642269881570046, 0.000000000000000000, 1.542392924267547594 ) ) ;
#28448 = CARTESIAN_POINT ( 'NONE',  ( -0.8942052331142552601, 3.346456692913386100, -0.6299212598425177889 ) ) ;
#28449 = ORIENTED_EDGE ( 'NONE', *, *, #28884, .T. ) ;
#28450 = CARTESIAN_POINT ( 'NONE',  ( 0.5455278134075211005, 0.000000000000000000, -1.141732283464564013 ) ) ;
#28451 = DIRECTION ( 'NONE',  ( 1.000000000000000000, 0.000000000000000000, -3.469446951953613696E-16 ) ) ;
#28452 = EDGE_CURVE ( 'NONE', #12460, #1675, #13953, .T. ) ;
#28453 = EDGE_LOOP ( 'NONE', ( #43865, #23021, #37512, #22287 ) ) ;
#28454 = EDGE_CURVE ( 'NONE', #32849, #31431, #4732, .T. ) ;
#28455 = DIRECTION ( 'NONE',  ( -0.000000000000000000, 1.000000000000000000, 0.000000000000000000 ) ) ;
#28456 = EDGE_LOOP ( 'NONE', ( #17487, #10482, #2717, #39678 ) ) ;
#28457 = ORIENTED_EDGE ( 'NONE', *, *, #40399, .T. ) ;
#28458 = CARTESIAN_POINT ( 'NONE',  ( 1.363819533518803251, 0.000000000000000000, 0.4724409448818871482 ) ) ;
#28459 = FACE_OUTER_BOUND ( 'NONE', #40542, .T. ) ;
#28460 = EDGE_CURVE ( 'NONE', #42073, #15363, #45161, .T. ) ;
#28461 = LINE ( 'NONE', #48809, #16509 ) ;
#28462 = CARTESIAN_POINT ( 'NONE',  ( -2.164823134740035737, 1.574803149606302854, -0.04796011690018223833 ) ) ;
#28463 = EDGE_CURVE ( 'NONE', #17559, #21385, #6464, .T. ) ;
#28464 = CARTESIAN_POINT ( 'NONE',  ( 2.793030215715258446, 1.664308485742666877, 0.9592557174602684977 ) ) ;
#28465 = VERTEX_POINT ( 'NONE', #21957 ) ;
#28466 = ORIENTED_EDGE ( 'NONE', *, *, #140, .T. ) ;
#28467 = VECTOR ( 'NONE', #27781, 39.37007874015748143 ) ;
#28468 = AXIS2_PLACEMENT_3D ( 'NONE', #24003, #16261, #12388 ) ;
#28469 = FACE_OUTER_BOUND ( 'NONE', #11303, .T. ) ;
#28470 = B_SPLINE_CURVE_WITH_KNOTS ( 'NONE', 3,
 ( #28081, #32232, #36872, #28598 ),
 .UNSPECIFIED., .F., .F.,
 ( 4, 4 ),
 ( 0.01239106743709809423, 0.03073847721854806869 ),
 .UNSPECIFIED. ) ;
#28471 = ORIENTED_EDGE ( 'NONE', *, *, #28417, .T. ) ;
#28472 = DIRECTION ( 'NONE',  ( -0.000000000000000000, 1.000000000000000000, -0.000000000000000000 ) ) ;
#28473 = CARTESIAN_POINT ( 'NONE',  ( 0.5286458662987441048, 1.205361022782829114E-17, 2.100489422084715230 ) ) ;
#28474 = CIRCLE ( 'NONE', #30144, 2.165354330708661568 ) ;
#28475 = EDGE_CURVE ( 'NONE', #4194, #11914, #11754, .T. ) ;
#28476 = AXIS2_PLACEMENT_3D ( 'NONE', #29986, #5979, #45703 ) ;
#28477 = DIRECTION ( 'NONE',  ( -0.000000000000000000, 1.000000000000000000, -0.000000000000000000 ) ) ;
#28478 = DIRECTION ( 'NONE',  ( -1.000000000000000000, 0.000000000000000000, 1.734723475976806848E-16 ) ) ;
#28479 = DIRECTION ( 'NONE',  ( 1.000000000000000000, 0.000000000000000000, -3.469446951953613696E-16 ) ) ;
#28480 = VECTOR ( 'NONE', #44562, 39.37007874015748143 ) ;
#28481 = VERTEX_POINT ( 'NONE', #25309 ) ;
#28482 = DIRECTION ( 'NONE',  ( -1.000000000000000000, 0.000000000000000000, 1.734723475976806848E-16 ) ) ;
#28483 = ADVANCED_FACE ( 'NONE', ( #1817 ), #40622, .T. ) ;
#28484 = DIRECTION ( 'NONE',  ( -0.6234898018587431423, 0.000000000000000000, 0.7818314824680221431 ) ) ;
#28485 = ORIENTED_EDGE ( 'NONE', *, *, #5990, .T. ) ;
#28486 = CARTESIAN_POINT ( 'NONE',  ( 0.8182917201112817063, 0.000000000000000000, -1.417322834645664331 ) ) ;
#28487 = DIRECTION ( 'NONE',  ( 0.000000000000000000, 0.000000000000000000, -1.000000000000000000 ) ) ;
#28488 = LINE ( 'NONE', #47821, #45232 ) ;
#28489 = EDGE_CURVE ( 'NONE', #44295, #46164, #49276, .T. ) ;
#28490 = ORIENTED_EDGE ( 'NONE', *, *, #7548, .F. ) ;
#28491 = CARTESIAN_POINT ( 'NONE',  ( -0.9788642269881570046, 0.000000000000000000, 1.542392924267547594 ) ) ;
#28492 = DIRECTION ( 'NONE',  ( -1.000000000000000000, 0.000000000000000000, 1.734723475976806848E-16 ) ) ;
#28493 = CARTESIAN_POINT ( 'NONE',  ( 0.9914495361338626633, 5.905511811023623103, 2.781765111341825136 ) ) ;
#28494 = ORIENTED_EDGE ( 'NONE', *, *, #5465, .F. ) ;
#28495 = DIRECTION ( 'NONE',  ( -3.469446951953613696E-16, 0.000000000000000000, -1.000000000000000000 ) ) ;
#28496 = DIRECTION ( 'NONE',  ( 1.000000000000000000, 0.000000000000000000, 0.000000000000000000 ) ) ;
#28497 = ORIENTED_EDGE ( 'NONE', *, *, #49576, .F. ) ;
#28498 = DIRECTION ( 'NONE',  ( -0.000000000000000000, 1.000000000000000000, -0.000000000000000000 ) ) ;
#28499 = EDGE_CURVE ( 'NONE', #16378, #32340, #49772, .T. ) ;
#28500 = DIRECTION ( 'NONE',  ( -1.000000000000000000, 0.000000000000000000, -0.000000000000000000 ) ) ;
#28501 = DIRECTION ( 'NONE',  ( 0.000000000000000000, 0.000000000000000000, -1.000000000000000000 ) ) ;
#28502 = CARTESIAN_POINT ( 'NONE',  ( -2.076715649576790224, 1.576214352228098470, 0.6230206298219045369 ) ) ;
#28503 = ORIENTED_EDGE ( 'NONE', *, *, #27817, .F. ) ;
#28504 = ORIENTED_EDGE ( 'NONE', *, *, #5607, .F. ) ;
#28505 = DIRECTION ( 'NONE',  ( 1.000000000000000000, 0.000000000000000000, 0.000000000000000000 ) ) ;
#28506 = AXIS2_PLACEMENT_3D ( 'NONE', #7289, #23031, #38781 ) ;
#28507 = LINE ( 'NONE', #13543, #2385 ) ;
#28508 = VECTOR ( 'NONE', #43059, 39.37007874015748143 ) ;
#28509 = EDGE_LOOP ( 'NONE', ( #33836, #9561, #44202, #39176 ) ) ;
#28510 = CARTESIAN_POINT ( 'NONE',  ( 0.08139965876239094178, 1.610780518492231694, 0.000000000000000000 ) ) ;
#28511 = CARTESIAN_POINT ( 'NONE',  ( -2.182111253630085290, 3.346456692913386100, 0.3149606299212578953 ) ) ;
#28512 = PLANE ( 'NONE',  #30225 ) ;
#28513 = CONICAL_SURFACE ( 'NONE', #6269, 2.246510896728926010, 0.01601546068027819014 ) ;
#28514 = LINE ( 'NONE', #44264, #25691 ) ;
#28515 = ORIENTED_EDGE ( 'NONE', *, *, #3050, .F. ) ;
#28516 = ORIENTED_EDGE ( 'NONE', *, *, #44539, .F. ) ;
#28517 = DIRECTION ( 'NONE',  ( 1.734723475976806848E-16, -0.000000000000000000, 1.000000000000000000 ) ) ;
#28518 = CARTESIAN_POINT ( 'NONE',  ( 0.7423782071083087075, 3.267716535433071279, -0.9448818897637765168 ) ) ;
#28519 = AXIS2_PLACEMENT_3D ( 'NONE', #8080, #43436, #3448 ) ;
#28520 = DIRECTION ( 'NONE',  ( -0.000000000000000000, 1.000000000000000000, -0.000000000000000000 ) ) ;
#28521 = ORIENTED_EDGE ( 'NONE', *, *, #33568, .T. ) ;
#28522 = CARTESIAN_POINT ( 'NONE',  ( -0.07591351300297340121, 3.267716535433071279, -0.3543307086614175816 ) ) ;
#28524 = VECTOR ( 'NONE', #4701, 39.37007874015748143 ) ;
#28523 = FACE_BOUND ( 'NONE', #44765, .T. ) ;
#28525 = ORIENTED_EDGE ( 'NONE', *, *, #38026, .F. ) ;
#28526 = LINE ( 'NONE', #44276, #1840 ) ;
#28527 = VERTEX_POINT ( 'NONE', #25820 ) ;
#28528 = VERTEX_POINT ( 'NONE', #41072 ) ;
#28529 = LINE ( 'NONE', #44279, #9391 ) ;
#28530 = EDGE_CURVE ( 'NONE', #35466, #28267, #41322, .T. ) ;
#28531 = EDGE_CURVE ( 'NONE', #31184, #37535, #2332, .T. ) ;
#28532 = ORIENTED_EDGE ( 'NONE', *, *, #4455, .T. ) ;
#28533 = EDGE_LOOP ( 'NONE', ( #42055, #47464, #31556, #15424 ) ) ;
#28534 = LINE ( 'NONE', #19763, #17839 ) ;
#28535 = EDGE_CURVE ( 'NONE', #50863, #33328, #29698, .T. ) ;
#28536 = VERTEX_POINT ( 'NONE', #45922 ) ;
#28537 = FACE_OUTER_BOUND ( 'NONE', #46641, .T. ) ;
#28538 = DIRECTION ( 'NONE',  ( -0.000000000000000000, 1.000000000000000000, -0.000000000000000000 ) ) ;
#28539 = DIRECTION ( 'NONE',  ( -0.000000000000000000, 1.000000000000000000, -0.000000000000000000 ) ) ;
#28540 = VECTOR ( 'NONE', #29, 39.37007874015748143 ) ;
#28541 = DIRECTION ( 'NONE',  ( 0.000000000000000000, 0.000000000000000000, 1.000000000000000000 ) ) ;
#28542 = DIRECTION ( 'NONE',  ( -0.9998717552508121775, -0.01601477604151182663, 0.000000000000000000 ) ) ;
#28543 = CARTESIAN_POINT ( 'NONE',  ( 0.000000000000000000, 3.267716535433071279, 0.7874015748031456541 ) ) ;
#28544 = CIRCLE ( 'NONE', #36820, 1.850107469027523432 ) ;
#28545 = ORIENTED_EDGE ( 'NONE', *, *, #8147, .T. ) ;
#28546 = DIRECTION ( 'NONE',  ( 1.000000000000000000, 0.000000000000000000, 0.000000000000000000 ) ) ;
#28547 = VECTOR ( 'NONE', #36102, 39.37007874015748143 ) ;
#28548 = CARTESIAN_POINT ( 'NONE',  ( -1.363819533518803029, 3.346456692913386100, 0.1574803149606287811 ) ) ;
#28549 = AXIS2_PLACEMENT_3D ( 'NONE', #18688, #19173, #50617 ) ;
#28550 = CARTESIAN_POINT ( 'NONE',  ( 2.715141060683428531, 5.905511811023623991, -1.160506983230062739 ) ) ;
#28551 = ORIENTED_EDGE ( 'NONE', *, *, #37368, .T. ) ;
#28552 = LINE ( 'NONE', #47880, #32257 ) ;
#28553 = DIRECTION ( 'NONE',  ( 1.734723475976806848E-16, -0.000000000000000000, 1.000000000000000000 ) ) ;
#28554 = ORIENTED_EDGE ( 'NONE', *, *, #31514, .F. ) ;
#28555 = CARTESIAN_POINT ( 'NONE',  ( -1.166969139818015977, 3.346456692913386100, 1.732283464566920950 ) ) ;
#28556 = VECTOR ( 'NONE', #40678, 39.37007874015748143 ) ;
#28557 = EDGE_CURVE ( 'NONE', #41994, #1801, #26329, .T. ) ;
#28558 = CARTESIAN_POINT ( 'NONE',  ( 2.528673309384623646, 1.751762191246605260, -0.1628250514548083838 ) ) ;
#28559 = CARTESIAN_POINT ( 'NONE',  ( 2.017116292511733189, 3.267716535433071279, -0.7874015748031473194 ) ) ;
#28560 = AXIS2_PLACEMENT_3D ( 'NONE', #48918, #24965, #1219 ) ;
#28561 = ORIENTED_EDGE ( 'NONE', *, *, #30695, .T. ) ;
#28562 = PLANE ( 'NONE',  #10072 ) ;
#28563 = ORIENTED_EDGE ( 'NONE', *, *, #24349, .F. ) ;
#28564 = FACE_BOUND ( 'NONE', #23566, .T. ) ;
#28565 = ADVANCED_FACE ( 'NONE', ( #18081 ), #42075, .F. ) ;
#28566 = PLANE ( 'NONE',  #43201 ) ;
#28567 = CARTESIAN_POINT ( 'NONE',  ( 0.000000000000000000, 3.267716535433071279, -1.732283464566922726 ) ) ;
#28568 = PLANE ( 'NONE',  #7811 ) ;
#28569 = ORIENTED_EDGE ( 'NONE', *, *, #18761, .F. ) ;
#28570 = EDGE_LOOP ( 'NONE', ( #48414, #17519, #48123, #34007 ) ) ;
#28571 = CARTESIAN_POINT ( 'NONE',  ( 1.052882392200863215, 1.637204117213755250, 2.758708974820646809 ) ) ;
#28572 = ORIENTED_EDGE ( 'NONE', *, *, #28104, .T. ) ;
#28573 = ADVANCED_FACE ( 'NONE', ( #2836 ), #40303, .F. ) ;
#28574 = CARTESIAN_POINT ( 'NONE',  ( 1.015142113812069091, 3.267716535433071279, -3.521981712565031896E-16 ) ) ;
#28575 = VERTEX_POINT ( 'NONE', #21193 ) ;
#28576 = ADVANCED_FACE ( 'NONE', ( #9569 ), #36427, .F. ) ;
#28577 = CARTESIAN_POINT ( 'NONE',  ( -1.712496953225537188, 3.346456692913386100, 0.2755905511810996522 ) ) ;
#28578 = ORIENTED_EDGE ( 'NONE', *, *, #36577, .T. ) ;
#28579 = DIRECTION ( 'NONE',  ( 0.000000000000000000, -1.000000000000000000, 0.000000000000000000 ) ) ;
#28580 = VECTOR ( 'NONE', #3035, 39.37007874015748143 ) ;
#28581 = LINE ( 'NONE', #21106, #41316 ) ;
#28582 = AXIS2_PLACEMENT_3D ( 'NONE', #22895, #38893, #42252 ) ;
#28583 = ORIENTED_EDGE ( 'NONE', *, *, #14442, .T. ) ;
#28584 = AXIS2_PLACEMENT_3D ( 'NONE', #15594, #39084, #19955 ) ;
#28585 = CARTESIAN_POINT ( 'NONE',  ( 1.223349603905365068, 0.04751384826852676074, 1.475034436811822669 ) ) ;
#28586 = ORIENTED_EDGE ( 'NONE', *, *, #27416, .T. ) ;
#28587 = ADVANCED_FACE ( 'NONE', ( #36946, #36172 ), #32829, .F. ) ;
#28588 = CARTESIAN_POINT ( 'NONE',  ( 0.000000000000000000, 3.346456692913386100, 0.000000000000000000 ) ) ;
#28589 = VECTOR ( 'NONE', #20209, 39.37007874015748143 ) ;
#28590 = ORIENTED_EDGE ( 'NONE', *, *, #24521, .T. ) ;
#28591 = ORIENTED_EDGE ( 'NONE', *, *, #2960, .T. ) ;
#28592 = EDGE_CURVE ( 'NONE', #5349, #28852, #9312, .T. ) ;
#28593 = ADVANCED_FACE ( 'NONE', ( #47994 ), #16805, .T. ) ;
#28594 = CARTESIAN_POINT ( 'NONE',  ( 2.813305137472101425, 1.450017550732547456, 0.8968559245517169209 ) ) ;
#28595 = CONICAL_SURFACE ( 'NONE', #31076, 3.483074324928249421, 1.244861948955335196 ) ;
#28596 = EDGE_CURVE ( 'NONE', #35032, #50405, #44156, .T. ) ;
#28597 = ORIENTED_EDGE ( 'NONE', *, *, #42702, .F. ) ;
#28598 = CARTESIAN_POINT ( 'NONE',  ( -0.4788131938641533303, 1.711801685632677428, 2.914091152102185944 ) ) ;
#28599 = ORIENTED_EDGE ( 'NONE', *, *, #45349, .T. ) ;
#28600 = CARTESIAN_POINT ( 'NONE',  ( 0.7423782071083082634, 0.000000000000000000, -2.086614173228340086 ) ) ;
#28601 = LINE ( 'NONE', #44087, #34938 ) ;
#28602 = CARTESIAN_POINT ( 'NONE',  ( 0.07982360342473591996, 1.709180471932028711, 0.000000000000000000 ) ) ;
#28603 = EDGE_CURVE ( 'NONE', #23841, #16862, #35671, .T. ) ;
#28604 = VERTEX_POINT ( 'NONE', #4926 ) ;
#28605 = DIRECTION ( 'NONE',  ( 0.000000000000000000, 1.000000000000000000, 0.000000000000000000 ) ) ;
#28606 = DIRECTION ( 'NONE',  ( -0.000000000000000000, 1.000000000000000000, -0.000000000000000000 ) ) ;
#28607 = CARTESIAN_POINT ( 'NONE',  ( 2.623503965249849301, 1.760141956857387724, 1.355882097269874187 ) ) ;
#28608 = DIRECTION ( 'NONE',  ( -0.000000000000000000, 1.000000000000000000, -0.000000000000000000 ) ) ;
#28609 = PLANE ( 'NONE',  #49882 ) ;
#28610 = CARTESIAN_POINT ( 'NONE',  ( 0.000000000000000000, 3.267716535433071279, -0.1968503937007886062 ) ) ;
#28611 = DIRECTION ( 'NONE',  ( 0.7227948638273878901, -8.024280841161103757E-17, 0.6910626489868684219 ) ) ;
#28612 = ORIENTED_EDGE ( 'NONE', *, *, #28592, .F. ) ;
#28613 = CARTESIAN_POINT ( 'NONE',  ( -1.985260859929297572, 3.346456692913386100, -6.146657985744592735E-16 ) ) ;
#28614 = VECTOR ( 'NONE', #49092, 39.37007874015748143 ) ;
#28615 = EDGE_CURVE ( 'NONE', #10739, #46962, #24804, .T. ) ;
#28616 = DIRECTION ( 'NONE',  ( 0.000000000000000000, 0.000000000000000000, 1.000000000000000000 ) ) ;
#28617 = ORIENTED_EDGE ( 'NONE', *, *, #8744, .T. ) ;
#28618 = VECTOR ( 'NONE', #15656, 39.37007874015748143 ) ;
#28619 = LINE ( 'NONE', #9262, #44876 ) ;
#28620 = ORIENTED_EDGE ( 'NONE', *, *, #28972, .F. ) ;
#28621 = CARTESIAN_POINT ( 'NONE',  ( 0.000000000000000000, 3.267716535433071279, 0.000000000000000000 ) ) ;
#28622 = EDGE_CURVE ( 'NONE', #20947, #1023, #20930, .T. ) ;
#28623 = CARTESIAN_POINT ( 'NONE',  ( 0.000000000000000000, 3.267716535433071279, -0.6692913385826760875 ) ) ;
#28624 = DIRECTION ( 'NONE',  ( 1.000000000000000000, 0.000000000000000000, 0.000000000000000000 ) ) ;
#28625 = EDGE_CURVE ( 'NONE', #514, #10053, #1569, .T. ) ;
#28626 = LINE ( 'NONE', #44372, #17700 ) ;
#28627 = CARTESIAN_POINT ( 'NONE',  ( 0.3136974817028395091, 1.508467219206862664, -2.936457595020219635 ) ) ;
#28628 = VERTEX_POINT ( 'NONE', #33078 ) ;
#28629 = EDGE_CURVE ( 'NONE', #32984, #8503, #12938, .T. ) ;
#28630 = CARTESIAN_POINT ( 'NONE',  ( 1.722315188380549422, 1.647628733693584868, -2.398471789188510783 ) ) ;
#28631 = CARTESIAN_POINT ( 'NONE',  ( -2.889674983507169337, 1.575089141731351505, -0.6090712660038034576 ) ) ;
#28632 = EDGE_LOOP ( 'NONE', ( #22055, #42002, #42641, #11769 ) ) ;
#28633 = CARTESIAN_POINT ( 'NONE',  ( -0.04921259842519689481, 6.692913385826772199, 2.213182383082911375 ) ) ;
#28634 = VECTOR ( 'NONE', #22644, 39.37007874015748143 ) ;
#28635 = EDGE_LOOP ( 'NONE', ( #15878, #40135, #18237, #26545 ) ) ;
#28636 = DIRECTION ( 'NONE',  ( 1.000000000000000000, 0.000000000000000000, 0.000000000000000000 ) ) ;
#28637 = PLANE ( 'NONE',  #14049 ) ;
#28638 = EDGE_CURVE ( 'NONE', #14307, #26807, #28669, .T. ) ;
#28639 = CARTESIAN_POINT ( 'NONE',  ( -1.446240454009885879, 0.003210851617283033092, -1.013622345577424699 ) ) ;
#28640 = ORIENTED_EDGE ( 'NONE', *, *, #23382, .F. ) ;
#28641 = VERTEX_POINT ( 'NONE', #41075 ) ;
#28642 = DIRECTION ( 'NONE',  ( -1.000000000000000000, -0.000000000000000000, -0.000000000000000000 ) ) ;
#28643 = CARTESIAN_POINT ( 'NONE',  ( -2.182111253630085290, 0.000000000000000000, -0.1968503937007880511 ) ) ;
#28644 = DIRECTION ( 'NONE',  ( -1.000000000000000000, 0.000000000000000000, 1.734723475976806848E-16 ) ) ;
#28645 = ADVANCED_FACE ( 'NONE', ( #47738 ), #13443, .F. ) ;
#28646 = DIRECTION ( 'NONE',  ( 0.000000000000000000, 0.000000000000000000, -1.000000000000000000 ) ) ;
#28647 = CARTESIAN_POINT ( 'NONE',  ( 0.5455278134075216556, 3.346456692913386100, 2.095509194042718626 ) ) ;
#28648 = VECTOR ( 'NONE', #38508, 39.37007874015748143 ) ;
#28649 = VECTOR ( 'NONE', #49029, 39.37007874015748143 ) ;
#28650 = ORIENTED_EDGE ( 'NONE', *, *, #32831, .T. ) ;
#28651 = EDGE_CURVE ( 'NONE', #22611, #44092, #37202, .T. ) ;
#28652 = EDGE_CURVE ( 'NONE', #44838, #40529, #28407, .T. ) ;
#28653 = LINE ( 'NONE', #24013, #19140 ) ;
#28654 = EDGE_CURVE ( 'NONE', #924, #7692, #43890, .T. ) ;
#28655 = ADVANCED_FACE ( 'NONE', ( #20412 ), #15111, .F. ) ;
#28656 = VERTEX_POINT ( 'NONE', #41830 ) ;
#28657 = ORIENTED_EDGE ( 'NONE', *, *, #12467, .T. ) ;
#28658 = VECTOR ( 'NONE', #30446, 39.37007874015748143 ) ;
#28659 = EDGE_LOOP ( 'NONE', ( #40576, #41967, #42885, #44 ) ) ;
#28660 = CARTESIAN_POINT ( 'NONE',  ( 1.834499544866850851, 1.737284818394516206, 1.400019292979238772 ) ) ;
#28661 = DIRECTION ( 'NONE',  ( 0.000000000000000000, 1.000000000000000000, 0.000000000000000000 ) ) ;
#28662 = CARTESIAN_POINT ( 'NONE',  ( -2.258024766633058622, 0.000000000000000000, -0.1574803149606298636 ) ) ;
#28663 = CARTESIAN_POINT ( 'NONE',  ( -0.5455278134075208785, 0.000000000000000000, 0.4330708661417290162 ) ) ;
#28664 = VECTOR ( 'NONE', #1686, 39.37007874015748143 ) ;
#28665 = EDGE_LOOP ( 'NONE', ( #9030, #23330, #43403, #32559 ) ) ;
#28666 = ORIENTED_EDGE ( 'NONE', *, *, #24871, .T. ) ;
#28667 = PLANE ( 'NONE',  #32372 ) ;
#28668 = CARTESIAN_POINT ( 'NONE',  ( 2.009930929872536964, 6.692913385826772199, -0.8055662819783819817 ) ) ;
#28669 = LINE ( 'NONE', #40039, #34066 ) ;
#28670 = LINE ( 'NONE', #5948, #33405 ) ;
#28671 = CARTESIAN_POINT ( 'NONE',  ( 0.000000000000000000, 3.267716535433071279, 0.7874015748031454320 ) ) ;
#28672 = CARTESIAN_POINT ( 'NONE',  ( 0.7506868623604561197, 1.205361022782829114E-17, 1.860140722251951484 ) ) ;
#28673 = CARTESIAN_POINT ( 'NONE',  ( -2.182111253630085290, 0.000000000000000000, 0.7480314960629874665 ) ) ;
#28674 = ORIENTED_EDGE ( 'NONE', *, *, #44645, .T. ) ;
#28675 = CARTESIAN_POINT ( 'NONE',  ( 0.08139965876239094178, 1.610780518492231694, 0.000000000000000000 ) ) ;
#28676 = DIRECTION ( 'NONE',  ( -0.9998717552508122886, -0.01601477604151181275, 0.000000000000000000 ) ) ;
#28677 = ORIENTED_EDGE ( 'NONE', *, *, #1917, .F. ) ;
#28678 = ORIENTED_EDGE ( 'NONE', *, *, #28843, .F. ) ;
#28679 = CARTESIAN_POINT ( 'NONE',  ( 0.07982360342473591996, 1.709180471932028711, 0.000000000000000000 ) ) ;
#28680 = CARTESIAN_POINT ( 'NONE',  ( -1.195183497228115035E-16, 0.000000000000000000, -1.259842519685035134 ) ) ;
#28681 = EDGE_CURVE ( 'NONE', #30948, #2778, #2839, .T. ) ;
#28682 = CIRCLE ( 'NONE', #6442, 2.443628662382284489 ) ;
#28683 = ORIENTED_EDGE ( 'NONE', *, *, #47845, .T. ) ;
#28684 = VECTOR ( 'NONE', #10787, 39.37007874015748143 ) ;
#28685 = EDGE_CURVE ( 'NONE', #49753, #7280, #10083, .T. ) ;
#28686 = B_SPLINE_CURVE_WITH_KNOTS ( 'NONE', 3,
 ( #27152, #50348, #39287, #26899 ),
 .UNSPECIFIED., .F., .F.,
 ( 4, 4 ),
 ( 2.329983654547761784E-07, 0.002500456612749824697 ),
 .UNSPECIFIED. ) ;
#28687 = ORIENTED_EDGE ( 'NONE', *, *, #29760, .T. ) ;
#28688 = LINE ( 'NONE', #10353, #2325 ) ;
#28689 = AXIS2_PLACEMENT_3D ( 'NONE', #28458, #1098, #28719 ) ;
#28690 = ORIENTED_EDGE ( 'NONE', *, *, #10614, .T. ) ;
#28691 = ORIENTED_EDGE ( 'NONE', *, *, #13652, .F. ) ;
#28692 = VECTOR ( 'NONE', #37732, 39.37007874015748143 ) ;
#28693 = CARTESIAN_POINT ( 'NONE',  ( 0.4465877632310379930, 0.5234978637819114322, 2.185288426772703296 ) ) ;
#28694 = DIRECTION ( 'NONE',  ( 0.000000000000000000, 0.000000000000000000, -1.000000000000000000 ) ) ;
#28695 = AXIS2_PLACEMENT_3D ( 'NONE', #26811, #42309, #3324 ) ;
#28696 = EDGE_LOOP ( 'NONE', ( #1109, #16651, #19660, #40786 ) ) ;
#28697 = VERTEX_POINT ( 'NONE', #30465 ) ;
#28698 = ORIENTED_EDGE ( 'NONE', *, *, #4163, .F. ) ;
#28699 = LINE ( 'NONE', #17098, #31272 ) ;
#28700 = ORIENTED_EDGE ( 'NONE', *, *, #3984, .F. ) ;
#28701 = ORIENTED_EDGE ( 'NONE', *, *, #41668, .T. ) ;
#28702 = LINE ( 'NONE', #24071, #33105 ) ;
#28703 = LINE ( 'NONE', #21477, #8764 ) ;
#28704 = LINE ( 'NONE', #44452, #29415 ) ;
#28705 = ADVANCED_FACE ( 'NONE', ( #5947 ), #37717, .F. ) ;
#28706 = ORIENTED_EDGE ( 'NONE', *, *, #14831, .T. ) ;
#28707 = EDGE_CURVE ( 'NONE', #17115, #11080, #13955, .T. ) ;
#28708 = B_SPLINE_CURVE_WITH_KNOTS ( 'NONE', 3,
 ( #26506, #11020, #26759, #19263 ),
 .UNSPECIFIED., .F., .F.,
 ( 4, 4 ),
 ( 2.558209911251601479E-07, 0.002500373748775632822 ),
 .UNSPECIFIED. ) ;
#28709 = DIRECTION ( 'NONE',  ( -0.000000000000000000, 1.000000000000000000, -0.000000000000000000 ) ) ;
#28710 = CARTESIAN_POINT ( 'NONE',  ( 0.000000000000000000, 1.574803149606302854, 0.000000000000000000 ) ) ;
#28711 = LINE ( 'NONE', #28448, #23675 ) ;
#28712 = VERTEX_POINT ( 'NONE', #45163 ) ;
#28713 = DIRECTION ( 'NONE',  ( 1.000000000000000000, 0.000000000000000000, 0.000000000000000000 ) ) ;
#28714 = CARTESIAN_POINT ( 'NONE',  ( 1.695772546416037363, 1.477242674555747426, -2.417756147381349141 ) ) ;
#28715 = EDGE_CURVE ( 'NONE', #6874, #16346, #42320, .T. ) ;
#28716 = CARTESIAN_POINT ( 'NONE',  ( 0.000000000000000000, 3.267716535433071279, 0.000000000000000000 ) ) ;
#28717 = ORIENTED_EDGE ( 'NONE', *, *, #7097, .T. ) ;
#28718 = ORIENTED_EDGE ( 'NONE', *, *, #29274, .T. ) ;
#28719 = DIRECTION ( 'NONE',  ( 1.000000000000000000, 0.000000000000000000, 0.000000000000000000 ) ) ;
#28720 = DIRECTION ( 'NONE',  ( -0.000000000000000000, 1.000000000000000000, -0.000000000000000000 ) ) ;
#28721 = DIRECTION ( 'NONE',  ( -0.01601477604151182663, 0.9998717552508123996, -0.000000000000000000 ) ) ;
#28722 = AXIS2_PLACEMENT_3D ( 'NONE', #20438, #37163, #24317 ) ;
#28723 = DIRECTION ( 'NONE',  ( 0.8805955318567321166, 0.000000000000000000, 0.4738686624730094055 ) ) ;
#28724 = FACE_OUTER_BOUND ( 'NONE', #15280, .T. ) ;
#28725 = VERTEX_POINT ( 'NONE', #9828 ) ;
#28726 = ORIENTED_EDGE ( 'NONE', *, *, #28998, .F. ) ;
#28727 = CARTESIAN_POINT ( 'NONE',  ( 0.08119777152254364916, 1.623385212329073957, 0.000000000000000000 ) ) ;
#28728 = VECTOR ( 'NONE', #32104, 39.37007874015748143 ) ;
#28729 = ORIENTED_EDGE ( 'NONE', *, *, #48524, .T. ) ;
#28730 = DIRECTION ( 'NONE',  ( 1.558091277195270436E-17, -1.000000000000000000, -1.150229170499806500E-16 ) ) ;
#28731 = DIRECTION ( 'NONE',  ( -0.000000000000000000, 1.000000000000000000, -0.000000000000000000 ) ) ;
#28732 = VECTOR ( 'NONE', #3761, 39.37007874015748143 ) ;
#28733 = AXIS2_PLACEMENT_3D ( 'NONE', #3871, #19600, #15491 ) ;
#28734 = VECTOR ( 'NONE', #37895, 39.37007874015748143 ) ;
#28735 = PLANE ( 'NONE',  #27478 ) ;
#28736 = CARTESIAN_POINT ( 'NONE',  ( 2.867773316779195447, 1.205361022782829114E-17, -0.7050287376752006896 ) ) ;
#28737 = LINE ( 'NONE', #12482, #8028 ) ;
#28738 = ORIENTED_EDGE ( 'NONE', *, *, #29046, .F. ) ;
#28739 = CARTESIAN_POINT ( 'NONE',  ( -1.024442997624234601E-17, 3.267716535433071279, 1.777125317778812071E-33 ) ) ;
#28740 = CONICAL_SURFACE ( 'NONE', #21353, 3.033577403570480779, 1.554780866114618743 ) ;
#28741 = PLANE ( 'NONE',  #49582 ) ;
#28742 = ORIENTED_EDGE ( 'NONE', *, *, #15486, .F. ) ;
#28743 = LINE ( 'NONE', #36505, #10870 ) ;
#28744 = VECTOR ( 'NONE', #17004, 39.37007874015748143 ) ;
#28745 = PLANE ( 'NONE',  #23676 ) ;
#28746 = CARTESIAN_POINT ( 'NONE',  ( -1.636583440222563635, 3.346456692913386100, -4.780733988912460139E-16 ) ) ;
#28747 = ORIENTED_EDGE ( 'NONE', *, *, #1593, .F. ) ;
#28748 = DIRECTION ( 'NONE',  ( 1.000000000000000000, 0.000000000000000000, 0.000000000000000000 ) ) ;
#28749 = CARTESIAN_POINT ( 'NONE',  ( -0.2727639067037608278, 0.000000000000000000, -1.299212598425193210 ) ) ;
#28750 = EDGE_CURVE ( 'NONE', #29680, #46268, #45416, .T. ) ;
#28751 = EDGE_CURVE ( 'NONE', #49645, #43429, #22712, .T. ) ;
#28752 = VERTEX_POINT ( 'NONE', #6209 ) ;
#28753 = CARTESIAN_POINT ( 'NONE',  ( 0.4696143004045479352, 0.000000000000000000, -1.417322834645664331 ) ) ;
#28754 = DIRECTION ( 'NONE',  ( 1.000000000000000000, -0.000000000000000000, 0.000000000000000000 ) ) ;
#28755 = ORIENTED_EDGE ( 'NONE', *, *, #32672, .F. ) ;
#28756 = LINE ( 'NONE', #33164, #17976 ) ;
#28757 = EDGE_CURVE ( 'NONE', #27988, #9844, #6713, .T. ) ;
#28758 = DIRECTION ( 'NONE',  ( -0.000000000000000000, 1.000000000000000000, -0.000000000000000000 ) ) ;
#28759 = LINE ( 'NONE', #49105, #30485 ) ;
#28760 = DIRECTION ( 'NONE',  ( 1.734723475976806848E-16, 0.000000000000000000, 1.000000000000000000 ) ) ;
#28761 = VECTOR ( 'NONE', #43483, 39.37007874015748143 ) ;
#28762 = EDGE_CURVE ( 'NONE', #35037, #50954, #25565, .T. ) ;
#28763 = CARTESIAN_POINT ( 'NONE',  ( -1.312442655063644770, 0.006898494447474761912, -1.186737126055851022 ) ) ;
#28764 = ORIENTED_EDGE ( 'NONE', *, *, #40056, .F. ) ;
#28765 = ORIENTED_EDGE ( 'NONE', *, *, #24871, .F. ) ;
#28766 = CARTESIAN_POINT ( 'NONE',  ( 0.1968503937007872462, 3.346456692913386100, -0.5118110236220465570 ) ) ;
#28767 = DIRECTION ( 'NONE',  ( 1.734723475976806848E-16, -0.000000000000000000, 1.000000000000000000 ) ) ;
#28768 = ORIENTED_EDGE ( 'NONE', *, *, #14983, .F. ) ;
#28769 = DIRECTION ( 'NONE',  ( -1.000000000000000000, 0.000000000000000000, -0.000000000000000000 ) ) ;
#28770 = CARTESIAN_POINT ( 'NONE',  ( 2.122091976112993272, 5.905511811023623991, 0.4338754535133124146 ) ) ;
#28771 = CARTESIAN_POINT ( 'NONE',  ( -1.712496953225537188, 3.346456692913386100, 0.7874015748031456541 ) ) ;
#28772 = PLANE ( 'NONE',  #31437 ) ;
#28773 = VECTOR ( 'NONE', #8841, 39.37007874015748143 ) ;
#28774 = AXIS2_PLACEMENT_3D ( 'NONE', #40864, #21242, #12222 ) ;
#28775 = EDGE_LOOP ( 'NONE', ( #20570, #48153, #40262, #16048 ) ) ;
#28776 = EDGE_LOOP ( 'NONE', ( #24833, #23680, #41675, #37227 ) ) ;
#28777 = EDGE_CURVE ( 'NONE', #24413, #32550, #25822, .T. ) ;
#28778 = ADVANCED_FACE ( 'NONE', ( #18333 ), #1818, .F. ) ;
#28779 = LINE ( 'NONE', #13298, #18019 ) ;
#28780 = DIRECTION ( 'NONE',  ( 0.9989930665413151445, 0.000000000000000000, -0.04486483035050446017 ) ) ;
#28781 = CARTESIAN_POINT ( 'NONE',  ( 1.091055626815042645, 3.267716535433071279, -1.892679809432644882E-16 ) ) ;
#28782 = VERTEX_POINT ( 'NONE', #49018 ) ;
#28783 = AXIS2_PLACEMENT_3D ( 'NONE', #13316, #50086, #29048 ) ;
#28784 = DIRECTION ( 'NONE',  ( -0.000000000000000000, 1.000000000000000000, -0.000000000000000000 ) ) ;
#28785 = FACE_BOUND ( 'NONE', #37722, .T. ) ;
#28786 = ORIENTED_EDGE ( 'NONE', *, *, #7381, .T. ) ;
#28787 = EDGE_CURVE ( 'NONE', #38287, #9419, #13701, .T. ) ;
#28788 = CARTESIAN_POINT ( 'NONE',  ( 2.083268748869757658, 3.346456692913386100, 0.5905511811023582691 ) ) ;
#28789 = ORIENTED_EDGE ( 'NONE', *, *, #49403, .T. ) ;
#28790 = ORIENTED_EDGE ( 'NONE', *, *, #10551, .T. ) ;
#28791 = VECTOR ( 'NONE', #37342, 39.37007874015748143 ) ;
#28792 = LINE ( 'NONE', #39644, #22583 ) ;
#28793 = EDGE_LOOP ( 'NONE', ( #23607, #2452, #17281, #31099 ) ) ;
#28794 = CARTESIAN_POINT ( 'NONE',  ( -0.6214413264104945434, 0.000000000000000000, -2.244094488188968395 ) ) ;
#28795 = EDGE_LOOP ( 'NONE', ( #30314, #49737, #16663, #10830 ) ) ;
#28796 = DIMENSIONAL_EXPONENTS ( 1.000000000000000000, 0.000000000000000000, 0.000000000000000000, 0.000000000000000000, 0.000000000000000000, 0.000000000000000000, 0.000000000000000000 ) ;
#28797 = DIRECTION ( 'NONE',  ( 1.734723475976806848E-16, 0.000000000000000000, 1.000000000000000000 ) ) ;
#28798 = EDGE_CURVE ( 'NONE', #187, #14069, #38219, .T. ) ;
#28799 = LINE ( 'NONE', #14074, #8798 ) ;
#28800 = LINE ( 'NONE', #28029, #1989 ) ;
#28801 = AXIS2_PLACEMENT_3D ( 'NONE', #48792, #13223, #13473 ) ;
#28802 = CARTESIAN_POINT ( 'NONE',  ( -1.037524086854360483, 0.000000000000000000, 2.764473043227569260 ) ) ;
#28803 = FACE_OUTER_BOUND ( 'NONE', #36439, .T. ) ;
#28804 = DIRECTION ( 'NONE',  ( -0.000000000000000000, 1.000000000000000000, -0.000000000000000000 ) ) ;
#28805 = B_SPLINE_CURVE_WITH_KNOTS ( 'NONE', 3,
 ( #39945, #31433, #35312, #39688 ),
 .UNSPECIFIED., .F., .F.,
 ( 4, 4 ),
 ( 0.0009642369134306138503, 0.004861909058386497222 ),
 .UNSPECIFIED. ) ;
#28806 = EDGE_LOOP ( 'NONE', ( #22945, #51052, #38494, #46408 ) ) ;
#28807 = FACE_OUTER_BOUND ( 'NONE', #35562, .T. ) ;
#28808 = CARTESIAN_POINT ( 'NONE',  ( 0.5455278134075208785, 0.000000000000000000, -1.889763779527552812 ) ) ;
#28809 = CIRCLE ( 'NONE', #37081, 2.443628662382284489 ) ;
#28810 = ORIENTED_EDGE ( 'NONE', *, *, #33851, .T. ) ;
#28811 = DIRECTION ( 'NONE',  ( -0.000000000000000000, 1.000000000000000000, -0.000000000000000000 ) ) ;
#28812 = FACE_OUTER_BOUND ( 'NONE', #7015, .T. ) ;
#28813 = ORIENTED_EDGE ( 'NONE', *, *, #18206, .F. ) ;
#28814 = CARTESIAN_POINT ( 'NONE',  ( 0.000000000000000000, 3.267716535433071279, 0.000000000000000000 ) ) ;
#28815 = CARTESIAN_POINT ( 'NONE',  ( 1.833433833923351353, 3.346456692913386100, 1.259842519685033135 ) ) ;
#28816 = CIRCLE ( 'NONE', #3240, 2.244934639244525076 ) ;
#28817 = DIRECTION ( 'NONE',  ( -1.000000000000000000, 0.000000000000000000, -0.000000000000000000 ) ) ;
#28818 = EDGE_CURVE ( 'NONE', #30940, #8556, #37964, .T. ) ;
#28819 = ORIENTED_EDGE ( 'NONE', *, *, #46890, .F. ) ;
#28820 = DIRECTION ( 'NONE',  ( -3.469446951953613696E-16, 0.000000000000000000, -1.000000000000000000 ) ) ;
#28821 = AXIS2_PLACEMENT_3D ( 'NONE', #6554, #38551, #14802 ) ;
#28822 = VERTEX_POINT ( 'NONE', #10333 ) ;
#28823 = FACE_BOUND ( 'NONE', #42404, .T. ) ;
#28824 = EDGE_CURVE ( 'NONE', #23728, #28782, #22461, .T. ) ;
#28825 = CARTESIAN_POINT ( 'NONE',  ( 1.560669927219590303, 0.000000000000000000, -1.102362204724405714 ) ) ;
#28826 = CARTESIAN_POINT ( 'NONE',  ( 1.930249146414562578, 0.05883613814988478824, 0.3111320644955062886 ) ) ;
#28828 = EDGE_CURVE ( 'NONE', #2040, #47582, #42306, .T. ) ;
#28827 = LINE ( 'NONE', #29078, #28480 ) ;
#28829 = EDGE_CURVE ( 'NONE', #1905, #1056, #18594, .T. ) ;
#28830 = ORIENTED_EDGE ( 'NONE', *, *, #13039, .T. ) ;
#28831 = ORIENTED_EDGE ( 'NONE', *, *, #25476, .F. ) ;
#28832 = CARTESIAN_POINT ( 'NONE',  ( -0.6214413264104945434, 3.267716535433071279, 2.156057715732901026E-16 ) ) ;
#28833 = ORIENTED_EDGE ( 'NONE', *, *, #8952, .T. ) ;
#28834 = CARTESIAN_POINT ( 'NONE',  ( -1.712496953225537188, 3.267716535433071279, 1.102362204724404160 ) ) ;
#28835 = EDGE_LOOP ( 'NONE', ( #31, #28363, #39334, #21101 ) ) ;
#28836 = FACE_OUTER_BOUND ( 'NONE', #50848, .T. ) ;
#28837 = EDGE_CURVE ( 'NONE', #16144, #5349, #27326, .T. ) ;
#28838 = VECTOR ( 'NONE', #32536, 39.37007874015748143 ) ;
#28839 = EDGE_LOOP ( 'NONE', ( #18804, #27796, #15800, #2750 ) ) ;
#28840 = CARTESIAN_POINT ( 'NONE',  ( 0.000000000000000000, 1.574803149606302854, 0.000000000000000000 ) ) ;
#28841 = DIRECTION ( 'NONE',  ( 0.9639628606958549062, 3.084137967884539202E-17, -0.2660368455666687892 ) ) ;
#28842 = VERTEX_POINT ( 'NONE', #11590 ) ;
#28843 = EDGE_CURVE ( 'NONE', #4283, #15792, #43583, .T. ) ;
#28844 = CARTESIAN_POINT ( 'NONE',  ( -2.258024766633058622, 0.000000000000000000, -0.03937007874015881204 ) ) ;
#28845 = ORIENTED_EDGE ( 'NONE', *, *, #29220, .T. ) ;
#28846 = VERTEX_POINT ( 'NONE', #39212 ) ;
#28847 = CONICAL_SURFACE ( 'NONE', #49443, 2.244934639244524632, 1.554780866114618743 ) ;
#28848 = EDGE_CURVE ( 'NONE', #17243, #24661, #12104, .T. ) ;
#28849 = ORIENTED_EDGE ( 'NONE', *, *, #30997, .F. ) ;
#28850 = ORIENTED_EDGE ( 'NONE', *, *, #42960, .F. ) ;
#28851 = CARTESIAN_POINT ( 'NONE',  ( -1.483604961240789555, 5.905511811023623991, 1.623324365321667129 ) ) ;
#28852 = VERTEX_POINT ( 'NONE', #35601 ) ;
#28853 = CIRCLE ( 'NONE', #1664, 2.165354330708661568 ) ;
#28854 = CARTESIAN_POINT ( 'NONE',  ( -0.8182917201112819283, 3.346456692913386100, 2.047244094488179567 ) ) ;
#28855 = EDGE_CURVE ( 'NONE', #16985, #8210, #7206, .T. ) ;
#28856 = EDGE_LOOP ( 'NONE', ( #21941, #30298, #3363, #32102 ) ) ;
#28857 = DIRECTION ( 'NONE',  ( 1.000000000000000000, 0.000000000000000000, 0.000000000000000000 ) ) ;
#28858 = CARTESIAN_POINT ( 'NONE',  ( 1.090138530625468061, 5.905511811023623991, 1.920534397867777798 ) ) ;
#28859 = ORIENTED_EDGE ( 'NONE', *, *, #40590, .F. ) ;
#28860 = LINE ( 'NONE', #44592, #48338 ) ;
#28861 = CARTESIAN_POINT ( 'NONE',  ( 1.909347346926324684, 3.346456692913386100, -0.4724409448818889246 ) ) ;
#28862 = LINE ( 'NONE', #3655, #32411 ) ;
#28863 = DIRECTION ( 'NONE',  ( -0.000000000000000000, 1.000000000000000000, -0.000000000000000000 ) ) ;
#28864 = EDGE_CURVE ( 'NONE', #41853, #48369, #48055, .T. ) ;
#28865 = CARTESIAN_POINT ( 'NONE',  ( 0.5455278134075212115, 3.346456692913386100, 0.3149606299212576177 ) ) ;
#28866 = EDGE_CURVE ( 'NONE', #9684, #17906, #38470, .T. ) ;
#28867 = CARTESIAN_POINT ( 'NONE',  ( -1.439733046521777027, 3.346456692913386100, -1.141732283464563791 ) ) ;
#28868 = CARTESIAN_POINT ( 'NONE',  ( -1.363819533518803029, 0.000000000000000000, 0.7874015748031456541 ) ) ;
#28869 = ORIENTED_EDGE ( 'NONE', *, *, #19309, .F. ) ;
#28870 = DIRECTION ( 'NONE',  ( -0.000000000000000000, -0.000000000000000000, 1.000000000000000000 ) ) ;
#28871 = CARTESIAN_POINT ( 'NONE',  ( 0.3530705266098149164, -0.6299212598425202314, -0.1234057657284599735 ) ) ;
#28872 = ORIENTED_EDGE ( 'NONE', *, *, #9592, .F. ) ;
#28873 = CARTESIAN_POINT ( 'NONE',  ( 1.556712866041120247, 1.480457248723645591, 2.509548638715870084 ) ) ;
#28874 = ORIENTED_EDGE ( 'NONE', *, *, #14205, .F. ) ;
#28875 = DIRECTION ( 'NONE',  ( -0.000000000000000000, 1.000000000000000000, -0.000000000000000000 ) ) ;
#28876 = EDGE_CURVE ( 'NONE', #7253, #41982, #14966, .T. ) ;
#28877 = CARTESIAN_POINT ( 'NONE',  ( 0.000000000000000000, 1.574803149606302854, 0.000000000000000000 ) ) ;
#28878 = VECTOR ( 'NONE', #42759, 39.37007874015748143 ) ;
#28879 = DIRECTION ( 'NONE',  ( -3.469446951953613696E-16, 0.000000000000000000, -1.000000000000000000 ) ) ;
#28880 = VECTOR ( 'NONE', #21752, 39.37007874015748143 ) ;
#28881 = PLANE ( 'NONE',  #35822 ) ;
#28882 = DIRECTION ( 'NONE',  ( 1.000000000000000000, 0.000000000000000000, 0.000000000000000000 ) ) ;
#28883 = EDGE_LOOP ( 'NONE', ( #7276, #561, #18508, #47082 ) ) ;
#28884 = EDGE_CURVE ( 'NONE', #27061, #47061, #34590, .T. ) ;
#28885 = LINE ( 'NONE', #16769, #32407 ) ;
#28886 = DIRECTION ( 'NONE',  ( -3.469446951953613696E-16, 0.000000000000000000, -1.000000000000000000 ) ) ;
#28887 = EDGE_LOOP ( 'NONE', ( #16733, #18427, #47538, #41464 ) ) ;
#28888 = DIRECTION ( 'NONE',  ( 0.000000000000000000, 0.000000000000000000, -1.000000000000000000 ) ) ;
#28889 = VECTOR ( 'NONE', #50246, 39.37007874015748143 ) ;
#28890 = VERTEX_POINT ( 'NONE', #27582 ) ;
#28891 = PLANE ( 'NONE',  #20258 ) ;
#28892 = CARTESIAN_POINT ( 'NONE',  ( -1.636583440222564301, 3.346456692913386100, -1.259842519685034468 ) ) ;
#28893 = DIRECTION ( 'NONE',  ( 0.000000000000000000, 0.000000000000000000, 1.000000000000000000 ) ) ;
#28894 = CARTESIAN_POINT ( 'NONE',  ( -2.014567149787738654, 1.675634971041569443, -0.8075478974698888646 ) ) ;
#28895 = EDGE_LOOP ( 'NONE', ( #3865, #19302, #37819, #47914 ) ) ;
#28896 = ORIENTED_EDGE ( 'NONE', *, *, #10869, .F. ) ;
#28897 = LINE ( 'NONE', #12913, #15284 ) ;
#28898 = CARTESIAN_POINT ( 'NONE',  ( 1.636583440222563857, 3.267716535433071279, 1.574803149606291974 ) ) ;
#28899 = CARTESIAN_POINT ( 'NONE',  ( 2.100227814008711391, 1.205361022782829114E-17, -2.076109931251913565 ) ) ;
#28900 = VERTEX_POINT ( 'NONE', #27077 ) ;
#28901 = DIRECTION ( 'NONE',  ( -0.000000000000000000, 1.000000000000000000, -0.000000000000000000 ) ) ;
#28902 = LINE ( 'NONE', #48996, #24208 ) ;
#28903 = EDGE_CURVE ( 'NONE', #46686, #26290, #33259, .T. ) ;
#28904 = ORIENTED_EDGE ( 'NONE', *, *, #6642, .T. ) ;
#28905 = LINE ( 'NONE', #48494, #29059 ) ;
#28906 = PLANE ( 'NONE',  #8059 ) ;
#28907 = ORIENTED_EDGE ( 'NONE', *, *, #30878, .F. ) ;
#28908 = VERTEX_POINT ( 'NONE', #23206 ) ;
#28909 = ADVANCED_FACE ( 'NONE', ( #7467 ), #11342, .F. ) ;
#28910 = EDGE_LOOP ( 'NONE', ( #31301, #43498, #8015, #4468 ) ) ;
#28911 = DIRECTION ( 'NONE',  ( 1.734723475976806848E-16, -0.000000000000000000, 1.000000000000000000 ) ) ;
#28912 = AXIS2_PLACEMENT_3D ( 'NONE', #23211, #35096, #47171 ) ;
#28913 = CARTESIAN_POINT ( 'NONE',  ( 1.636583440222563857, 3.346456692913386100, -0.3149606299212596716 ) ) ;
#28914 = B_SPLINE_CURVE_WITH_KNOTS ( 'NONE', 3,
 ( #30056, #45771, #26180, #41926 ),
 .UNSPECIFIED., .F., .F.,
 ( 4, 4 ),
 ( 0.02729311668581372446, 0.02847067742387721784 ),
 .UNSPECIFIED. ) ;
#28915 = VECTOR ( 'NONE', #435, 39.37007874015748143 ) ;
#28916 = EDGE_CURVE ( 'NONE', #6701, #25223, #31471, .T. ) ;
#28917 = EDGE_CURVE ( 'NONE', #16822, #16156, #27838, .T. ) ;
#28918 = CARTESIAN_POINT ( 'NONE',  ( 1.287906020515830141, 3.346456692913386100, 0.9448818897637746295 ) ) ;
#28919 = CARTESIAN_POINT ( 'NONE',  ( -0.3937007874015748254, 0.000000000000000000, -0.7480314960629921295 ) ) ;
#28920 = EDGE_LOOP ( 'NONE', ( #5163, #17481, #4322, #39711 ) ) ;
#28921 = ORIENTED_EDGE ( 'NONE', *, *, #11103, .T. ) ;
#28922 = CARTESIAN_POINT ( 'NONE',  ( 1.474379988472116487, 1.633091647787944911, 1.762361831087230213 ) ) ;
#28923 = DIRECTION ( 'NONE',  ( -3.469446951953613696E-16, 0.000000000000000000, -1.000000000000000000 ) ) ;
#28924 = DIRECTION ( 'NONE',  ( -1.000000000000000000, 0.000000000000000000, 1.734723475976806848E-16 ) ) ;
#28925 = ADVANCED_FACE ( 'NONE', ( #15968 ), #50275, .F. ) ;
#28926 = AXIS2_PLACEMENT_3D ( 'NONE', #46337, #3250, #46586 ) ;
#28927 = PLANE ( 'NONE',  #48192 ) ;
#28928 = CARTESIAN_POINT ( 'NONE',  ( 2.112319093887386146, 0.000000000000000000, 0.3357951146312926904 ) ) ;
#28929 = LINE ( 'NONE', #9061, #22662 ) ;
#28930 = DIRECTION ( 'NONE',  ( -0.000000000000000000, 1.000000000000000000, -0.000000000000000000 ) ) ;
#28931 = VERTEX_POINT ( 'NONE', #47168 ) ;
#28932 = CARTESIAN_POINT ( 'NONE',  ( 2.491402175429655141, 5.905511811023623991, -1.585592796919505387 ) ) ;
#28933 = CARTESIAN_POINT ( 'NONE',  ( 2.947574761915768171, 1.447536563168191126, -0.1816379373804911657 ) ) ;
#28934 = VERTEX_POINT ( 'NONE', #7972 ) ;
#28936 = EDGE_LOOP ( 'NONE', ( #46099, #35390, #25926, #4858 ) ) ;
#28935 = EDGE_CURVE ( 'NONE', #29992, #18572, #4109, .T. ) ;
#28937 = CARTESIAN_POINT ( 'NONE',  ( 0.000000000000000000, 3.267716535433071279, 1.850393700787392293 ) ) ;
#28938 = CARTESIAN_POINT ( 'NONE',  ( 1.287906020515830141, 3.267716535433071279, 0.3149606299212578953 ) ) ;
#28939 = ORIENTED_EDGE ( 'NONE', *, *, #45428, .F. ) ;
#28940 = EDGE_CURVE ( 'NONE', #36553, #49693, #3091, .T. ) ;
#28941 = EDGE_CURVE ( 'NONE', #19249, #38642, #14581, .T. ) ;
#28942 = ORIENTED_EDGE ( 'NONE', *, *, #31040, .T. ) ;
#28943 = DIRECTION ( 'NONE',  ( -1.000000000000000000, 0.000000000000000000, 1.734723475976806848E-16 ) ) ;
#28944 = ORIENTED_EDGE ( 'NONE', *, *, #1324, .T. ) ;
#28945 = VECTOR ( 'NONE', #24692, 39.37007874015748143 ) ;
#28946 = DIRECTION ( 'NONE',  ( 1.734723475976806848E-16, -0.000000000000000000, 1.000000000000000000 ) ) ;
#28947 = LINE ( 'NONE', #20954, #35459 ) ;
#28948 = VECTOR ( 'NONE', #4588, 39.37007874015748143 ) ;
#28949 = EDGE_LOOP ( 'NONE', ( #30864, #24541, #47568, #11568, #29196, #13929, #8054, #5357 ) ) ;
#28950 = VERTEX_POINT ( 'NONE', #26827 ) ;
#28951 = ORIENTED_EDGE ( 'NONE', *, *, #38050, .T. ) ;
#28952 = DIRECTION ( 'NONE',  ( 0.000000000000000000, 0.000000000000000000, -1.000000000000000000 ) ) ;
#28953 = ORIENTED_EDGE ( 'NONE', *, *, #3778, .F. ) ;
#28954 = ORIENTED_EDGE ( 'NONE', *, *, #6590, .T. ) ;
#28955 = DIRECTION ( 'NONE',  ( -0.000000000000000000, 0.000000000000000000, 1.000000000000000000 ) ) ;
#28956 = DIRECTION ( 'NONE',  ( 0.000000000000000000, 0.000000000000000000, -1.000000000000000000 ) ) ;
#28957 = AXIS2_PLACEMENT_3D ( 'NONE', #45956, #22747, #42609 ) ;
#28958 = CARTESIAN_POINT ( 'NONE',  ( -1.909347346926324462, 3.346456692913386100, -0.3543307086614171930 ) ) ;
#28959 = VECTOR ( 'NONE', #39156, 39.37007874015748143 ) ;
#28960 = VERTEX_POINT ( 'NONE', #47939 ) ;
#28961 = LINE ( 'NONE', #47784, #45223 ) ;
#28962 = FACE_OUTER_BOUND ( 'NONE', #20948, .T. ) ;
#28963 = CARTESIAN_POINT ( 'NONE',  ( 1.909347346926324684, 3.267716535433071279, 0.5905511811023582691 ) ) ;
#28964 = ORIENTED_EDGE ( 'NONE', *, *, #9062, .F. ) ;
#28965 = CARTESIAN_POINT ( 'NONE',  ( 2.106197740627111514, 0.000000000000000000, -1.102362204724406602 ) ) ;
#28966 = CARTESIAN_POINT ( 'NONE',  ( -2.491402175429632493, 5.905511811023623991, -1.585592796919543579 ) ) ;
#28967 = CARTESIAN_POINT ( 'NONE',  ( -1.091055626815042645, 0.000000000000000000, 1.889763779527550147 ) ) ;
#28968 = ORIENTED_EDGE ( 'NONE', *, *, #14836, .F. ) ;
#28969 = ORIENTED_EDGE ( 'NONE', *, *, #41028, .F. ) ;
#28970 = CARTESIAN_POINT ( 'NONE',  ( -0.8942052331142547050, 3.267716535433071279, 0.7480314960629874665 ) ) ;
#28971 = LINE ( 'NONE', #44709, #25571 ) ;
#28972 = EDGE_CURVE ( 'NONE', #28465, #1977, #27538, .T. ) ;
#28973 = EDGE_CURVE ( 'NONE', #16862, #26872, #1248, .T. ) ;
#28974 = DIRECTION ( 'NONE',  ( -0.000000000000000000, 1.000000000000000000, -0.000000000000000000 ) ) ;
#28975 = FACE_OUTER_BOUND ( 'NONE', #44170, .T. ) ;
#28976 = VERTEX_POINT ( 'NONE', #482 ) ;
#28978 = EDGE_CURVE ( 'NONE', #46962, #4005, #48697, .T. ) ;
#28977 = ORIENTED_EDGE ( 'NONE', *, *, #16728, .F. ) ;
#28979 = CARTESIAN_POINT ( 'NONE',  ( -0.6214413264104945434, 3.346456692913386100, -0.7874015748031467643 ) ) ;
#28980 = ORIENTED_EDGE ( 'NONE', *, *, #23337, .F. ) ;
#28981 = CARTESIAN_POINT ( 'NONE',  ( 1.833433833923351353, 0.000000000000000000, -0.3149606299212596716 ) ) ;
#28982 = DIRECTION ( 'NONE',  ( -1.000000000000000000, 0.000000000000000000, -0.000000000000000000 ) ) ;
#28983 = VECTOR ( 'NONE', #15157, 39.37007874015748143 ) ;
#28984 = VECTOR ( 'NONE', #19750, 39.37007874015748143 ) ;
#28985 = LINE ( 'NONE', #6009, #6890 ) ;
#28986 = CARTESIAN_POINT ( 'NONE',  ( -1.547114303032252502, 1.584696887024839906, -1.547279266820049237 ) ) ;
#28988 = DIRECTION ( 'NONE',  ( -0.000000000000000000, 1.000000000000000000, -0.000000000000000000 ) ) ;
#28987 = VECTOR ( 'NONE', #9668, 39.37007874015748143 ) ;
#28989 = ORIENTED_EDGE ( 'NONE', *, *, #42091, .T. ) ;
#28990 = DIRECTION ( 'NONE',  ( -0.000000000000000000, 1.000000000000000000, -0.000000000000000000 ) ) ;
#28991 = VECTOR ( 'NONE', #27052, 39.37007874015748854 ) ;
#28992 = EDGE_CURVE ( 'NONE', #50367, #30196, #8487, .T. ) ;
#28993 = B_SPLINE_CURVE_WITH_KNOTS ( 'NONE', 3,
 ( #28660, #24537, #12658, #28398 ),
 .UNSPECIFIED., .F., .F.,
 ( 4, 4 ),
 ( 0.01434375831065246368, 0.03074838983875128814 ),
 .UNSPECIFIED. ) ;
#28994 = DIRECTION ( 'NONE',  ( -0.000000000000000000, 1.000000000000000000, -0.000000000000000000 ) ) ;
#28995 = ORIENTED_EDGE ( 'NONE', *, *, #49941, .F. ) ;
#28996 = AXIS2_PLACEMENT_3D ( 'NONE', #23034, #22283, #26399 ) ;
#28997 = CARTESIAN_POINT ( 'NONE',  ( 1.244991204790707684, 3.346456692913386100, -1.771653543307081691 ) ) ;
#28998 = EDGE_CURVE ( 'NONE', #42546, #33385, #4612, .T. ) ;
#28999 = DIRECTION ( 'NONE',  ( 1.734723475976806848E-16, 0.000000000000000000, 1.000000000000000000 ) ) ;
#29000 = DIRECTION ( 'NONE',  ( -3.469446951953613696E-16, 0.000000000000000000, -1.000000000000000000 ) ) ;
#29001 = ORIENTED_EDGE ( 'NONE', *, *, #13617, .F. ) ;
#29002 = DIRECTION ( 'NONE',  ( -3.469446951953613696E-16, 0.000000000000000000, -1.000000000000000000 ) ) ;
#29003 = ADVANCED_FACE ( 'NONE', ( #48194 ), #8998, .F. ) ;
#29004 = DIRECTION ( 'NONE',  ( 1.000000000000000000, -0.000000000000000000, 0.000000000000000000 ) ) ;
#29005 = EDGE_CURVE ( 'NONE', #48104, #4710, #44595, .T. ) ;
#29006 = ORIENTED_EDGE ( 'NONE', *, *, #17752, .F. ) ;
#29007 = CARTESIAN_POINT ( 'NONE',  ( 0.000000000000000000, 3.267716535433071279, -1.889763779527552146 ) ) ;
#29008 = CARTESIAN_POINT ( 'NONE',  ( 0.04921259842519675604, 1.049866565067837820, 2.024102349885854135 ) ) ;
#29009 = VERTEX_POINT ( 'NONE', #4360 ) ;
#29010 = EDGE_CURVE ( 'NONE', #7441, #6293, #24238, .T. ) ;
#29011 = DIRECTION ( 'NONE',  ( 0.000000000000000000, 0.000000000000000000, -1.000000000000000000 ) ) ;
#29012 = DIRECTION ( 'NONE',  ( -3.469446951953613696E-16, 0.000000000000000000, -1.000000000000000000 ) ) ;
#29013 = PLANE ( 'NONE',  #34578 ) ;
#29014 = LINE ( 'NONE', #43991, #46591 ) ;
#29015 = DIRECTION ( 'NONE',  ( 1.734723475976806848E-16, -0.000000000000000000, 1.000000000000000000 ) ) ;
#29016 = EDGE_LOOP ( 'NONE', ( #9498, #34537, #13006, #477 ) ) ;
#29017 = ORIENTED_EDGE ( 'NONE', *, *, #26557, .F. ) ;
#29018 = LINE ( 'NONE', #29792, #43797 ) ;
#29019 = DIRECTION ( 'NONE',  ( -3.469446951953613696E-16, 0.000000000000000000, -1.000000000000000000 ) ) ;
#29020 = ORIENTED_EDGE ( 'NONE', *, *, #29830, .T. ) ;
#29021 = DIRECTION ( 'NONE',  ( 0.000000000000000000, 0.000000000000000000, -1.000000000000000000 ) ) ;
#29022 = LINE ( 'NONE', #21036, #7951 ) ;
#29023 = LINE ( 'NONE', #901, #45857 ) ;
#29024 = CARTESIAN_POINT ( 'NONE',  ( 1.387661672111481836, 0.000000000000000000, -1.663104731517921930 ) ) ;
#29025 = ORIENTED_EDGE ( 'NONE', *, *, #50395, .T. ) ;
#29026 = AXIS2_PLACEMENT_3D ( 'NONE', #1862, #38008, #22255 ) ;
#29027 = ORIENTED_EDGE ( 'NONE', *, *, #47374, .T. ) ;
#29028 = DIRECTION ( 'NONE',  ( 0.000000000000000000, 0.000000000000000000, -1.000000000000000000 ) ) ;
#29029 = DIRECTION ( 'NONE',  ( 0.000000000000000000, -1.000000000000000000, 0.000000000000000000 ) ) ;
#29030 = DIRECTION ( 'NONE',  ( -1.000000000000000000, 0.000000000000000000, 0.000000000000000000 ) ) ;
#29031 = EDGE_LOOP ( 'NONE', ( #40654, #7451, #28786, #40071 ) ) ;
#29032 = FACE_OUTER_BOUND ( 'NONE', #33830, .T. ) ;
#29033 = AXIS2_PLACEMENT_3D ( 'NONE', #31191, #30681, #46893 ) ;
#29034 = FACE_BOUND ( 'NONE', #45586, .T. ) ;
#29035 = ORIENTED_EDGE ( 'NONE', *, *, #15053, .F. ) ;
#29036 = CARTESIAN_POINT ( 'NONE',  ( 0.07982360342473591996, 1.709180471932028711, 0.000000000000000000 ) ) ;
#29037 = ORIENTED_EDGE ( 'NONE', *, *, #4623, .F. ) ;
#29038 = AXIS2_PLACEMENT_3D ( 'NONE', #30065, #17937, #38329 ) ;
#29039 = EDGE_LOOP ( 'NONE', ( #15614, #50378, #21555, #14711 ) ) ;
#29040 = CARTESIAN_POINT ( 'NONE',  ( -1.258178306623050746, 0.002647435328324944988, -1.271028168397900338 ) ) ;
#29041 = VECTOR ( 'NONE', #44673, 39.37007874015748143 ) ;
#29042 = ORIENTED_EDGE ( 'NONE', *, *, #4548, .F. ) ;
#29043 = CARTESIAN_POINT ( 'NONE',  ( -0.3382312733057311060, 1.205361022782829114E-17, -2.139420919314970693 ) ) ;
#29044 = CARTESIAN_POINT ( 'NONE',  ( 0.6507993007407579800, 1.619900495825837838, -2.173134161263437392 ) ) ;
#29045 = ORIENTED_EDGE ( 'NONE', *, *, #39645, .T. ) ;
#29046 = EDGE_CURVE ( 'NONE', #8962, #19997, #39724, .T. ) ;
#29047 = ADVANCED_FACE ( 'NONE', ( #39980 ), #9251, .F. ) ;
#29048 = DIRECTION ( 'NONE',  ( -0.9998717552508121775, -0.01601477604151182663, 0.000000000000000000 ) ) ;
#29049 = FACE_OUTER_BOUND ( 'NONE', #13608, .T. ) ;
#29050 = EDGE_CURVE ( 'NONE', #35680, #38409, #35852, .T. ) ;
#29051 = CARTESIAN_POINT ( 'NONE',  ( -1.317187389162816080, 0.004599037771469988850, -1.191273556348049434 ) ) ;
#29052 = CARTESIAN_POINT ( 'NONE',  ( -1.909347346926324906, 3.267716535433071279, -1.299212598425193210 ) ) ;
#29053 = CARTESIAN_POINT ( 'NONE',  ( -0.04921259842519706829, 1.516406576848131849, 2.952755905511811108 ) ) ;
#29054 = DIRECTION ( 'NONE',  ( -0.9998717552508121775, -0.01601477604151182316, 0.000000000000000000 ) ) ;
#29055 = ORIENTED_EDGE ( 'NONE', *, *, #13614, .T. ) ;
#29056 = CARTESIAN_POINT ( 'NONE',  ( -1.325491792074585451, 1.543512378121542961, -2.638988599164751925 ) ) ;
#29057 = FACE_OUTER_BOUND ( 'NONE', #28793, .T. ) ;
#29058 = ORIENTED_EDGE ( 'NONE', *, *, #5967, .T. ) ;
#29059 = VECTOR ( 'NONE', #44642, 39.37007874015748143 ) ;
#29060 = DIRECTION ( 'NONE',  ( -1.000000000000000000, 0.000000000000000000, 1.734723475976806848E-16 ) ) ;
#29061 = EDGE_CURVE ( 'NONE', #22430, #22117, #31990, .T. ) ;
#29062 = CARTESIAN_POINT ( 'NONE',  ( -0.3499216181689347449, 1.669488919521048276, 2.203840029116182375 ) ) ;
#29063 = ORIENTED_EDGE ( 'NONE', *, *, #43554, .F. ) ;
#29064 = PLANE ( 'NONE',  #33716 ) ;
#29065 = LINE ( 'NONE', #20565, #4493 ) ;
#29066 = DIRECTION ( 'NONE',  ( 1.000000000000000000, -0.000000000000000000, 0.000000000000000000 ) ) ;
#29067 = AXIS2_PLACEMENT_3D ( 'NONE', #37881, #5606, #13866 ) ;
#29068 = ADVANCED_FACE ( 'NONE', ( #40751 ), #20869, .F. ) ;
#29069 = ORIENTED_EDGE ( 'NONE', *, *, #31338, .F. ) ;
#29070 = VECTOR ( 'NONE', #26536, 39.37007874015748854 ) ;
#29071 = DIRECTION ( 'NONE',  ( 1.000000000000000000, -0.000000000000000000, 0.000000000000000000 ) ) ;
#29072 = ORIENTED_EDGE ( 'NONE', *, *, #49196, .F. ) ;
#29073 = FACE_BOUND ( 'NONE', #9246, .T. ) ;
#29074 = CARTESIAN_POINT ( 'NONE',  ( -1.363819533518803029, 3.346456692913386100, 1.102362204724404160 ) ) ;
#29075 = AXIS2_PLACEMENT_3D ( 'NONE', #2643, #14521, #3400 ) ;
#29076 = VECTOR ( 'NONE', #13786, 39.37007874015748143 ) ;
#29077 = CARTESIAN_POINT ( 'NONE',  ( -0.5455278134075216556, 3.267716535433071279, -2.381957271744193250 ) ) ;
#29078 = CARTESIAN_POINT ( 'NONE',  ( 0.000000000000000000, 3.267716535433071279, 0.2755905511810998187 ) ) ;
#29079 = ORIENTED_EDGE ( 'NONE', *, *, #28067, .T. ) ;
#29080 = ORIENTED_EDGE ( 'NONE', *, *, #41203, .F. ) ;
#29081 = DIRECTION ( 'NONE',  ( -0.000000000000000000, 1.000000000000000000, -0.000000000000000000 ) ) ;
#29082 = EDGE_LOOP ( 'NONE', ( #48560, #1888, #19165, #33553 ) ) ;
#29083 = CARTESIAN_POINT ( 'NONE',  ( 2.182111253630085290, 3.346456692913386100, 0.6299212598425161236 ) ) ;
#29084 = ORIENTED_EDGE ( 'NONE', *, *, #48484, .F. ) ;
#29085 = CARTESIAN_POINT ( 'NONE',  ( 2.106197740627111958, 3.267716535433071279, 0.5905511811023582691 ) ) ;
#29086 = ORIENTED_EDGE ( 'NONE', *, *, #17996, .F. ) ;
#29087 = CARTESIAN_POINT ( 'NONE',  ( -0.8182917201112814842, 3.267716535433071279, 0.2755905511810998187 ) ) ;
#29088 = DIRECTION ( 'NONE',  ( 1.734723475976806848E-16, -0.000000000000000000, 1.000000000000000000 ) ) ;
#29089 = ORIENTED_EDGE ( 'NONE', *, *, #16176, .F. ) ;
#29090 = CARTESIAN_POINT ( 'NONE',  ( 1.015142113812069313, 3.346456692913386100, 0.4724409448818868706 ) ) ;
#29091 = EDGE_LOOP ( 'NONE', ( #3219, #36549, #1836, #4229 ) ) ;
#29092 = ORIENTED_EDGE ( 'NONE', *, *, #29349, .F. ) ;
#29093 = B_SPLINE_CURVE_WITH_KNOTS ( 'NONE', 3,
 ( #433, #16188, #47638, #12313 ),
 .UNSPECIFIED., .F., .F.,
 ( 4, 4 ),
 ( 6.016737642395432559E-07, 0.0003054758831321558767 ),
 .UNSPECIFIED. ) ;
#29094 = ORIENTED_EDGE ( 'NONE', *, *, #20618, .F. ) ;
#29095 = VERTEX_POINT ( 'NONE', #20614 ) ;
#29096 = DIRECTION ( 'NONE',  ( 1.000000000000000000, 0.000000000000000000, 0.000000000000000000 ) ) ;
#29097 = AXIS2_PLACEMENT_3D ( 'NONE', #651, #32160, #47850 ) ;
#29098 = ADVANCED_FACE ( 'NONE', ( #16232 ), #27445, .F. ) ;
#29099 = EDGE_CURVE ( 'NONE', #35527, #31327, #28090, .T. ) ;
#29100 = ORIENTED_EDGE ( 'NONE', *, *, #48486, .T. ) ;
#29101 = CARTESIAN_POINT ( 'NONE',  ( 0.5455278134075212115, 0.000000000000000000, -6.146657985744592735E-16 ) ) ;
#29102 = VERTEX_POINT ( 'NONE', #992 ) ;
#29103 = DIRECTION ( 'NONE',  ( 1.000000000000000000, 0.000000000000000000, -3.469446951953613696E-16 ) ) ;
#29104 = EDGE_CURVE ( 'NONE', #35146, #2592, #31213, .T. ) ;
#29105 = CIRCLE ( 'NONE', #4378, 2.952755905511811552 ) ;
#29106 = PRODUCT_RELATED_PRODUCT_CATEGORY ( 'part', '', ( #8350 ) ) ;
#29107 = VECTOR ( 'NONE', #44097, 39.37007874015748143 ) ;
#29108 = B_SPLINE_CURVE_WITH_KNOTS ( 'NONE', 3,
 ( #15950, #36352, #8464, #24474 ),
 .UNSPECIFIED., .F., .F.,
 ( 4, 4 ),
 ( 0.02871092247522269783, 0.03111204650372608252 ),
 .UNSPECIFIED. ) ;
#29109 = EDGE_CURVE ( 'NONE', #43424, #3538, #8511, .T. ) ;
#29110 = EDGE_CURVE ( 'NONE', #44277, #35815, #33779, .T. ) ;
#29111 = DIRECTION ( 'NONE',  ( 0.5128992774058948045, -9.966352232896248990E-17, 0.8584487936018727616 ) ) ;
#29112 = EDGE_LOOP ( 'NONE', ( #37759, #40521, #46843, #47837 ) ) ;
#29113 = CARTESIAN_POINT ( 'NONE',  ( -1.266372989542556393, 1.601078161548953771, -2.667458713958470895 ) ) ;
#29114 = CARTESIAN_POINT ( 'NONE',  ( -1.613340714851948965, 1.583636149837539975, -1.474425128113891814 ) ) ;
#29115 = AXIS2_PLACEMENT_3D ( 'NONE', #2472, #29319, #37335 ) ;
#29116 = ORIENTED_EDGE ( 'NONE', *, *, #19604, .F. ) ;
#29117 = CYLINDRICAL_SURFACE ( 'NONE', #6007, 0.3937007874015748254 ) ;
#29118 = CARTESIAN_POINT ( 'NONE',  ( -0.2727639067037602727, 0.000000000000000000, 1.850393700787392293 ) ) ;
#29119 = DIRECTION ( 'NONE',  ( -0.000000000000000000, 1.000000000000000000, -0.000000000000000000 ) ) ;
#29120 = DIRECTION ( 'NONE',  ( -0.000000000000000000, 1.000000000000000000, -0.000000000000000000 ) ) ;
#29121 = CARTESIAN_POINT ( 'NONE',  ( -1.166969139818015977, 3.267716535433071279, -0.1574803149606300023 ) ) ;
#29122 = EDGE_CURVE ( 'NONE', #37129, #34200, #29890, .T. ) ;
#29123 = ORIENTED_EDGE ( 'NONE', *, *, #45464, .T. ) ;
#29124 = DIRECTION ( 'NONE',  ( -0.01601477604151182663, 0.9998717552508123996, -0.000000000000000000 ) ) ;
#29125 = CARTESIAN_POINT ( 'NONE',  ( -0.5455278134075208785, 3.346456692913386100, 0.7480314960629874665 ) ) ;
#29126 = ORIENTED_EDGE ( 'NONE', *, *, #8466, .F. ) ;
#29127 = CARTESIAN_POINT ( 'NONE',  ( 2.106197740627111514, 3.201134874551266218, -1.299212598425194320 ) ) ;
#29128 = EDGE_CURVE ( 'NONE', #50633, #36517, #30773, .T. ) ;
#29129 = EDGE_LOOP ( 'NONE', ( #2800, #8268, #1165, #6194 ) ) ;
#29130 = DIRECTION ( 'NONE',  ( 1.000000000000000000, 0.000000000000000000, 0.000000000000000000 ) ) ;
#29131 = DIRECTION ( 'NONE',  ( -1.000000000000000000, 0.000000000000000000, 0.000000000000000000 ) ) ;
#29132 = DIRECTION ( 'NONE',  ( -0.000000000000000000, 1.000000000000000000, 0.000000000000000000 ) ) ;
#29133 =( BOUNDED_CURVE ( )  B_SPLINE_CURVE ( 3, ( #43194, #19956, #40373, #16617 ),
 .UNSPECIFIED., .F., .F. ) 
 B_SPLINE_CURVE_WITH_KNOTS ( ( 4, 4 ),
 ( 1.095572580490222991, 1.146464844878060996 ),
 .UNSPECIFIED. ) 
 CURVE ( )  GEOMETRIC_REPRESENTATION_ITEM ( )  RATIONAL_B_SPLINE_CURVE ( ( 1.000000000000000000, 0.9997841764314150392, 0.9997841764314150392, 1.000000000000000000 ) ) 
 REPRESENTATION_ITEM ( '' )  );
#29134 = DIRECTION ( 'NONE',  ( 0.000000000000000000, 0.000000000000000000, 1.000000000000000000 ) ) ;
#29135 = ORIENTED_EDGE ( 'NONE', *, *, #1010, .F. ) ;
#29136 = ADVANCED_FACE ( 'NONE', ( #38155 ), #18527, .F. ) ;
#29137 = CARTESIAN_POINT ( 'NONE',  ( 1.041764289084840645, 1.629758184783876240, -2.276669304528769366 ) ) ;
#29138 = AXIS2_PLACEMENT_3D ( 'NONE', #34878, #3377, #46709 ) ;
#29139 = CARTESIAN_POINT ( 'NONE',  ( -1.711605288297850969, 0.0005051743623580321960, -0.3401845456954783464 ) ) ;
#29140 = B_SPLINE_CURVE_WITH_KNOTS ( 'NONE', 3,
 ( #24927, #14070, #1432, #33955 ),
 .UNSPECIFIED., .F., .F.,
 ( 4, 4 ),
 ( 0.1211775127643062860, 0.1625894504277921315 ),
 .UNSPECIFIED. ) ;
#29141 = ORIENTED_EDGE ( 'NONE', *, *, #10007, .F. ) ;
#29142 = LINE ( 'NONE', #37165, #22153 ) ;
#29143 = CIRCLE ( 'NONE', #15946, 2.165354330708661568 ) ;
#29144 = ADVANCED_FACE ( 'NONE', ( #2524 ), #49967, .T. ) ;
#29145 = ORIENTED_EDGE ( 'NONE', *, *, #27977, .T. ) ;
#29146 = VECTOR ( 'NONE', #7628, 39.37007874015748143 ) ;
#29147 = VECTOR ( 'NONE', #29509, 39.37007874015748143 ) ;
#29148 = FACE_OUTER_BOUND ( 'NONE', #30163, .T. ) ;
#29149 = DIRECTION ( 'NONE',  ( -3.986037398843765983E-20, -1.000000000000000000, -1.160734090543304660E-16 ) ) ;
#29150 = FACE_OUTER_BOUND ( 'NONE', #29417, .T. ) ;
#29151 = AXIS2_PLACEMENT_3D ( 'NONE', #1117, #28482, #12484 ) ;
#29152 = CARTESIAN_POINT ( 'NONE',  ( -0.3486774197067340486, 3.346456692913386100, 2.077238655036873549 ) ) ;
#29153 = ORIENTED_EDGE ( 'NONE', *, *, #34610, .F. ) ;
#29154 = VERTEX_POINT ( 'NONE', #14650 ) ;
#29155 = CARTESIAN_POINT ( 'NONE',  ( -2.168245791271169676, 5.905511811023623991, -2.004968704497281262 ) ) ;
#29156 = CARTESIAN_POINT ( 'NONE',  ( 0.4696143004045484348, 3.267716535433071279, 0.9055118110236167750 ) ) ;
#29157 = FACE_BOUND ( 'NONE', #18232, .T. ) ;
#29158 = ORIENTED_EDGE ( 'NONE', *, *, #2217, .T. ) ;
#29159 = CARTESIAN_POINT ( 'NONE',  ( -0.5455278134075208785, 0.000000000000000000, 0.6299212598425164567 ) ) ;
#29160 = DIRECTION ( 'NONE',  ( -1.000000000000000000, 0.000000000000000000, 0.000000000000000000 ) ) ;
#29161 = ORIENTED_EDGE ( 'NONE', *, *, #9830, .T. ) ;
#29162 = DIRECTION ( 'NONE',  ( 1.000000000000000000, -0.000000000000000000, 0.000000000000000000 ) ) ;
#29163 = FACE_OUTER_BOUND ( 'NONE', #44309, .T. ) ;
#29164 = ORIENTED_EDGE ( 'NONE', *, *, #13737, .F. ) ;
#29165 = ORIENTED_EDGE ( 'NONE', *, *, #28214, .F. ) ;
#29166 = ORIENTED_EDGE ( 'NONE', *, *, #31102, .F. ) ;
#29167 = CARTESIAN_POINT ( 'NONE',  ( 0.08139965876239094178, 1.610780518492231694, 0.000000000000000000 ) ) ;
#29168 = EDGE_CURVE ( 'NONE', #1172, #23037, #48090, .T. ) ;
#29169 = CARTESIAN_POINT ( 'NONE',  ( 0.5455278134075216556, 3.267716535433071279, 2.095509194042718626 ) ) ;
#29170 = EDGE_CURVE ( 'NONE', #1675, #3555, #22147, .T. ) ;
#29171 = DIRECTION ( 'NONE',  ( -0.5407162030609373726, -0.6444004775717706579, 0.5407162030609373726 ) ) ;
#29172 = EDGE_CURVE ( 'NONE', #3461, #50816, #49714, .T. ) ;
#29173 = DIRECTION ( 'NONE',  ( -0.9998717552508121775, -0.01601477604151182316, 0.000000000000000000 ) ) ;
#29174 = ORIENTED_EDGE ( 'NONE', *, *, #15655, .F. ) ;
#29175 = VERTEX_POINT ( 'NONE', #18015 ) ;
#29176 = CIRCLE ( 'NONE', #21778, 2.164630168518208109 ) ;
#29177 = DIRECTION ( 'NONE',  ( -0.000000000000000000, 1.000000000000000000, -0.000000000000000000 ) ) ;
#29178 = LINE ( 'NONE', #4670, #1550 ) ;
#29179 = AXIS2_PLACEMENT_3D ( 'NONE', #18077, #31402, #37958 ) ;
#29180 = CARTESIAN_POINT ( 'NONE',  ( 0.000000000000000000, 0.000000000000000000, 0.000000000000000000 ) ) ;
#29181 = VECTOR ( 'NONE', #47641, 39.37007874015748143 ) ;
#29182 = DIRECTION ( 'NONE',  ( 0.000000000000000000, 0.000000000000000000, -1.000000000000000000 ) ) ;
#29183 = AXIS2_PLACEMENT_3D ( 'NONE', #30540, #37791, #42398 ) ;
#29184 = CARTESIAN_POINT ( 'NONE',  ( 2.878724150143186833, 5.905511811023623991, -0.6570500018394801467 ) ) ;
#29185 = AXIS2_PLACEMENT_3D ( 'NONE', #13451, #4934, #32571 ) ;
#29186 = CARTESIAN_POINT ( 'NONE',  ( 2.996777194923521126, 5.118110236220475784, 0.9139393566314087947 ) ) ;
#29187 = DIRECTION ( 'NONE',  ( 0.000000000000000000, 0.000000000000000000, -1.000000000000000000 ) ) ;
#29188 = CONICAL_SURFACE ( 'NONE', #36613, 3.483074324928249421, 1.244861948955335196 ) ;
#29189 = ORIENTED_EDGE ( 'NONE', *, *, #50740, .F. ) ;
#29190 = DIRECTION ( 'NONE',  ( -1.000000000000000000, 0.000000000000000000, -0.000000000000000000 ) ) ;
#29191 = CARTESIAN_POINT ( 'NONE',  ( 0.000000000000000000, 3.267716535433071279, 0.1181102362204701633 ) ) ;
#29192 = ORIENTED_EDGE ( 'NONE', *, *, #32699, .T. ) ;
#29193 = EDGE_LOOP ( 'NONE', ( #24622, #27879, #37812, #20424 ) ) ;
#29194 = CARTESIAN_POINT ( 'NONE',  ( -0.2727639067037602727, 0.000000000000000000, 0.5905511811023582691 ) ) ;
#29195 = DIRECTION ( 'NONE',  ( 1.734723475976806848E-16, 0.000000000000000000, 1.000000000000000000 ) ) ;
#29196 = ORIENTED_EDGE ( 'NONE', *, *, #20104, .T. ) ;
#29197 = EDGE_CURVE ( 'NONE', #18948, #24587, #9507, .T. ) ;
#29198 = VERTEX_POINT ( 'NONE', #48952 ) ;
#29199 = FACE_OUTER_BOUND ( 'NONE', #23169, .T. ) ;
#29200 = EDGE_CURVE ( 'NONE', #3200, #9387, #5971, .T. ) ;
#29201 = ORIENTED_EDGE ( 'NONE', *, *, #19658, .T. ) ;
#29202 = PLANE ( 'NONE',  #33455 ) ;
#29203 = DIRECTION ( 'NONE',  ( 1.734723475976806848E-16, 0.000000000000000000, 1.000000000000000000 ) ) ;
#29204 = EDGE_CURVE ( 'NONE', #24856, #19187, #10265, .T. ) ;
#29205 = ORIENTED_EDGE ( 'NONE', *, *, #15436, .T. ) ;
#29206 = AXIS2_PLACEMENT_3D ( 'NONE', #30759, #38264, #39004 ) ;
#29207 = ORIENTED_EDGE ( 'NONE', *, *, #11608, .F. ) ;
#29208 = ORIENTED_EDGE ( 'NONE', *, *, #14977, .T. ) ;
#29209 = DIRECTION ( 'NONE',  ( 1.000000000000000000, 0.000000000000000000, 0.000000000000000000 ) ) ;
#29210 = AXIS2_PLACEMENT_3D ( 'NONE', #36749, #32892, #9376 ) ;
#29211 = ORIENTED_EDGE ( 'NONE', *, *, #46888, .T. ) ;
#29212 = ORIENTED_EDGE ( 'NONE', *, *, #6289, .F. ) ;
#29213 = ADVANCED_FACE ( 'NONE', ( #30140 ), #25255, .F. ) ;
#29214 = VECTOR ( 'NONE', #25461, 39.37007874015748143 ) ;
#29215 = DIRECTION ( 'NONE',  ( -0.000000000000000000, 1.000000000000000000, -0.000000000000000000 ) ) ;
#29216 = PLANE ( 'NONE',  #50751 ) ;
#29217 = CARTESIAN_POINT ( 'NONE',  ( -1.091055626815042645, 3.267716535433071279, -0.3149606299212593941 ) ) ;
#29218 = B_SPLINE_CURVE_WITH_KNOTS ( 'NONE', 3,
 ( #35797, #47111, #157, #11781 ),
 .UNSPECIFIED., .F., .F.,
 ( 4, 4 ),
 ( 0.05979284115972890307, 0.06207050146966483495 ),
 .UNSPECIFIED. ) ;
#29219 = VECTOR ( 'NONE', #15169, 39.37007874015748143 ) ;
#29220 = EDGE_CURVE ( 'NONE', #14432, #11679, #25501, .T. ) ;
#29221 = VECTOR ( 'NONE', #33788, 39.37007874015748143 ) ;
#29222 = ORIENTED_EDGE ( 'NONE', *, *, #43632, .F. ) ;
#29223 = CARTESIAN_POINT ( 'NONE',  ( 0.000000000000000000, 3.267716535433071279, 0.000000000000000000 ) ) ;
#29224 = FACE_OUTER_BOUND ( 'NONE', #37783, .T. ) ;
#29225 = CARTESIAN_POINT ( 'NONE',  ( 1.006250229852934774, 3.346456692913386100, 1.850393700787392293 ) ) ;
#29226 = VERTEX_POINT ( 'NONE', #33268 ) ;
#29227 = CARTESIAN_POINT ( 'NONE',  ( 1.363819533518803251, 3.346456692913386100, 0.7874015748031454320 ) ) ;
#29228 = CARTESIAN_POINT ( 'NONE',  ( -0.7380211471543357549, 0.01609890615456165824, -1.645940171248041928 ) ) ;
#29229 = VECTOR ( 'NONE', #42830, 39.37007874015748143 ) ;
#29230 = CARTESIAN_POINT ( 'NONE',  ( 2.086662150992999010, 0.000000000000000000, -0.4594568716432768096 ) ) ;
#29231 = VERTEX_POINT ( 'NONE', #13637 ) ;
#29232 = ORIENTED_EDGE ( 'NONE', *, *, #21146, .F. ) ;
#29233 = EDGE_CURVE ( 'NONE', #8254, #15045, #29380, .T. ) ;
#29234 = DIRECTION ( 'NONE',  ( -3.469446951953613696E-16, 0.000000000000000000, -1.000000000000000000 ) ) ;
#29235 = LINE ( 'NONE', #1103, #14601 ) ;
#29236 = EDGE_CURVE ( 'NONE', #32813, #42496, #10016, .T. ) ;
#29237 = LINE ( 'NONE', #26381, #36266 ) ;
#29238 = EDGE_LOOP ( 'NONE', ( #34379, #14490, #45265, #3443 ) ) ;
#29239 = ORIENTED_EDGE ( 'NONE', *, *, #24037, .F. ) ;
#29240 = EDGE_CURVE ( 'NONE', #1553, #29362, #2766, .T. ) ;
#29241 = FACE_OUTER_BOUND ( 'NONE', #44528, .T. ) ;
#29242 = ORIENTED_EDGE ( 'NONE', *, *, #27909, .F. ) ;
#29243 = DIRECTION ( 'NONE',  ( 7.237058681235204266E-17, -1.000000000000000000, 9.074984547606538936E-17 ) ) ;
#29244 = DIRECTION ( 'NONE',  ( -6.394449067488487880E-17, -1.000000000000000000, -9.687176266499690201E-17 ) ) ;
#29245 = DIRECTION ( 'NONE',  ( 0.000000000000000000, -1.000000000000000000, 0.000000000000000000 ) ) ;
#29246 = DIRECTION ( 'NONE',  ( -0.000000000000000000, 0.000000000000000000, 1.000000000000000000 ) ) ;
#29247 = DIRECTION ( 'NONE',  ( -0.000000000000000000, -1.000000000000000000, -0.000000000000000000 ) ) ;
#29248 = ORIENTED_EDGE ( 'NONE', *, *, #6480, .T. ) ;
#29249 = VECTOR ( 'NONE', #31790, 39.37007874015748143 ) ;
#29250 = LINE ( 'NONE', #14019, #20073 ) ;
#29251 = AXIS2_PLACEMENT_3D ( 'NONE', #12676, #28411, #44160 ) ;
#29252 = CYLINDRICAL_SURFACE ( 'NONE', #1796, 2.874015748031496731 ) ;
#29253 = VECTOR ( 'NONE', #21852, 39.37007874015748143 ) ;
#29254 = B_SPLINE_CURVE_WITH_KNOTS ( 'NONE', 3,
 ( #12808, #36557, #39912, #12032 ),
 .UNSPECIFIED., .F., .F.,
 ( 4, 4 ),
 ( 2.074994163403008576E-07, 0.002500489216568123514 ),
 .UNSPECIFIED. ) ;
#29255 = ORIENTED_EDGE ( 'NONE', *, *, #27896, .T. ) ;
#29256 = LINE ( 'NONE', #13011, #44652 ) ;
#29257 = DIRECTION ( 'NONE',  ( 0.9998717552508121775, 0.01601477604151182663, 0.000000000000000000 ) ) ;
#29258 = DIRECTION ( 'NONE',  ( 1.000000000000000000, 0.000000000000000000, -3.469446951953613696E-16 ) ) ;
#29259 = ORIENTED_EDGE ( 'NONE', *, *, #18628, .F. ) ;
#29260 = EDGE_CURVE ( 'NONE', #50954, #10852, #41763, .T. ) ;
#29261 = CARTESIAN_POINT ( 'NONE',  ( -2.006326915404077038, 1.581476153537414220, -1.383332181782276127 ) ) ;
#29262 = LINE ( 'NONE', #25391, #40731 ) ;
#29263 = VECTOR ( 'NONE', #27887, 39.37007874015748143 ) ;
#29264 = ORIENTED_EDGE ( 'NONE', *, *, #35242, .F. ) ;
#29265 = DIRECTION ( 'NONE',  ( 1.000000000000000000, 0.000000000000000000, -3.469446951953613696E-16 ) ) ;
#29266 = CARTESIAN_POINT ( 'NONE',  ( -0.07591351300297333182, 3.346456692913386100, -0.7874015748031470974 ) ) ;
#29267 = ORIENTED_EDGE ( 'NONE', *, *, #40257, .T. ) ;
#29268 = LINE ( 'NONE', #1906, #42692 ) ;
#29269 = EDGE_CURVE ( 'NONE', #43429, #10488, #38402, .T. ) ;
#29270 = FACE_OUTER_BOUND ( 'NONE', #19676, .T. ) ;
#29271 = CARTESIAN_POINT ( 'NONE',  ( 2.182111253630085290, 3.267716535433071279, -3.785359618865289765E-16 ) ) ;
#29272 = CARTESIAN_POINT ( 'NONE',  ( -1.439733046521776361, 0.000000000000000000, 0.1181102362204704270 ) ) ;
#29273 = EDGE_CURVE ( 'NONE', #15190, #32538, #1620, .T. ) ;
#29274 = EDGE_CURVE ( 'NONE', #5605, #36136, #1100, .T. ) ;
#29275 = EDGE_CURVE ( 'NONE', #37703, #43876, #14903, .T. ) ;
#29276 = CARTESIAN_POINT ( 'NONE',  ( 2.734482843737263025, 5.118110236220475784, -1.115254632218672270 ) ) ;
#29277 = EDGE_LOOP ( 'NONE', ( #389, #44091, #34611, #26714 ) ) ;
#29278 = VERTEX_POINT ( 'NONE', #32120 ) ;
#29279 = DIRECTION ( 'NONE',  ( -1.000000000000000000, -0.000000000000000000, -0.000000000000000000 ) ) ;
#29280 = CARTESIAN_POINT ( 'NONE',  ( -0.4369915662458470074, 0.02092044581182531462, -1.768387524372482034 ) ) ;
#29281 = EDGE_LOOP ( 'NONE', ( #27941, #47802, #41378, #10115 ) ) ;
#29282 = LINE ( 'NONE', #17923, #20100 ) ;
#29283 = CARTESIAN_POINT ( 'NONE',  ( -0.9914495361339011881, 1.605369965488712136, 2.781765111341808705 ) ) ;
#29284 = CARTESIAN_POINT ( 'NONE',  ( -0.2727639067037610499, 3.346456692913386100, -2.088563196121306476 ) ) ;
#29285 = ORIENTED_EDGE ( 'NONE', *, *, #41734, .T. ) ;
#29286 = ORIENTED_EDGE ( 'NONE', *, *, #7135, .T. ) ;
#29287 = DIRECTION ( 'NONE',  ( 1.000000000000000000, 0.000000000000000000, 0.000000000000000000 ) ) ;
#29288 = DIRECTION ( 'NONE',  ( 7.105427357601001859E-15, 0.000000000000000000, -1.000000000000000000 ) ) ;
#29289 = LINE ( 'NONE', #33185, #25558 ) ;
#29290 = ORIENTED_EDGE ( 'NONE', *, *, #33582, .T. ) ;
#29291 = CARTESIAN_POINT ( 'NONE',  ( -0.3486774197067339376, 3.346456692913386100, -8.878505979408855953E-16 ) ) ;
#29292 = FACE_BOUND ( 'NONE', #43820, .T. ) ;
#29293 = AXIS2_PLACEMENT_3D ( 'NONE', #30651, #14394, #26513 ) ;
#29294 = ORIENTED_EDGE ( 'NONE', *, *, #38984, .F. ) ;
#29295 = VECTOR ( 'NONE', #16525, 39.37007874015748143 ) ;
#29296 = CARTESIAN_POINT ( 'NONE',  ( -1.909347346926324906, 3.346456692913386100, 1.417322834645662333 ) ) ;
#29297 = CIRCLE ( 'NONE', #27612, 2.165354330708661568 ) ;
#29298 = ORIENTED_EDGE ( 'NONE', *, *, #39673, .T. ) ;
#29299 = ORIENTED_EDGE ( 'NONE', *, *, #41798, .T. ) ;
#29300 = EDGE_CURVE ( 'NONE', #25793, #24046, #50213, .T. ) ;
#29301 = DIRECTION ( 'NONE',  ( 0.000000000000000000, 0.000000000000000000, -1.000000000000000000 ) ) ;
#29302 = CIRCLE ( 'NONE', #30955, 2.874015748031496731 ) ;
#29303 = ADVANCED_FACE ( 'NONE', ( #28220 ), #24362, .F. ) ;
#29304 = ORIENTED_EDGE ( 'NONE', *, *, #33179, .T. ) ;
#29305 = DIRECTION ( 'NONE',  ( 1.734723475976806848E-16, -0.000000000000000000, 1.000000000000000000 ) ) ;
#29307 = EDGE_CURVE ( 'NONE', #20045, #10888, #35034, .T. ) ;
#29306 = UNCERTAINTY_MEASURE_WITH_UNIT (LENGTH_MEASURE( 1.000000000000000082E-05 ), #10660, 'distance_accuracy_value', 'NONE');
#29308 = PLANE ( 'NONE',  #15585 ) ;
#29309 = ORIENTED_EDGE ( 'NONE', *, *, #20126, .F. ) ;
#29310 = VECTOR ( 'NONE', #47835, 39.37007874015748143 ) ;
#29311 = EDGE_CURVE ( 'NONE', #47095, #8152, #50707, .T. ) ;
#29312 = CARTESIAN_POINT ( 'NONE',  ( -0.8515791614234526907, 0.000000000000000000, 1.521253268579204398 ) ) ;
#29313 = LINE ( 'NONE', #17697, #36003 ) ;
#29314 = CARTESIAN_POINT ( 'NONE',  ( -0.5455278134075208785, 3.346456692913386100, 1.377952755905504256 ) ) ;
#29315 = PLANE ( 'NONE',  #14 ) ;
#29316 = FACE_OUTER_BOUND ( 'NONE', #15603, .T. ) ;
#29317 = CARTESIAN_POINT ( 'NONE',  ( -0.2468853591798393365, 0.5233347894274020806, -2.194114114529797988 ) ) ;
#29318 = ORIENTED_EDGE ( 'NONE', *, *, #35278, .F. ) ;
#29319 = DIRECTION ( 'NONE',  ( 1.000000000000000000, 0.000000000000000000, -3.469446951953613696E-16 ) ) ;
#29320 = LINE ( 'NONE', #25195, #26482 ) ;
#29321 = EDGE_LOOP ( 'NONE', ( #46026, #26343, #29080, #29020 ) ) ;
#29322 = CARTESIAN_POINT ( 'NONE',  ( 1.761123562704336232, 3.346456692913386100, -1.259842519685035800 ) ) ;
#29323 = DIRECTION ( 'NONE',  ( -3.469446951953613696E-16, 0.000000000000000000, -1.000000000000000000 ) ) ;
#29324 = EDGE_LOOP ( 'NONE', ( #39380, #23987, #6995, #19251 ) ) ;
#29325 = CARTESIAN_POINT ( 'NONE',  ( 0.2727639067037604392, 3.267716535433071279, -0.3543307086614173040 ) ) ;
#29326 = LINE ( 'NONE', #45556, #31615 ) ;
#29327 = LINE ( 'NONE', #45062, #43311 ) ;
#29328 = PRESENTATION_LAYER_ASSIGNMENT (  '', '', ( #40046 ) ) ;
#29329 = VECTOR ( 'NONE', #9201, 39.37007874015748143 ) ;
#29330 = ORIENTED_EDGE ( 'NONE', *, *, #25840, .T. ) ;
#29331 = PLANE ( 'NONE',  #23242 ) ;
#29332 = VERTEX_POINT ( 'NONE', #16621 ) ;
#29333 = FACE_BOUND ( 'NONE', #25237, .T. ) ;
#29334 = VECTOR ( 'NONE', #39748, 39.37007874015748143 ) ;
#29335 = DIRECTION ( 'NONE',  ( -3.469446951953613696E-16, 0.000000000000000000, -1.000000000000000000 ) ) ;
#29336 = CARTESIAN_POINT ( 'NONE',  ( -1.363819533518803029, 0.000000000000000000, 0.7874015748031456541 ) ) ;
#29337 = CARTESIAN_POINT ( 'NONE',  ( 0.000000000000000000, 3.267716535433071279, 0.7480314960629872445 ) ) ;
#29338 = ADVANCED_FACE ( 'NONE', ( #42764 ), #42256, .F. ) ;
#29339 = AXIS2_PLACEMENT_3D ( 'NONE', #29555, #17681, #49631 ) ;
#29340 = EDGE_CURVE ( 'NONE', #35616, #39217, #3532, .T. ) ;
#29341 = AXIS2_PLACEMENT_3D ( 'NONE', #35176, #3681, #7055 ) ;
#29342 = ORIENTED_EDGE ( 'NONE', *, *, #23207, .F. ) ;
#29343 = VERTEX_POINT ( 'NONE', #10771 ) ;
#29344 = EDGE_CURVE ( 'NONE', #12327, #23437, #30649, .T. ) ;
#29345 = DIRECTION ( 'NONE',  ( 1.734723475976806848E-16, -0.000000000000000000, 1.000000000000000000 ) ) ;
#29346 = ORIENTED_EDGE ( 'NONE', *, *, #29703, .T. ) ;
#29347 = LINE ( 'NONE', #12581, #34333 ) ;
#29348 = VERTEX_POINT ( 'NONE', #4741 ) ;
#29349 = EDGE_CURVE ( 'NONE', #50789, #18957, #5232, .T. ) ;
#29350 = LINE ( 'NONE', #45325, #27258 ) ;
#29351 = ORIENTED_EDGE ( 'NONE', *, *, #38283, .T. ) ;
#29352 = CARTESIAN_POINT ( 'NONE',  ( 1.636583440222563857, 3.267716535433071279, -2.839019714148966584E-16 ) ) ;
#29353 = CARTESIAN_POINT ( 'NONE',  ( -1.716372755931022454, 1.049866565067837820, -1.074000356310436555 ) ) ;
#29354 = VERTEX_POINT ( 'NONE', #38654 ) ;
#29355 = DIRECTION ( 'NONE',  ( 0.000000000000000000, 0.000000000000000000, 1.000000000000000000 ) ) ;
#29356 = ORIENTED_EDGE ( 'NONE', *, *, #28884, .F. ) ;
#29357 = ORIENTED_EDGE ( 'NONE', *, *, #46300, .F. ) ;
#29358 = EDGE_CURVE ( 'NONE', #660, #9566, #7162, .T. ) ;
#29359 = EDGE_CURVE ( 'NONE', #13304, #48175, #22899, .T. ) ;
#29360 = AXIS2_PLACEMENT_3D ( 'NONE', #37520, #29762, #48324 ) ;
#29361 = ORIENTED_EDGE ( 'NONE', *, *, #18220, .F. ) ;
#29362 = VERTEX_POINT ( 'NONE', #18775 ) ;
#29363 = CARTESIAN_POINT ( 'NONE',  ( -0.8942052331142552601, 3.346456692913386100, -0.1968503937007881899 ) ) ;
#29364 = VECTOR ( 'NONE', #45588, 39.37007874015748143 ) ;
#29365 = VECTOR ( 'NONE', #7648, 39.37007874015748143 ) ;
#29366 = ADVANCED_FACE ( 'NONE', ( #34529 ), #34776, .T. ) ;
#29367 = VERTEX_POINT ( 'NONE', #47808 ) ;
#29368 = CARTESIAN_POINT ( 'NONE',  ( 0.000000000000000000, 5.905511811023623991, 0.000000000000000000 ) ) ;
#29369 = EDGE_CURVE ( 'NONE', #19691, #6703, #12479, .T. ) ;
#29370 = VERTEX_POINT ( 'NONE', #11284 ) ;
#29371 = CARTESIAN_POINT ( 'NONE',  ( 1.526828301548457834, 3.267716535433071279, 1.535433070866133898 ) ) ;
#29372 = VECTOR ( 'NONE', #8589, 39.37007874015748143 ) ;
#29373 = CARTESIAN_POINT ( 'NONE',  ( 1.363819533518803029, 3.346456692913386100, -1.605145679676863724 ) ) ;
#29374 = ORIENTED_EDGE ( 'NONE', *, *, #48241, .F. ) ;
#29375 = AXIS2_PLACEMENT_3D ( 'NONE', #19293, #11807, #24200 ) ;
#29376 = CARTESIAN_POINT ( 'NONE',  ( 1.223349603905365068, 0.04751384826852676074, 1.475034436811822669 ) ) ;
#29377 = FACE_OUTER_BOUND ( 'NONE', #37137, .T. ) ;
#29378 = ORIENTED_EDGE ( 'NONE', *, *, #6289, .T. ) ;
#29379 = DIRECTION ( 'NONE',  ( -0.000000000000000000, -1.000000000000000000, -0.000000000000000000 ) ) ;
#29380 = LINE ( 'NONE', #45103, #17619 ) ;
#29381 = B_SPLINE_CURVE_WITH_KNOTS ( 'NONE', 3,
 ( #43210, #877, #20498, #16889 ),
 .UNSPECIFIED., .F., .F.,
 ( 4, 4 ),
 ( 0.1211873102087489551, 0.1625992483279400380 ),
 .UNSPECIFIED. ) ;
#29382 = DIRECTION ( 'NONE',  ( 1.734723475976806848E-16, -0.000000000000000000, 1.000000000000000000 ) ) ;
#29383 = LINE ( 'NONE', #37398, #126 ) ;
#29384 = DIRECTION ( 'NONE',  ( -0.6234898018587318180, 0.000000000000000000, -0.7818314824680309139 ) ) ;
#29385 = DIRECTION ( 'NONE',  ( 0.000000000000000000, 0.000000000000000000, -1.000000000000000000 ) ) ;
#29386 = VERTEX_POINT ( 'NONE', #27012 ) ;
#29387 = DIRECTION ( 'NONE',  ( 0.000000000000000000, 0.000000000000000000, -1.000000000000000000 ) ) ;
#29388 = CARTESIAN_POINT ( 'NONE',  ( 0.000000000000000000, 3.267716535433071279, -0.7874015748031473194 ) ) ;
#29389 = ORIENTED_EDGE ( 'NONE', *, *, #12328, .F. ) ;
#29390 = LINE ( 'NONE', #1002, #15189 ) ;
#29391 = EDGE_LOOP ( 'NONE', ( #37551, #48283, #7454, #24480 ) ) ;
#29392 = PLANE ( 'NONE',  #41017 ) ;
#29393 = LINE ( 'NONE', #25268, #25061 ) ;
#29394 = CARTESIAN_POINT ( 'NONE',  ( -1.905671854841497481, 1.591126119768930147, 2.256015092822653223 ) ) ;
#29395 = CARTESIAN_POINT ( 'NONE',  ( 0.5455278134075216556, 3.346456692913386100, 1.692913385826762873 ) ) ;
#29396 = CARTESIAN_POINT ( 'NONE',  ( 0.2810050591710572809, 1.508447189148403922, -2.939399966304093503 ) ) ;
#29397 = VERTEX_POINT ( 'NONE', #40376 ) ;
#29398 = VECTOR ( 'NONE', #41268, 39.37007874015748143 ) ;
#29399 = LINE ( 'NONE', #10546, #29070 ) ;
#29400 = EDGE_CURVE ( 'NONE', #21767, #36721, #31794, .T. ) ;
#29401 = VECTOR ( 'NONE', #26753, 39.37007874015748143 ) ;
#29402 = DIRECTION ( 'NONE',  ( -0.000000000000000000, -1.000000000000000000, -0.000000000000000000 ) ) ;
#29403 = ADVANCED_FACE ( 'NONE', ( #40876 ), #28735, .F. ) ;
#29404 = CARTESIAN_POINT ( 'NONE',  ( -1.486187880958816931, 3.346456692913386100, 1.574803149606291530 ) ) ;
#29405 = VECTOR ( 'NONE', #6069, 39.37007874015748143 ) ;
#29406 = ORIENTED_EDGE ( 'NONE', *, *, #21703, .T. ) ;
#29407 = CARTESIAN_POINT ( 'NONE',  ( -1.395323331152583002, 0.5249316475426865081, -1.265979166134213241 ) ) ;
#29408 = CARTESIAN_POINT ( 'NONE',  ( -1.195183497228115035E-16, 3.267716535433071279, 0.6299212598425161236 ) ) ;
#29409 = EDGE_LOOP ( 'NONE', ( #34096, #44926, #9010, #18823, #38389, #13824, #28831, #41168, #9342, #41518, #31500, #14440, #17490 ) ) ;
#29410 = EDGE_CURVE ( 'NONE', #28112, #47130, #17130, .T. ) ;
#29411 = DIRECTION ( 'NONE',  ( 0.000000000000000000, 0.000000000000000000, -1.000000000000000000 ) ) ;
#29412 = VECTOR ( 'NONE', #32694, 39.37007874015748143 ) ;
#29413 = CARTESIAN_POINT ( 'NONE',  ( -0.6214413264104944323, 3.267716535433071279, 2.156057715732900533E-16 ) ) ;
#29414 = ADVANCED_FACE ( 'NONE', ( #25630 ), #1375, .F. ) ;
#29415 = VECTOR ( 'NONE', #836, 39.37007874015748143 ) ;
#29416 = DIRECTION ( 'NONE',  ( 1.558091277195270436E-17, -1.000000000000000000, -1.150229170499806500E-16 ) ) ;
#29417 = EDGE_LOOP ( 'NONE', ( #894, #35664, #22196, #27662, #38328, #30977, #43418, #30936, #14700, #27756, #43489, #30814, #32031, #17927, #45322, #5839, #24787 ) ) ;
#29418 = ORIENTED_EDGE ( 'NONE', *, *, #26444, .F. ) ;
#29419 = LINE ( 'NONE', #9802, #37235 ) ;
#29420 = FACE_BOUND ( 'NONE', #39670, .T. ) ;
#29421 = ORIENTED_EDGE ( 'NONE', *, *, #36660, .F. ) ;
#29422 = DIRECTION ( 'NONE',  ( -0.000000000000000000, 1.000000000000000000, -0.000000000000000000 ) ) ;
#29423 = EDGE_CURVE ( 'NONE', #44234, #17956, #32896, .T. ) ;
#29424 = FACE_OUTER_BOUND ( 'NONE', #3816, .T. ) ;
#29425 = EDGE_LOOP ( 'NONE', ( #28666, #786, #23377, #304 ) ) ;
#29426 = ORIENTED_EDGE ( 'NONE', *, *, #40059, .T. ) ;
#29427 = B_SPLINE_CURVE_WITH_KNOTS ( 'NONE', 3,
 ( #21652, #44371, #29655, #45121 ),
 .UNSPECIFIED., .F., .F.,
 ( 4, 4 ),
 ( 0.002197616311132118659, 0.003926668439082322930 ),
 .UNSPECIFIED. ) ;
#29428 = FACE_OUTER_BOUND ( 'NONE', #34913, .T. ) ;
#29429 = CARTESIAN_POINT ( 'NONE',  ( -2.076676417810221942, 1.641831778720078017, 0.6230078826482280396 ) ) ;
#29430 = EDGE_CURVE ( 'NONE', #23868, #4959, #5504, .T. ) ;
#29431 = ORIENTED_EDGE ( 'NONE', *, *, #9344, .T. ) ;
#29432 = ORIENTED_EDGE ( 'NONE', *, *, #14318, .T. ) ;
#29433 = ORIENTED_EDGE ( 'NONE', *, *, #40201, .T. ) ;
#29434 = DIRECTION ( 'NONE',  ( -3.469446951953613696E-16, 0.000000000000000000, -1.000000000000000000 ) ) ;
#29435 = CARTESIAN_POINT ( 'NONE',  ( -1.439733046521776583, 0.000000000000000000, -1.259842519685034468 ) ) ;
#29437 = CARTESIAN_POINT ( 'NONE',  ( -1.363819533518803473, 0.000000000000000000, 1.732283464566920950 ) ) ;
#29436 = AXIS2_PLACEMENT_3D ( 'NONE', #45237, #11165, #26897 ) ;
#29438 = LINE ( 'NONE', #37197, #49410 ) ;
#29439 = ORIENTED_EDGE ( 'NONE', *, *, #37012, .F. ) ;
#29440 = ORIENTED_EDGE ( 'NONE', *, *, #37072, .T. ) ;
#29442 = CIRCLE ( 'NONE', #26918, 2.165354330708661568 ) ;
#29441 = DIRECTION ( 'NONE',  ( -0.000000000000000000, 1.000000000000000000, -0.000000000000000000 ) ) ;
#29443 = DIRECTION ( 'NONE',  ( -1.000000000000000000, 0.000000000000000000, 0.000000000000000000 ) ) ;
#29444 = CARTESIAN_POINT ( 'NONE',  ( 0.000000000000000000, 3.267716535433071279, 0.1574803149606283648 ) ) ;
#29445 = EDGE_CURVE ( 'NONE', #28145, #29278, #44478, .T. ) ;
#29446 = CARTESIAN_POINT ( 'NONE',  ( 0.000000000000000000, 3.346456692913386100, -2.493791675044291445 ) ) ;
#29447 = DIRECTION ( 'NONE',  ( 0.000000000000000000, 0.000000000000000000, 1.000000000000000000 ) ) ;
#29448 = CARTESIAN_POINT ( 'NONE',  ( -2.160407304981126320, 6.692913385826772199, -0.1462862061266902158 ) ) ;
#29449 =( BOUNDED_CURVE ( )  B_SPLINE_CURVE ( 3, ( #27274, #47371, #11786, #31413 ),
 .UNSPECIFIED., .F., .F. ) 
 B_SPLINE_CURVE_WITH_KNOTS ( ( 4, 4 ),
 ( 4.146021982105191128, 4.196929668049186546 ),
 .UNSPECIFIED. ) 
 CURVE ( )  GEOMETRIC_REPRESENTATION_ITEM ( )  RATIONAL_B_SPLINE_CURVE ( ( 1.000000000000000000, 0.9997840456193998193, 0.9997840456193998193, 1.000000000000000000 ) ) 
 REPRESENTATION_ITEM ( '' )  );
#29450 = VECTOR ( 'NONE', #24091, 39.37007874015748143 ) ;
#29451 = LINE ( 'NONE', #48259, #23390 ) ;
#29452 = ORIENTED_EDGE ( 'NONE', *, *, #10869, .T. ) ;
#29453 = DIRECTION ( 'NONE',  ( 0.000000000000000000, 0.000000000000000000, 1.000000000000000000 ) ) ;
#29454 = DIRECTION ( 'NONE',  ( -3.986037398843765983E-20, -1.000000000000000000, -1.160734090543304660E-16 ) ) ;
#29455 = VERTEX_POINT ( 'NONE', #33401 ) ;
#29456 = VERTEX_POINT ( 'NONE', #44228 ) ;
#29457 = CARTESIAN_POINT ( 'NONE',  ( 1.930190994932110771, 5.905511811023623991, -0.9827944786818444411 ) ) ;
#29458 = CARTESIAN_POINT ( 'NONE',  ( 1.015142113812069313, 3.267716535433071279, -0.3543307086614175816 ) ) ;
#29459 = ORIENTED_EDGE ( 'NONE', *, *, #23193, .T. ) ;
#29460 = EDGE_CURVE ( 'NONE', #28307, #29367, #37265, .T. ) ;
#29461 = ORIENTED_EDGE ( 'NONE', *, *, #4226, .F. ) ;
#29462 = LINE ( 'NONE', #33097, #9768 ) ;
#29463 = ORIENTED_EDGE ( 'NONE', *, *, #3262, .T. ) ;
#29464 = EDGE_CURVE ( 'NONE', #15158, #29676, #28985, .T. ) ;
#29465 = CARTESIAN_POINT ( 'NONE',  ( 1.909347346926324462, 3.267716535433071279, -3.312189666507127188E-16 ) ) ;
#29466 = B_SPLINE_CURVE_WITH_KNOTS ( 'NONE', 3,
 ( #26679, #11692, #30815, #38818 ),
 .UNSPECIFIED., .F., .F.,
 ( 4, 4 ),
 ( 0.01469741895130448860, 0.03075036094151098465 ),
 .UNSPECIFIED. ) ;
#29467 = DIRECTION ( 'NONE',  ( -1.000000000000000000, -0.000000000000000000, -0.000000000000000000 ) ) ;
#29468 = EDGE_CURVE ( 'NONE', #36377, #16144, #37013, .T. ) ;
#29469 = VECTOR ( 'NONE', #49817, 39.37007874015748143 ) ;
#29470 = AXIS2_PLACEMENT_3D ( 'NONE', #49289, #48778, #24821 ) ;
#29471 = EDGE_CURVE ( 'NONE', #29695, #39301, #47806, .T. ) ;
#29472 = VERTEX_POINT ( 'NONE', #36497 ) ;
#29473 = ORIENTED_EDGE ( 'NONE', *, *, #29172, .F. ) ;
#29474 = CONICAL_SURFACE ( 'NONE', #7222, 2.244934639244524632, 1.554780866114618743 ) ;
#29475 = CARTESIAN_POINT ( 'NONE',  ( 0.8952071785065199849, 1.205361022782829114E-17, 1.972340328593147785 ) ) ;
#29476 = ORIENTED_EDGE ( 'NONE', *, *, #29753, .F. ) ;
#29477 = ORIENTED_EDGE ( 'NONE', *, *, #28935, .T. ) ;
#29478 = DIRECTION ( 'NONE',  ( 1.142080616180678453E-16, -1.000000000000000000, 2.072570748943325363E-17 ) ) ;
#29479 = DIRECTION ( 'NONE',  ( 1.000000000000000000, 0.000000000000000000, 0.000000000000000000 ) ) ;
#29480 = DIRECTION ( 'NONE',  ( 1.000000000000000000, 0.000000000000000000, 0.000000000000000000 ) ) ;
#29481 = ORIENTED_EDGE ( 'NONE', *, *, #42754, .F. ) ;
#29482 = CARTESIAN_POINT ( 'NONE',  ( 0.2156685157584260770, 1.510622172706404864, -2.945280361644574185 ) ) ;
#29483 = ADVANCED_FACE ( 'NONE', ( #5759 ), #41539, .T. ) ;
#29484 = DIRECTION ( 'NONE',  ( 0.000000000000000000, 1.000000000000000000, 0.000000000000000000 ) ) ;
#29485 = CARTESIAN_POINT ( 'NONE',  ( 2.106197740627111958, 3.346456692913386100, -0.6692913385826764205 ) ) ;
#29486 = ORIENTED_EDGE ( 'NONE', *, *, #29110, .T. ) ;
#29487 = CARTESIAN_POINT ( 'NONE',  ( 0.000000000000000000, 6.692913385826772199, 0.000000000000000000 ) ) ;
#29488 = DIRECTION ( 'NONE',  ( 0.8090169943749422332, -1.160734090543304660E-16, 0.5877852522924802425 ) ) ;
#29489 = LINE ( 'NONE', #48805, #26595 ) ;
#29490 = EDGE_CURVE ( 'NONE', #30462, #36192, #11642, .T. ) ;
#29491 = ORIENTED_EDGE ( 'NONE', *, *, #49335, .T. ) ;
#29492 = ORIENTED_EDGE ( 'NONE', *, *, #26098, .F. ) ;
#29493 =( NAMED_UNIT ( * ) SI_UNIT ( $, .STERADIAN. ) SOLID_ANGLE_UNIT ( ) );
#29494 = AXIS2_PLACEMENT_3D ( 'NONE', #6599, #38097, #29054 ) ;
#29495 = CARTESIAN_POINT ( 'NONE',  ( 1.287906020515830363, 3.267716535433071279, -4.468321617281356063E-16 ) ) ;
#29496 = ADVANCED_FACE ( 'NONE', ( #48323 ), #9377, .F. ) ;
#29497 = CARTESIAN_POINT ( 'NONE',  ( -1.905671854841497481, 1.555429617898292705, 2.256015092822653667 ) ) ;
#29498 = B_SPLINE_CURVE_WITH_KNOTS ( 'NONE', 3,
 ( #35494, #23872, #8382, #31622 ),
 .UNSPECIFIED., .F., .F.,
 ( 4, 4 ),
 ( 6.057676006406350327E-07, 0.0007515069461672322206 ),
 .UNSPECIFIED. ) ;
#29499 = CARTESIAN_POINT ( 'NONE',  ( -2.491402175429631605, 1.680428061220146096, -1.585592796919542025 ) ) ;
#29500 = ORIENTED_EDGE ( 'NONE', *, *, #35026, .F. ) ;
#29501 = ORIENTED_EDGE ( 'NONE', *, *, #45468, .T. ) ;
#29502 = PLANE ( 'NONE',  #14374 ) ;
#29503 = ORIENTED_EDGE ( 'NONE', *, *, #16710, .T. ) ;
#29504 = LINE ( 'NONE', #44476, #20828 ) ;
#29505 = EDGE_CURVE ( 'NONE', #34486, #11040, #9891, .T. ) ;
#29506 = CARTESIAN_POINT ( 'NONE',  ( -2.083222340934659300, 0.5254407309824460359, -0.5259600971123018498 ) ) ;
#29507 = VECTOR ( 'NONE', #374, 39.37007874015748143 ) ;
#29508 = VECTOR ( 'NONE', #41278, 39.37007874015748143 ) ;
#29509 = DIRECTION ( 'NONE',  ( 1.000000000000000000, -0.000000000000000000, 0.000000000000000000 ) ) ;
#29510 = LINE ( 'NONE', #9892, #26869 ) ;
#29511 = LINE ( 'NONE', #22024, #23766 ) ;
#29512 = VERTEX_POINT ( 'NONE', #45226 ) ;
#29513 = LINE ( 'NONE', #45230, #5238 ) ;
#29514 = DIRECTION ( 'NONE',  ( 1.000000000000000000, 0.000000000000000000, 0.000000000000000000 ) ) ;
#29515 = EDGE_CURVE ( 'NONE', #40104, #42907, #12740, .T. ) ;
#29516 = VECTOR ( 'NONE', #33569, 39.37007874015748143 ) ;
#29517 = CARTESIAN_POINT ( 'NONE',  ( 0.8329809839909850799, 1.633788288308783976, -2.833254665166554442 ) ) ;
#29518 = EDGE_CURVE ( 'NONE', #17531, #38065, #37519, .T. ) ;
#29519 = ORIENTED_EDGE ( 'NONE', *, *, #45839, .T. ) ;
#29520 = DIRECTION ( 'NONE',  ( 1.000000000000000000, 0.000000000000000000, 0.000000000000000000 ) ) ;
#29521 = FACE_OUTER_BOUND ( 'NONE', #28403, .T. ) ;
#29522 = FACE_OUTER_BOUND ( 'NONE', #7635, .T. ) ;
#29523 = VERTEX_POINT ( 'NONE', #33649 ) ;
#29524 = CARTESIAN_POINT ( 'NONE',  ( -2.221753473495927445, 1.582160102031600735, -1.525534007743318377 ) ) ;
#29525 = VECTOR ( 'NONE', #50510, 39.37007874015748143 ) ;
#29526 = DIRECTION ( 'NONE',  ( -3.469446951953613696E-16, 0.000000000000000000, -1.000000000000000000 ) ) ;
#29527 = ORIENTED_EDGE ( 'NONE', *, *, #43378, .F. ) ;
#29528 = PLANE ( 'NONE',  #2446 ) ;
#29529 = CARTESIAN_POINT ( 'NONE',  ( -0.07591351300297333182, 3.267716535433071279, -1.102362204724405714 ) ) ;
#29530 = ORIENTED_EDGE ( 'NONE', *, *, #23225, .F. ) ;
#29531 = AXIS2_PLACEMENT_3D ( 'NONE', #23028, #15029, #46488 ) ;
#29532 = DIRECTION ( 'NONE',  ( -0.000000000000000000, 1.000000000000000000, -0.000000000000000000 ) ) ;
#29533 = ADVANCED_FACE ( 'NONE', ( #38284 ), #10140, .T. ) ;
#29534 = CARTESIAN_POINT ( 'NONE',  ( 1.833433833923351353, 3.346456692913386100, -1.036830145017913596 ) ) ;
#29535 = DIRECTION ( 'NONE',  ( -0.000000000000000000, 1.000000000000000000, -0.000000000000000000 ) ) ;
#29536 = DIRECTION ( 'NONE',  ( 0.000000000000000000, 0.000000000000000000, -1.000000000000000000 ) ) ;
#29537 = EDGE_CURVE ( 'NONE', #35582, #970, #46486, .T. ) ;
#29538 = LINE ( 'NONE', #45254, #46899 ) ;
#29539 = ORIENTED_EDGE ( 'NONE', *, *, #18299, .T. ) ;
#29540 = ORIENTED_EDGE ( 'NONE', *, *, #50776, .F. ) ;
#29541 = CARTESIAN_POINT ( 'NONE',  ( 0.000000000000000000, 3.267716535433071279, -0.6299212598425181220 ) ) ;
#29542 = CARTESIAN_POINT ( 'NONE',  ( 2.182111253630085290, 3.346456692913386100, 0.4330708661417287386 ) ) ;
#29543 = ORIENTED_EDGE ( 'NONE', *, *, #23941, .T. ) ;
#29544 = LINE ( 'NONE', #13799, #10250 ) ;
#29545 = DIRECTION ( 'NONE',  ( -0.8660254037844362651, 0.000000000000000000, 0.5000000000000041078 ) ) ;
#29546 = DIRECTION ( 'NONE',  ( 5.782411586589357392E-17, -0.000000000000000000, 1.000000000000000000 ) ) ;
#29547 = EDGE_LOOP ( 'NONE', ( #43358, #45789, #38751, #47693 ) ) ;
#29548 = ORIENTED_EDGE ( 'NONE', *, *, #21056, .F. ) ;
#29549 = LINE ( 'NONE', #18437, #33741 ) ;
#29550 = CARTESIAN_POINT ( 'NONE',  ( 0.1968503937007872462, 3.267716535433071279, -1.456692913385822630 ) ) ;
#29551 = AXIS2_PLACEMENT_3D ( 'NONE', #11053, #41790, #26792 ) ;
#29552 = DIRECTION ( 'NONE',  ( -0.000000000000000000, -1.000000000000000000, -0.000000000000000000 ) ) ;
#29553 = VERTEX_POINT ( 'NONE', #49340 ) ;
#29554 = CARTESIAN_POINT ( 'NONE',  ( -2.139032205770588835, 1.608024637552048164, 0.3394136515002111887 ) ) ;
#29555 = CARTESIAN_POINT ( 'NONE',  ( -1.091055626815042201, 0.000000000000000000, 1.574803149606291974 ) ) ;
#29556 = ORIENTED_EDGE ( 'NONE', *, *, #21839, .T. ) ;
#29557 = DIRECTION ( 'NONE',  ( 1.734723475976806848E-16, -0.000000000000000000, 1.000000000000000000 ) ) ;
#29558 = ORIENTED_EDGE ( 'NONE', *, *, #14003, .T. ) ;
#29560 = ORIENTED_EDGE ( 'NONE', *, *, #10841, .T. ) ;
#29559 = CIRCLE ( 'NONE', #3972, 2.165354330708661568 ) ;
#29561 = DIRECTION ( 'NONE',  ( 0.5773502691896241767, 0.5773502691896261751, 0.5773502691896268413 ) ) ;
#29562 = DIRECTION ( 'NONE',  ( -1.000000000000000000, 0.000000000000000000, -0.000000000000000000 ) ) ;
#29563 = VECTOR ( 'NONE', #2353, 39.37007874015748143 ) ;
#29565 = ORIENTED_EDGE ( 'NONE', *, *, #28638, .T. ) ;
#29564 = ADVANCED_FACE ( 'NONE', ( #49586 ), #11150, .F. ) ;
#29566 = CARTESIAN_POINT ( 'NONE',  ( 0.8182917201112819283, 0.000000000000000000, -1.102362204724405714 ) ) ;
#29568 = CARTESIAN_POINT ( 'NONE',  ( 1.636583440222563857, 3.346456692913386100, -0.6299212598425181220 ) ) ;
#29567 = VECTOR ( 'NONE', #1179, 39.37007874015748143 ) ;
#29569 = ORIENTED_EDGE ( 'NONE', *, *, #29887, .F. ) ;
#29570 = VECTOR ( 'NONE', #39159, 39.37007874015748143 ) ;
#29571 = CARTESIAN_POINT ( 'NONE',  ( 0.9248149864487152927, 1.627908877233774421, 2.324103449680534172 ) ) ;
#29572 = EDGE_CURVE ( 'NONE', #25302, #13127, #22518, .T. ) ;
#29573 = CARTESIAN_POINT ( 'NONE',  ( -1.859752235501543227, 0.5249316475426858419, 0.3015826090669521120 ) ) ;
#29574 = VECTOR ( 'NONE', #21630, 39.37007874015748143 ) ;
#29575 = EDGE_CURVE ( 'NONE', #11672, #45506, #45252, .T. ) ;
#29576 = ADVANCED_FACE ( 'NONE', ( #10896 ), #30271, .F. ) ;
#29577 = CARTESIAN_POINT ( 'NONE',  ( -2.951990591674674480, 1.205361022782829114E-17, -0.08331184815402571664 ) ) ;
#29578 = CARTESIAN_POINT ( 'NONE',  ( -1.363819533518803473, 3.346456692913386100, -1.929133858267710000 ) ) ;
#29579 = CARTESIAN_POINT ( 'NONE',  ( -0.2802969821979833243, 1.022684513435495157, -2.565347650952780612 ) ) ;
#29580 = ORIENTED_EDGE ( 'NONE', *, *, #20066, .F. ) ;
#29581 = FACE_OUTER_BOUND ( 'NONE', #25740, .T. ) ;
#29582 = B_SPLINE_CURVE_WITH_KNOTS ( 'NONE', 3,
 ( #5118, #20354, #40240, #12611 ),
 .UNSPECIFIED., .F., .F.,
 ( 4, 4 ),
 ( 0.0001573404397883737223, 0.004927678653679096535 ),
 .UNSPECIFIED. ) ;
#29583 = DIRECTION ( 'NONE',  ( 0.01601477604151182663, -0.9998717552508123996, 0.000000000000000000 ) ) ;
#29584 = ORIENTED_EDGE ( 'NONE', *, *, #28829, .T. ) ;
#29585 = DIRECTION ( 'NONE',  ( 1.000000000000000000, 0.000000000000000000, -3.469446951953613696E-16 ) ) ;
#29586 = FACE_OUTER_BOUND ( 'NONE', #34774, .T. ) ;
#29587 = ORIENTED_EDGE ( 'NONE', *, *, #45941, .F. ) ;
#29588 = CARTESIAN_POINT ( 'NONE',  ( -1.091055626815042201, 3.346456692913386100, 1.062992125984246083 ) ) ;
#29589 = VECTOR ( 'NONE', #37875, 39.37007874015748143 ) ;
#29590 = EDGE_CURVE ( 'NONE', #4720, #47282, #14778, .T. ) ;
#29591 = CARTESIAN_POINT ( 'NONE',  ( 4.268512490100411402E-16, 3.346456692913386100, 2.204724409448808764 ) ) ;
#29592 = DIRECTION ( 'NONE',  ( -0.000000000000000000, 1.000000000000000000, -0.000000000000000000 ) ) ;
#29593 = VERTEX_POINT ( 'NONE', #38775 ) ;
#29594 = CARTESIAN_POINT ( 'NONE',  ( 2.932638728931774352, 1.205361022782829114E-17, 0.3475908556738223631 ) ) ;
#29595 = EDGE_LOOP ( 'NONE', ( #13425, #10698, #11314, #33447 ) ) ;
#29596 = FACE_BOUND ( 'NONE', #43625, .T. ) ;
#29597 = CARTESIAN_POINT ( 'NONE',  ( 0.7759887336347247588, 0.04034854520891290042, -1.724780676950718794 ) ) ;
#29598 = EDGE_CURVE ( 'NONE', #4856, #13403, #22022, .T. ) ;
#29599 = VECTOR ( 'NONE', #3444, 39.37007874015748143 ) ;
#29600 = AXIS2_PLACEMENT_3D ( 'NONE', #27601, #4376, #7992 ) ;
#29601 = DIRECTION ( 'NONE',  ( -0.01601477604151182663, 0.9998717552508123996, -0.000000000000000000 ) ) ;
#29602 = CARTESIAN_POINT ( 'NONE',  ( -2.182111253630085290, 0.000000000000000000, 0.3149606299212578953 ) ) ;
#29603 = EDGE_CURVE ( 'NONE', #38735, #20325, #8991, .T. ) ;
#29604 = EDGE_CURVE ( 'NONE', #8748, #14593, #26142, .T. ) ;
#29605 = CIRCLE ( 'NONE', #5682, 1.743387098533651480 ) ;
#29606 = ORIENTED_EDGE ( 'NONE', *, *, #29172, .T. ) ;
#29607 = ORIENTED_EDGE ( 'NONE', *, *, #41598, .F. ) ;
#29608 = LINE ( 'NONE', #41475, #8978 ) ;
#29609 = VERTEX_POINT ( 'NONE', #2399 ) ;
#29610 = VECTOR ( 'NONE', #39860, 39.37007874015748143 ) ;
#29611 = CARTESIAN_POINT ( 'NONE',  ( 3.937007874015748143, 0.000000000000000000, 0.000000000000000000 ) ) ;
#29612 = ORIENTED_EDGE ( 'NONE', *, *, #36156, .F. ) ;
#29613 = CARTESIAN_POINT ( 'NONE',  ( -0.07591351300297333182, 0.000000000000000000, 0.4724409448818869817 ) ) ;
#29614 = ORIENTED_EDGE ( 'NONE', *, *, #39086, .T. ) ;
#29615 = DIRECTION ( 'NONE',  ( -1.000000000000000000, -0.000000000000000000, -0.000000000000000000 ) ) ;
#29616 = CARTESIAN_POINT ( 'NONE',  ( 2.013783482383322720, 1.740156378764222245, 1.139548688847630942 ) ) ;
#29617 = B_SPLINE_CURVE_WITH_KNOTS ( 'NONE', 3,
 ( #17405, #41407, #9916, #6033 ),
 .UNSPECIFIED., .F., .F.,
 ( 4, 4 ),
 ( 0.001422306547608694852, 0.003922515224842213107 ),
 .UNSPECIFIED. ) ;
#29618 = VERTEX_POINT ( 'NONE', #38529 ) ;
#29619 = CARTESIAN_POINT ( 'NONE',  ( 1.442672029790674104, 1.738133376546725506, 2.318676429272163109 ) ) ;
#29620 = ORIENTED_EDGE ( 'NONE', *, *, #2597, .T. ) ;
#29621 = ORIENTED_EDGE ( 'NONE', *, *, #30782, .F. ) ;
#29622 = VECTOR ( 'NONE', #2431, 39.37007874015748143 ) ;
#29623 = EDGE_LOOP ( 'NONE', ( #43777, #39497, #50926, #13456 ) ) ;
#29624 = ORIENTED_EDGE ( 'NONE', *, *, #9663, .T. ) ;
#29625 = DIRECTION ( 'NONE',  ( 0.000000000000000000, -1.000000000000000000, 0.000000000000000000 ) ) ;
#29626 = ORIENTED_EDGE ( 'NONE', *, *, #22472, .T. ) ;
#29627 = PLANE ( 'NONE',  #16364 ) ;
#29628 = CARTESIAN_POINT ( 'NONE',  ( 1.306513359544259956, 1.663211357094787957, -1.881986840193734967 ) ) ;
#29629 = VECTOR ( 'NONE', #49396, 39.37007874015748143 ) ;
#29630 = EDGE_CURVE ( 'NONE', #10321, #32755, #21751, .T. ) ;
#29631 = LINE ( 'NONE', #1240, #19769 ) ;
#29632 = AXIS2_PLACEMENT_3D ( 'NONE', #8631, #47828, #48085 ) ;
#29633 = ORIENTED_EDGE ( 'NONE', *, *, #31340, .F. ) ;
#29634 = ADVANCED_FACE ( 'NONE', ( #30775 ), #34939, .T. ) ;
#29635 = PLANE ( 'NONE',  #22003 ) ;
#29636 = DIRECTION ( 'NONE',  ( -3.469446951953613696E-16, 0.000000000000000000, -1.000000000000000000 ) ) ;
#29637 = ORIENTED_EDGE ( 'NONE', *, *, #17981, .T. ) ;
#29638 = CARTESIAN_POINT ( 'NONE',  ( 0.000000000000000000, 10.31496062992126284, 0.000000000000000000 ) ) ;
#29639 = DIRECTION ( 'NONE',  ( 0.000000000000000000, 0.000000000000000000, 1.000000000000000000 ) ) ;
#29640 = CIRCLE ( 'NONE', #43651, 2.165354330708661568 ) ;
#29641 = LINE ( 'NONE', #37906, #2945 ) ;
#29642 = DIRECTION ( 'NONE',  ( 0.000000000000000000, 1.160734090543304660E-16, -1.000000000000000000 ) ) ;
#29643 = EDGE_CURVE ( 'NONE', #29652, #19240, #30577, .T. ) ;
#29644 = DIRECTION ( 'NONE',  ( 0.01601477604151182663, -0.9998717552508123996, 0.000000000000000000 ) ) ;
#29645 = CARTESIAN_POINT ( 'NONE',  ( 1.558105373646058167, 3.346456692913386100, -1.417322834645665219 ) ) ;
#29646 = EDGE_LOOP ( 'NONE', ( #18679, #37973, #7521, #24773 ) ) ;
#29647 = CARTESIAN_POINT ( 'NONE',  ( 2.106197740627112402, 3.346456692913386100, 0.7874015748031456541 ) ) ;
#29648 = CARTESIAN_POINT ( 'NONE',  ( 0.000000000000000000, 3.313179664429866556, 0.000000000000000000 ) ) ;
#29649 = ORIENTED_EDGE ( 'NONE', *, *, #35228, .F. ) ;
#29650 = DIRECTION ( 'NONE',  ( 0.000000000000000000, 1.000000000000000000, 0.000000000000000000 ) ) ;
#29651 = EDGE_CURVE ( 'NONE', #30246, #49658, #22778, .T. ) ;
#29652 = VERTEX_POINT ( 'NONE', #15026 ) ;
#29653 = LINE ( 'NONE', #21398, #41821 ) ;
#29654 = CARTESIAN_POINT ( 'NONE',  ( 0.5455278134075216556, 3.346456692913386100, 2.034427629037600660 ) ) ;
#29655 = CARTESIAN_POINT ( 'NONE',  ( -0.3818873615803586308, 0.007309285104348540660, 1.828759827582272068 ) ) ;
#29656 = EDGE_CURVE ( 'NONE', #606, #26629, #27903, .T. ) ;
#29657 = PLANE ( 'NONE',  #20137 ) ;
#29658 = FACE_BOUND ( 'NONE', #22975, .T. ) ;
#29659 = VECTOR ( 'NONE', #42550, 39.37007874015748854 ) ;
#29660 = EDGE_LOOP ( 'NONE', ( #16302, #23436, #32663, #25770 ) ) ;
#29661 = EDGE_CURVE ( 'NONE', #42568, #43159, #31793, .T. ) ;
#29662 = LINE ( 'NONE', #25780, #42192 ) ;
#29663 = ORIENTED_EDGE ( 'NONE', *, *, #40368, .T. ) ;
#29664 = VERTEX_POINT ( 'NONE', #42882 ) ;
#29665 = CARTESIAN_POINT ( 'NONE',  ( 0.2727639067037609943, 3.346456692913386100, 1.220472440944875281 ) ) ;
#29666 = EDGE_CURVE ( 'NONE', #15435, #1405, #39275, .T. ) ;
#29667 = EDGE_LOOP ( 'NONE', ( #48151, #19176, #19804, #44387 ) ) ;
#29668 = DIRECTION ( 'NONE',  ( 1.000000000000000000, 0.000000000000000000, 0.000000000000000000 ) ) ;
#29669 = DIRECTION ( 'NONE',  ( -0.7071067811865483499, -0.000000000000000000, 0.7071067811865466846 ) ) ;
#29670 = EDGE_CURVE ( 'NONE', #17533, #10321, #23269, .T. ) ;
#29671 = ORIENTED_EDGE ( 'NONE', *, *, #41891, .T. ) ;
#29672 = DIRECTION ( 'NONE',  ( 0.7227948638273880011, 0.000000000000000000, 0.6910626489868685329 ) ) ;
#29673 = B_SPLINE_CURVE_WITH_KNOTS ( 'NONE', 3,
 ( #23993, #15992, #34856, #50540 ),
 .UNSPECIFIED., .F., .F.,
 ( 4, 4 ),
 ( 0.001225133028562884257, 0.003725407075890712141 ),
 .UNSPECIFIED. ) ;
#29674 = DIRECTION ( 'NONE',  ( 1.000000000000000000, 0.000000000000000000, 0.000000000000000000 ) ) ;
#29675 = CARTESIAN_POINT ( 'NONE',  ( 1.833433833923350909, 3.267716535433071279, -6.361001426713997494E-16 ) ) ;
#29676 = VERTEX_POINT ( 'NONE', #12419 ) ;
#29677 = ORIENTED_EDGE ( 'NONE', *, *, #13706, .F. ) ;
#29678 = CARTESIAN_POINT ( 'NONE',  ( 0.1525302393087137887, 1.710345001767278994, -2.243756654240526505 ) ) ;
#29679 = FACE_BOUND ( 'NONE', #26040, .T. ) ;
#29680 = VERTEX_POINT ( 'NONE', #50582 ) ;
#29681 = VECTOR ( 'NONE', #47254, 39.37007874015748143 ) ;
#29682 = CARTESIAN_POINT ( 'NONE',  ( 0.8182917201112817063, 0.000000000000000000, -1.732283464566923614 ) ) ;
#29683 = CARTESIAN_POINT ( 'NONE',  ( -0.3486774197067340486, 3.346456692913386100, -2.077238655036873549 ) ) ;
#29684 = ORIENTED_EDGE ( 'NONE', *, *, #2217, .F. ) ;
#29685 = VERTEX_POINT ( 'NONE', #11905 ) ;
#29686 = CARTESIAN_POINT ( 'NONE',  ( -1.985260859929297794, 0.000000000000000000, 0.4330708661417290162 ) ) ;
#29687 = DIRECTION ( 'NONE',  ( -0.000000000000000000, 1.000000000000000000, -0.000000000000000000 ) ) ;
#29688 = VERTEX_POINT ( 'NONE', #15277 ) ;
#29689 = EDGE_LOOP ( 'NONE', ( #47702, #21308, #33723, #38549 ) ) ;
#29690 = ORIENTED_EDGE ( 'NONE', *, *, #45117, .T. ) ;
#29691 = CARTESIAN_POINT ( 'NONE',  ( 0.000000000000000000, 0.07874015748031502893, 0.000000000000000000 ) ) ;
#29692 = PLANE ( 'NONE',  #44761 ) ;
#29693 = CARTESIAN_POINT ( 'NONE',  ( -0.2134117707794043750, 0.02450148541315291459, -1.822192086320855164 ) ) ;
#29694 = CARTESIAN_POINT ( 'NONE',  ( 1.909347346926324684, 3.346456692913386100, -0.3543307086614178592 ) ) ;
#29695 = VERTEX_POINT ( 'NONE', #8033 ) ;
#29696 = EDGE_LOOP ( 'NONE', ( #27418, #34734, #36204, #18691 ) ) ;
#29697 = EDGE_CURVE ( 'NONE', #1162, #5904, #4165, .T. ) ;
#29698 = LINE ( 'NONE', #18591, #46368 ) ;
#29699 =( NAMED_UNIT ( * ) SI_UNIT ( $, .STERADIAN. ) SOLID_ANGLE_UNIT ( ) );
#29700 = EDGE_CURVE ( 'NONE', #42296, #33123, #11651, .T. ) ;
#29701 = DIRECTION ( 'NONE',  ( -0.000000000000000000, 1.000000000000000000, -0.000000000000000000 ) ) ;
#29702 = CARTESIAN_POINT ( 'NONE',  ( -0.6214413264104939882, 3.346456692913386100, 0.7874015748031456541 ) ) ;
#29703 = EDGE_CURVE ( 'NONE', #30894, #49397, #47493, .T. ) ;
#29704 = CARTESIAN_POINT ( 'NONE',  ( 0.000000000000000000, 3.267716535433071279, -1.771653543307081691 ) ) ;
#29705 = AXIS2_PLACEMENT_3D ( 'NONE', #41756, #2005, #33521 ) ;
#29706 = AXIS2_PLACEMENT_3D ( 'NONE', #44214, #28721, #20985 ) ;
#29707 = LINE ( 'NONE', #14464, #44098 ) ;
#29708 = CARTESIAN_POINT ( 'NONE',  ( 3.616083068348484413E-16, 0.000000000000000000, 2.952755905511811552 ) ) ;
#29709 = VERTEX_POINT ( 'NONE', #35660 ) ;
#29710 = CARTESIAN_POINT ( 'NONE',  ( 1.636583440222563857, 3.346456692913386100, -0.1968503937007886062 ) ) ;
#29711 = CARTESIAN_POINT ( 'NONE',  ( 0.000000000000000000, 2.755905511811027164, 0.000000000000000000 ) ) ;
#29712 = CONICAL_SURFACE ( 'NONE', #23106, 3.033577403570480779, 1.554780866114618743 ) ;
#29713 = ORIENTED_EDGE ( 'NONE', *, *, #7676, .F. ) ;
#29714 = ORIENTED_EDGE ( 'NONE', *, *, #35823, .T. ) ;
#29715 = LINE ( 'NONE', #9842, #17944 ) ;
#29716 = EDGE_CURVE ( 'NONE', #30486, #17428, #39786, .T. ) ;
#29717 = VERTEX_POINT ( 'NONE', #31285 ) ;
#29718 = EDGE_CURVE ( 'NONE', #25537, #2388, #19891, .T. ) ;
#29719 = ORIENTED_EDGE ( 'NONE', *, *, #334, .F. ) ;
#29720 = LINE ( 'NONE', #22480, #36969 ) ;
#29721 = ORIENTED_EDGE ( 'NONE', *, *, #13060, .F. ) ;
#29722 = CARTESIAN_POINT ( 'NONE',  ( 0.1968503937007872184, 3.267716535433071279, -6.829619984160650651E-17 ) ) ;
#29723 = CARTESIAN_POINT ( 'NONE',  ( 0.5455278134075212115, 0.000000000000000000, 0.3149606299212576177 ) ) ;
#29724 = ORIENTED_EDGE ( 'NONE', *, *, #820, .T. ) ;
#29725 = VERTEX_POINT ( 'NONE', #24302 ) ;
#29726 = CARTESIAN_POINT ( 'NONE',  ( -1.477691947303356290, 1.684234009953186728, 1.616556376299586706 ) ) ;
#29727 = EDGE_LOOP ( 'NONE', ( #27180, #442, #36529, #9070 ) ) ;
#29728 = ORIENTED_EDGE ( 'NONE', *, *, #28097, .T. ) ;
#29729 = CARTESIAN_POINT ( 'NONE',  ( -0.8368120681608454126, 0.004905009409801163595, -1.624234696386792631 ) ) ;
#29730 = DIRECTION ( 'NONE',  ( -0.000000000000000000, 1.000000000000000000, -0.000000000000000000 ) ) ;
#29731 = PLANE ( 'NONE',  #30151 ) ;
#29732 = EDGE_CURVE ( 'NONE', #33442, #19657, #3403, .T. ) ;
#29733 = VECTOR ( 'NONE', #545, 39.37007874015748143 ) ;
#29734 = ORIENTED_EDGE ( 'NONE', *, *, #14763, .F. ) ;
#29735 = CIRCLE ( 'NONE', #42111, 2.165354330708661568 ) ;
#29736 = DIRECTION ( 'NONE',  ( -0.000000000000000000, 1.000000000000000000, -0.000000000000000000 ) ) ;
#29737 = CARTESIAN_POINT ( 'NONE',  ( -4.268512490100411402E-16, 0.000000000000000000, -2.086614173228339641 ) ) ;
#29738 = CARTESIAN_POINT ( 'NONE',  ( -0.2727639067037608278, 3.267716535433071279, 4.731699523581614055E-17 ) ) ;
#29739 = ORIENTED_EDGE ( 'NONE', *, *, #44122, .F. ) ;
#29740 = DIRECTION ( 'NONE',  ( -1.000000000000000000, 0.000000000000000000, -0.000000000000000000 ) ) ;
#29741 = CARTESIAN_POINT ( 'NONE',  ( -2.623503965249869729, 1.678368413758691391, 1.355882097269835107 ) ) ;
#29742 = CARTESIAN_POINT ( 'NONE',  ( -1.281152772984899491, 0.000000000000000000, -2.660341145381166506 ) ) ;
#29743 = ORIENTED_EDGE ( 'NONE', *, *, #6815, .T. ) ;
#29744 = ORIENTED_EDGE ( 'NONE', *, *, #28158, .F. ) ;
#29745 = AXIS2_PLACEMENT_3D ( 'NONE', #38872, #7881, #39631 ) ;
#29746 = DIRECTION ( 'NONE',  ( 1.000000000000000000, 0.000000000000000000, 0.000000000000000000 ) ) ;
#29747 =( BOUNDED_CURVE ( )  B_SPLINE_CURVE ( 3, ( #42914, #7815, #11942, #22551 ),
 .UNSPECIFIED., .F., .F. ) 
 B_SPLINE_CURVE_WITH_KNOTS ( ( 4, 4 ),
 ( 1.467165271168491936, 1.518105237349054670 ),
 .UNSPECIFIED. ) 
 CURVE ( )  GEOMETRIC_REPRESENTATION_ITEM ( )  RATIONAL_B_SPLINE_CURVE ( ( 1.000000000000000000, 0.9997837716768099847, 0.9997837716768099847, 1.000000000000000000 ) ) 
 REPRESENTATION_ITEM ( '' )  );
#29748 = B_SPLINE_CURVE_WITH_KNOTS ( 'NONE', 3,
 ( #6786, #6542, #50102, #10909 ),
 .UNSPECIFIED., .F., .F.,
 ( 4, 4 ),
 ( 2.008297436534455258E-07, 0.01816780577132326782 ),
 .UNSPECIFIED. ) ;
#29749 = LINE ( 'NONE', #25619, #19515 ) ;
#29750 = DIRECTION ( 'NONE',  ( -0.000000000000000000, 1.000000000000000000, -0.000000000000000000 ) ) ;
#29751 = ORIENTED_EDGE ( 'NONE', *, *, #5959, .T. ) ;
#29752 = VERTEX_POINT ( 'NONE', #27142 ) ;
#29753 = EDGE_CURVE ( 'NONE', #50330, #3427, #6936, .T. ) ;
#29754 = DIRECTION ( 'NONE',  ( 0.000000000000000000, -1.000000000000000000, 0.000000000000000000 ) ) ;
#29755 = EDGE_LOOP ( 'NONE', ( #45176, #34430, #7068, #8362 ) ) ;
#29756 = DIRECTION ( 'NONE',  ( -3.469446951953613696E-16, 0.000000000000000000, -1.000000000000000000 ) ) ;
#29757 = LINE ( 'NONE', #45475, #8614 ) ;
#29758 = EDGE_CURVE ( 'NONE', #8254, #28950, #47231, .T. ) ;
#29759 = EDGE_CURVE ( 'NONE', #44082, #15287, #49742, .T. ) ;
#29760 = EDGE_CURVE ( 'NONE', #18530, #3406, #11404, .T. ) ;
#29761 = DIRECTION ( 'NONE',  ( 1.734723475976806848E-16, 0.000000000000000000, 1.000000000000000000 ) ) ;
#29762 = DIRECTION ( 'NONE',  ( -0.000000000000000000, 1.000000000000000000, -0.000000000000000000 ) ) ;
#29763 = DIRECTION ( 'NONE',  ( 0.000000000000000000, -0.000000000000000000, -1.000000000000000000 ) ) ;
#29764 = ORIENTED_EDGE ( 'NONE', *, *, #42008, .F. ) ;
#29765 = DIRECTION ( 'NONE',  ( -0.000000000000000000, 1.000000000000000000, -0.000000000000000000 ) ) ;
#29766 = DIRECTION ( 'NONE',  ( -3.469446951953613696E-16, 0.000000000000000000, -1.000000000000000000 ) ) ;
#29767 = DIRECTION ( 'NONE',  ( -3.469446951953613696E-16, 0.000000000000000000, -1.000000000000000000 ) ) ;
#29768 = CIRCLE ( 'NONE', #33907, 2.244934639244525076 ) ;
#29769 = ORIENTED_EDGE ( 'NONE', *, *, #26281, .F. ) ;
#29770 = CARTESIAN_POINT ( 'NONE',  ( -0.8182917201112819283, 3.267716535433071279, -0.4724409448818886470 ) ) ;
#29771 = AXIS2_PLACEMENT_3D ( 'NONE', #12448, #4452, #16328 ) ;
#29772 = DIRECTION ( 'NONE',  ( 1.734723475976806848E-16, -0.000000000000000000, 1.000000000000000000 ) ) ;
#29773 = ADVANCED_FACE ( 'NONE', ( #15533 ), #46979, .F. ) ;
#29774 = FACE_OUTER_BOUND ( 'NONE', #27760, .T. ) ;
#29775 = EDGE_LOOP ( 'NONE', ( #13596, #40934, #7679, #34581 ) ) ;
#29776 = DIRECTION ( 'NONE',  ( 0.000000000000000000, 1.000000000000000000, -0.000000000000000000 ) ) ;
#29777 = EDGE_CURVE ( 'NONE', #16605, #20587, #24252, .T. ) ;
#29778 = ORIENTED_EDGE ( 'NONE', *, *, #49695, .F. ) ;
#29779 = DIRECTION ( 'NONE',  ( 0.000000000000000000, 1.000000000000000000, 0.000000000000000000 ) ) ;
#29780 = VECTOR ( 'NONE', #23240, 39.37007874015748143 ) ;
#29781 = CARTESIAN_POINT ( 'NONE',  ( 0.5455278134075212115, 0.000000000000000000, -0.6299212598425181220 ) ) ;
#29782 = VERTEX_POINT ( 'NONE', #35411 ) ;
#29783 = DIRECTION ( 'NONE',  ( 1.000000000000000000, 0.000000000000000000, -3.469446951953613696E-16 ) ) ;
#29784 = CIRCLE ( 'NONE', #30635, 2.165354330708661568 ) ;
#29785 = CARTESIAN_POINT ( 'NONE',  ( -1.363819533518803473, 3.346456692913386100, 1.850393700787392293 ) ) ;
#29786 = CARTESIAN_POINT ( 'NONE',  ( 2.106197740627112402, 0.000000000000000000, -0.4724409448818889246 ) ) ;
#29787 = FACE_OUTER_BOUND ( 'NONE', #10575, .T. ) ;
#29788 = EDGE_CURVE ( 'NONE', #41228, #23992, #28, .T. ) ;
#29789 = CARTESIAN_POINT ( 'NONE',  ( 1.109524193798303804, 0.000000000000000000, 1.344750771968474590 ) ) ;
#29790 = ORIENTED_EDGE ( 'NONE', *, *, #16295, .T. ) ;
#29791 = ORIENTED_EDGE ( 'NONE', *, *, #43956, .T. ) ;
#29792 = CARTESIAN_POINT ( 'NONE',  ( 1.091055626815042645, 3.346456692913386100, -1.141732283464564013 ) ) ;
#29793 = CARTESIAN_POINT ( 'NONE',  ( 1.363819533518803251, 3.346456692913386100, -0.3543307086614178592 ) ) ;
#29794 = ORIENTED_EDGE ( 'NONE', *, *, #25695, .T. ) ;
#29795 = LINE ( 'NONE', #9925, #7763 ) ;
#29796 = CARTESIAN_POINT ( 'NONE',  ( 1.015142113812069091, 3.346456692913386100, -2.244094488188969283 ) ) ;
#29797 = CARTESIAN_POINT ( 'NONE',  ( 0.000000000000000000, 3.267716535433071279, -0.8267716535433049518 ) ) ;
#29798 = ADVANCED_FACE ( 'NONE', ( #17327 ), #33343, .F. ) ;
#29799 = ORIENTED_EDGE ( 'NONE', *, *, #36596, .T. ) ;
#29800 = ORIENTED_EDGE ( 'NONE', *, *, #25140, .F. ) ;
#29801 = DIRECTION ( 'NONE',  ( 1.734723475976806848E-16, 0.000000000000000000, 1.000000000000000000 ) ) ;
#29802 = DIRECTION ( 'NONE',  ( 5.500355109725808462E-17, -1.000000000000000000, -1.022137253806221654E-16 ) ) ;
#29803 = DIRECTION ( 'NONE',  ( -1.858431260983764056E-16, -0.7660444431189770143, 0.6427876096865403621 ) ) ;
#29804 = ORIENTED_EDGE ( 'NONE', *, *, #11732, .F. ) ;
#29805 = DIRECTION ( 'NONE',  ( 0.000000000000000000, -1.000000000000000000, 0.000000000000000000 ) ) ;
#29806 = CARTESIAN_POINT ( 'NONE',  ( 1.091055626815043311, 3.346456692913386100, 1.889763779527550369 ) ) ;
#29807 = VERTEX_POINT ( 'NONE', #21453 ) ;
#29808 = ADVANCED_FACE ( 'NONE', ( #49022 ), #9575, .F. ) ;
#29809 = CARTESIAN_POINT ( 'NONE',  ( -1.363819533518803251, 3.267716535433071279, 2.365849761790805487E-16 ) ) ;
#29810 = EDGE_LOOP ( 'NONE', ( #39139, #9559, #14105 ) ) ;
#29811 = EDGE_LOOP ( 'NONE', ( #16242, #3684, #21805, #42813 ) ) ;
#29812 = DIRECTION ( 'NONE',  ( -1.000000000000000000, 0.000000000000000000, 1.734723475976806848E-16 ) ) ;
#29813 = DIRECTION ( 'NONE',  ( 0.000000000000000000, 0.000000000000000000, -1.000000000000000000 ) ) ;
#29814 = VECTOR ( 'NONE', #26269, 39.37007874015748143 ) ;
#29816 = VECTOR ( 'NONE', #11449, 39.37007874015748143 ) ;
#29815 = PLANE ( 'NONE',  #17358 ) ;
#29817 = ORIENTED_EDGE ( 'NONE', *, *, #30694, .F. ) ;
#29818 = PLANE ( 'NONE',  #48311 ) ;
#29819 = LINE ( 'NONE', #29568, #10652 ) ;
#29820 = B_SPLINE_CURVE_WITH_KNOTS ( 'NONE', 3,
 ( #40782, #20383, #44121, #36138 ),
 .UNSPECIFIED., .F., .F.,
 ( 4, 4 ),
 ( 2.102946038521954085E-07, 0.002500239258116422787 ),
 .UNSPECIFIED. ) ;
#29821 = ORIENTED_EDGE ( 'NONE', *, *, #26258, .F. ) ;
#29822 = VECTOR ( 'NONE', #36272, 39.37007874015748143 ) ;
#29823 = VECTOR ( 'NONE', #41742, 39.37007874015748143 ) ;
#29824 = ORIENTED_EDGE ( 'NONE', *, *, #8413, .F. ) ;
#29825 = CARTESIAN_POINT ( 'NONE',  ( -0.6214413264104945434, 3.346456692913386100, -1.417322834645664331 ) ) ;
#29826 = CARTESIAN_POINT ( 'NONE',  ( -1.636583440222564301, 0.000000000000000000, -0.9448818897637762948 ) ) ;
#29827 = EDGE_CURVE ( 'NONE', #945, #32113, #28412, .T. ) ;
#29828 = AXIS2_PLACEMENT_3D ( 'NONE', #34162, #22031, #30023 ) ;
#29829 = CARTESIAN_POINT ( 'NONE',  ( 2.424495731808704591, 1.651670313967669390, 0.7360212284965905738 ) ) ;
#29830 = EDGE_CURVE ( 'NONE', #23878, #8216, #27446, .T. ) ;
#29831 = LINE ( 'NONE', #37332, #42618 ) ;
#29832 = PLANE ( 'NONE',  #20413 ) ;
#29833 = EDGE_LOOP ( 'NONE', ( #19006, #8274, #12663, #48084 ) ) ;
#29834 = DIRECTION ( 'NONE',  ( -3.469446951953613696E-16, 0.000000000000000000, -1.000000000000000000 ) ) ;
#29835 = CARTESIAN_POINT ( 'NONE',  ( -0.07591351300297277671, 0.000000000000000000, 1.417322834645662777 ) ) ;
#29836 = EDGE_LOOP ( 'NONE', ( #17248, #32345, #45832, #48998, #19223 ) ) ;
#29837 = CARTESIAN_POINT ( 'NONE',  ( 0.000000000000000000, 3.267716535433071279, -1.614173228346452715 ) ) ;
#29838 = CARTESIAN_POINT ( 'NONE',  ( 0.000000000000000000, 1.574803149606302854, 0.000000000000000000 ) ) ;
#29839 = ORIENTED_EDGE ( 'NONE', *, *, #44280, .F. ) ;
#29840 = LINE ( 'NONE', #17454, #18030 ) ;
#29841 = FACE_OUTER_BOUND ( 'NONE', #2695, .T. ) ;
#29842 = CARTESIAN_POINT ( 'NONE',  ( 0.5455278134075216556, 0.000000000000000000, 1.062992125984246083 ) ) ;
#29843 = ORIENTED_EDGE ( 'NONE', *, *, #8600, .T. ) ;
#29844 = LINE ( 'NONE', #1455, #37323 ) ;
#29845 = EDGE_LOOP ( 'NONE', ( #25165, #29452, #32352, #14744, #28819 ) ) ;
#29846 = FACE_BOUND ( 'NONE', #29281, .T. ) ;
#29847 = DIRECTION ( 'NONE',  ( -0.9749279121818259508, 0.000000000000000000, 0.2225209339563041788 ) ) ;
#29848 = AXIS2_PLACEMENT_3D ( 'NONE', #18662, #30278, #34659 ) ;
#29849 = AXIS2_PLACEMENT_3D ( 'NONE', #29487, #41871, #5739 ) ;
#29850 = DIRECTION ( 'NONE',  ( -3.469446951953613696E-16, 0.000000000000000000, -1.000000000000000000 ) ) ;
#29851 = CARTESIAN_POINT ( 'NONE',  ( 0.000000000000000000, 3.267716535433071279, 0.7874015748031456541 ) ) ;
#29852 = EDGE_CURVE ( 'NONE', #7564, #34607, #9063, .T. ) ;
#29853 = AXIS2_PLACEMENT_3D ( 'NONE', #45762, #22303, #46762 ) ;
#29854 = ORIENTED_EDGE ( 'NONE', *, *, #16338, .F. ) ;
#29855 = ORIENTED_EDGE ( 'NONE', *, *, #37798, .F. ) ;
#29856 = CARTESIAN_POINT ( 'NONE',  ( 1.636583440222563857, 3.267716535433071279, -2.839019714148966584E-16 ) ) ;
#29857 = CONICAL_SURFACE ( 'NONE', #14190, 2.244934639244524632, 1.554780866114618743 ) ;
#29858 = CARTESIAN_POINT ( 'NONE',  ( -2.120667608396066051, 0.5253322431346389987, 0.3369259977602169220 ) ) ;
#29859 = VERTEX_POINT ( 'NONE', #33086 ) ;
#29860 = EDGE_CURVE ( 'NONE', #23969, #36096, #29451, .T. ) ;
#29861 = DIRECTION ( 'NONE',  ( 5.500355109725658086E-17, -1.000000000000000000, 1.022137253806229789E-16 ) ) ;
#29862 = VECTOR ( 'NONE', #5194, 39.37007874015748143 ) ;
#29863 = EDGE_CURVE ( 'NONE', #9844, #48933, #45168, .T. ) ;
#29864 = VERTEX_POINT ( 'NONE', #20938 ) ;
#29865 = FACE_OUTER_BOUND ( 'NONE', #39544, .T. ) ;
#29866 = ADVANCED_FACE ( 'NONE', ( #9317 ), #36690, .F. ) ;
#29867 = CARTESIAN_POINT ( 'NONE',  ( 0.1155636338427008941, -0.5222242541845523167, 0.000000000000000000 ) ) ;
#29868 = ORIENTED_EDGE ( 'NONE', *, *, #37927, .T. ) ;
#29869 = EDGE_CURVE ( 'NONE', #22692, #22325, #22593, .T. ) ;
#29870 = CARTESIAN_POINT ( 'NONE',  ( 1.556712866041120247, 1.743522182421873401, 2.509548638715870084 ) ) ;
#29871 = ORIENTED_EDGE ( 'NONE', *, *, #36299, .F. ) ;
#29872 = ORIENTED_EDGE ( 'NONE', *, *, #9062, .T. ) ;
#29873 = EDGE_CURVE ( 'NONE', #46587, #8462, #2809, .T. ) ;
#29874 = EDGE_LOOP ( 'NONE', ( #19932, #29406, #32676, #32261 ) ) ;
#29875 = ORIENTED_EDGE ( 'NONE', *, *, #46799, .F. ) ;
#29876 = LINE ( 'NONE', #21620, #29364 ) ;
#29877 = ORIENTED_EDGE ( 'NONE', *, *, #33209, .T. ) ;
#29878 = CARTESIAN_POINT ( 'NONE',  ( 1.386843392441768241, 1.730114785850798587, -1.825100698618727257 ) ) ;
#29879 = CARTESIAN_POINT ( 'NONE',  ( 0.000000000000000000, 3.267716535433071279, 0.1181102362204701633 ) ) ;
#29880 = EDGE_CURVE ( 'NONE', #7588, #17434, #32835, .T. ) ;
#29881 = VECTOR ( 'NONE', #3577, 39.37007874015748854 ) ;
#29882 = CARTESIAN_POINT ( 'NONE',  ( 1.481515513156649977, 0.000000000000000000, -0.9189724476880527515 ) ) ;
#29883 = EDGE_CURVE ( 'NONE', #706, #8583, #40818, .T. ) ;
#29884 = VECTOR ( 'NONE', #19748, 39.37007874015748143 ) ;
#29885 = CARTESIAN_POINT ( 'NONE',  ( -1.236813753895213086, 1.601547340627394567, -2.681693691597581974 ) ) ;
#29886 = DIRECTION ( 'NONE',  ( 1.000000000000000000, 0.000000000000000000, 0.000000000000000000 ) ) ;
#29887 = EDGE_CURVE ( 'NONE', #39537, #13500, #39915, .T. ) ;
#29888 = ORIENTED_EDGE ( 'NONE', *, *, #4644, .F. ) ;
#29889 = DIRECTION ( 'NONE',  ( 1.734723475976806848E-16, -0.000000000000000000, 1.000000000000000000 ) ) ;
#29890 = LINE ( 'NONE', #18264, #24180 ) ;
#29891 = VECTOR ( 'NONE', #25016, 39.37007874015748143 ) ;
#29892 = LINE ( 'NONE', #45357, #7031 ) ;
#29893 = CARTESIAN_POINT ( 'NONE',  ( 0.000000000000000000, 1.574803149606302854, 0.000000000000000000 ) ) ;
#29894 = AXIS2_PLACEMENT_3D ( 'NONE', #15023, #6770, #6267 ) ;
#29895 = VECTOR ( 'NONE', #1046, 39.37007874015748143 ) ;
#29896 = ORIENTED_EDGE ( 'NONE', *, *, #38424, .F. ) ;
#29897 = FACE_OUTER_BOUND ( 'NONE', #9229, .T. ) ;
#29898 = LINE ( 'NONE', #45107, #17062 ) ;
#29899 = ORIENTED_EDGE ( 'NONE', *, *, #28535, .T. ) ;
#29900 = DIRECTION ( 'NONE',  ( -0.000000000000000000, 1.000000000000000000, -0.000000000000000000 ) ) ;
#29901 = DIRECTION ( 'NONE',  ( -1.000000000000000000, 0.000000000000000000, -0.000000000000000000 ) ) ;
#29902 = ORIENTED_EDGE ( 'NONE', *, *, #10507, .F. ) ;
#29903 = ORIENTED_EDGE ( 'NONE', *, *, #3588, .T. ) ;
#29904 = LINE ( 'NONE', #27026, #2542 ) ;
#29905 = FACE_OUTER_BOUND ( 'NONE', #26997, .T. ) ;
#29906 = CARTESIAN_POINT ( 'NONE',  ( 0.000000000000000000, 0.000000000000000000, 0.000000000000000000 ) ) ;
#29907 = CARTESIAN_POINT ( 'NONE',  ( -2.659291275338656391, 1.673716702457430650, 0.4098875308770844605 ) ) ;
#29908 = CARTESIAN_POINT ( 'NONE',  ( 1.971247363764867977, 5.905511811023623991, -0.8960709840011632510 ) ) ;
#29909 = ORIENTED_EDGE ( 'NONE', *, *, #3758, .T. ) ;
#29910 = CARTESIAN_POINT ( 'NONE',  ( 2.182111253630085290, 3.346456692913386100, -0.3149606299212596716 ) ) ;
#29911 = ORIENTED_EDGE ( 'NONE', *, *, #44479, .T. ) ;
#29912 = ORIENTED_EDGE ( 'NONE', *, *, #39296, .T. ) ;
#29913 = CARTESIAN_POINT ( 'NONE',  ( 0.8182917201112819283, 3.346456692913386100, 1.102362204724403938 ) ) ;
#29914 = ORIENTED_EDGE ( 'NONE', *, *, #27974, .T. ) ;
#29915 = LINE ( 'NONE', #6931, #8955 ) ;
#29916 = CARTESIAN_POINT ( 'NONE',  ( 1.287906020515830141, 3.267716535433071279, -0.5118110236220471121 ) ) ;
#29917 = EDGE_LOOP ( 'NONE', ( #17601, #21712, #37122 ) ) ;
#29918 = CARTESIAN_POINT ( 'NONE',  ( -2.793030215715272213, 1.205361022782829114E-17, 0.9592557174602285297 ) ) ;
#29919 = ADVANCED_FACE ( 'NONE', ( #44161 ), #40310, .F. ) ;
#29920 = DIRECTION ( 'NONE',  ( -0.01601477604151182663, 0.9998717552508123996, -0.000000000000000000 ) ) ;
#29921 = EDGE_CURVE ( 'NONE', #16323, #6701, #1574, .T. ) ;
#29922 = ADVANCED_FACE ( 'NONE', ( #16812 ), #48769, .F. ) ;
#29923 = VECTOR ( 'NONE', #36540, 39.37007874015748143 ) ;
#29924 = DIRECTION ( 'NONE',  ( -0.08963930890342654279, 0.000000000000000000, -0.9959742939952397345 ) ) ;
#29925 = ORIENTED_EDGE ( 'NONE', *, *, #45397, .T. ) ;
#29926 = EDGE_LOOP ( 'NONE', ( #3087, #45052, #47381, #49977 ) ) ;
#29927 = CARTESIAN_POINT ( 'NONE',  ( -1.636583440222564301, 3.346456692913386100, -1.259842519685034468 ) ) ;
#29928 = FACE_BOUND ( 'NONE', #31583, .T. ) ;
#29929 = VERTEX_POINT ( 'NONE', #1825 ) ;
#29930 = AXIS2_PLACEMENT_3D ( 'NONE', #44146, #8789, #24538 ) ;
#29931 = VECTOR ( 'NONE', #6466, 39.37007874015748143 ) ;
#29932 = DIRECTION ( 'NONE',  ( 1.000000000000000000, -0.000000000000000000, 0.000000000000000000 ) ) ;
#29933 = DIRECTION ( 'NONE',  ( -3.986037398843765983E-20, -1.000000000000000000, -1.160734090543304660E-16 ) ) ;
#29934 = VERTEX_POINT ( 'NONE', #17576 ) ;
#29935 = VERTEX_POINT ( 'NONE', #30472 ) ;
#29936 = CARTESIAN_POINT ( 'NONE',  ( -1.166969139818015977, 0.000000000000000000, 2.047244094488179567 ) ) ;
#29937 = VECTOR ( 'NONE', #27267, 39.37007874015748143 ) ;
#29938 = CARTESIAN_POINT ( 'NONE',  ( 0.000000000000000000, 1.574803149606302854, 0.000000000000000000 ) ) ;
#29939 = ORIENTED_EDGE ( 'NONE', *, *, #9976, .F. ) ;
#29940 = ORIENTED_EDGE ( 'NONE', *, *, #14695, .T. ) ;
#29941 = ADVANCED_FACE ( 'NONE', ( #29959 ), #10842, .F. ) ;
#29942 = ORIENTED_EDGE ( 'NONE', *, *, #26416, .F. ) ;
#29943 = LINE ( 'NONE', #41560, #35924 ) ;
#29944 = CARTESIAN_POINT ( 'NONE',  ( 4.268512490100411402E-16, 0.000000000000000000, 2.204724409448808764 ) ) ;
#29945 = EDGE_CURVE ( 'NONE', #3065, #13301, #42324, .T. ) ;
#29946 = LINE ( 'NONE', #2327, #49774 ) ;
#29947 = DIRECTION ( 'NONE',  ( -3.469446951953613696E-16, 0.000000000000000000, -1.000000000000000000 ) ) ;
#29948 = EDGE_CURVE ( 'NONE', #46776, #5726, #10087, .T. ) ;
#29949 = ORIENTED_EDGE ( 'NONE', *, *, #39245, .T. ) ;
#29950 = ORIENTED_EDGE ( 'NONE', *, *, #28652, .F. ) ;
#29951 = DIRECTION ( 'NONE',  ( 1.734723475976806848E-16, -0.000000000000000000, 1.000000000000000000 ) ) ;
#29952 = PLANE ( 'NONE',  #24666 ) ;
#29953 = EDGE_CURVE ( 'NONE', #12349, #38065, #30720, .T. ) ;
#29954 = EDGE_CURVE ( 'NONE', #47540, #1516, #22718, .T. ) ;
#29955 = DIRECTION ( 'NONE',  ( -0.000000000000000000, 1.000000000000000000, -0.000000000000000000 ) ) ;
#29956 = DIRECTION ( 'NONE',  ( 0.000000000000000000, 1.000000000000000000, 0.000000000000000000 ) ) ;
#29957 = LINE ( 'NONE', #45166, #16577 ) ;
#29958 = CARTESIAN_POINT ( 'NONE',  ( 0.002207914879453961535, -5.712274067634378313E-18, 0.04916304461325374242 ) ) ;
#29959 = FACE_OUTER_BOUND ( 'NONE', #28020, .T. ) ;
#29960 = AXIS2_PLACEMENT_3D ( 'NONE', #20391, #15508, #40282 ) ;
#29961 = VERTEX_POINT ( 'NONE', #29708 ) ;
#29962 = CARTESIAN_POINT ( 'NONE',  ( 0.4696143004045479352, 0.000000000000000000, 0.4724409448818868706 ) ) ;
#29963 = LINE ( 'NONE', #26835, #31018 ) ;
#29964 = VECTOR ( 'NONE', #7609, 39.37007874015748143 ) ;
#29965 = EDGE_LOOP ( 'NONE', ( #22197, #33598, #22277, #31077 ) ) ;
#29966 = VECTOR ( 'NONE', #25365, 39.37007874015748143 ) ;
#29967 = VERTEX_POINT ( 'NONE', #18598 ) ;
#29968 = FACE_OUTER_BOUND ( 'NONE', #35337, .T. ) ;
#29969 = ORIENTED_EDGE ( 'NONE', *, *, #50798, .T. ) ;
#29970 = VECTOR ( 'NONE', #10403, 39.37007874015748143 ) ;
#29971 = ORIENTED_EDGE ( 'NONE', *, *, #24832, .T. ) ;
#29972 = CARTESIAN_POINT ( 'NONE',  ( 1.015142113812069091, 3.267716535433071279, -1.929133858267711110 ) ) ;
#29973 = EDGE_LOOP ( 'NONE', ( #37605, #15546, #2250, #3232 ) ) ;
#29974 = LINE ( 'NONE', #6989, #26016 ) ;
#29975 = CARTESIAN_POINT ( 'NONE',  ( 0.1968503937007873017, 3.267716535433071279, 0.3149606299212576177 ) ) ;
#29976 = VERTEX_POINT ( 'NONE', #42085 ) ;
#29977 = EDGE_CURVE ( 'NONE', #26751, #42980, #45424, .T. ) ;
#29978 = VERTEX_POINT ( 'NONE', #38475 ) ;
#29979 = DIRECTION ( 'NONE',  ( 1.734723475976806848E-16, 0.000000000000000000, 1.000000000000000000 ) ) ;
#29980 = EDGE_CURVE ( 'NONE', #45076, #47505, #21788, .T. ) ;
#29981 = ORIENTED_EDGE ( 'NONE', *, *, #4158, .F. ) ;
#29982 = ORIENTED_EDGE ( 'NONE', *, *, #2347, .T. ) ;
#29983 = PLANE ( 'NONE',  #18240 ) ;
#29984 = CARTESIAN_POINT ( 'NONE',  ( 1.271755610052043295, 3.267716535433071279, -2.086614173228339641 ) ) ;
#29985 = CARTESIAN_POINT ( 'NONE',  ( 2.919426793319799707, 1.764751637901927905, 0.4451252810446822417 ) ) ;
#29986 = CARTESIAN_POINT ( 'NONE',  ( 0.8182917201112819283, 0.000000000000000000, 0.7874015748031454320 ) ) ;
#29987 = EDGE_CURVE ( 'NONE', #49734, #29198, #14973, .T. ) ;
#29988 = ORIENTED_EDGE ( 'NONE', *, *, #32580, .T. ) ;
#29989 = PLANE ( 'NONE',  #8139 ) ;
#29990 = CARTESIAN_POINT ( 'NONE',  ( 1.955086072707955314, 1.749719979519482882, 2.212843190799998805 ) ) ;
#29991 = DIRECTION ( 'NONE',  ( 1.000000000000000000, 0.000000000000000000, 0.000000000000000000 ) ) ;
#29992 = VERTEX_POINT ( 'NONE', #17829 ) ;
#29993 = CYLINDRICAL_SURFACE ( 'NONE', #29849, 2.165354330708661568 ) ;
#29994 = CIRCLE ( 'NONE', #44826, 2.165354330708661568 ) ;
#29995 = DIRECTION ( 'NONE',  ( -1.000000000000000000, -0.000000000000000000, -0.000000000000000000 ) ) ;
#29996 = CARTESIAN_POINT ( 'NONE',  ( 0.8182917201112817063, 0.000000000000000000, -1.929133858267711110 ) ) ;
#29997 = EDGE_LOOP ( 'NONE', ( #21648, #7270, #25342, #15947 ) ) ;
#29998 = VECTOR ( 'NONE', #7731, 39.37007874015748143 ) ;
#29999 = ORIENTED_EDGE ( 'NONE', *, *, #21569, .F. ) ;
#30000 = AXIS2_PLACEMENT_3D ( 'NONE', #39203, #43318, #27574 ) ;
#30001 = AXIS2_PLACEMENT_3D ( 'NONE', #35608, #47435, #12111 ) ;
#30002 = DIRECTION ( 'NONE',  ( 1.000000000000000000, 0.000000000000000000, -3.469446951953613696E-16 ) ) ;
#30003 = EDGE_CURVE ( 'NONE', #19400, #16457, #6471, .T. ) ;
#30004 = LINE ( 'NONE', #46476, #25315 ) ;
#30005 = B_SPLINE_CURVE_WITH_KNOTS ( 'NONE', 3,
 ( #33524, #42011, #45858, #6648 ),
 .UNSPECIFIED., .F., .F.,
 ( 4, 4 ),
 ( 0.01377987572523645989, 0.03074485555701141071 ),
 .UNSPECIFIED. ) ;
#30006 = LINE ( 'NONE', #41881, #12338 ) ;
#30007 = ORIENTED_EDGE ( 'NONE', *, *, #5033, .T. ) ;
#30008 = EDGE_LOOP ( 'NONE', ( #5724, #39954, #40698, #7728 ) ) ;
#30009 = AXIS2_PLACEMENT_3D ( 'NONE', #44165, #4424, #24042 ) ;
#30010 = ADVANCED_FACE ( 'NONE', ( #34093 ), #21966, .F. ) ;
#30011 = DIRECTION ( 'NONE',  ( -0.000000000000000000, 1.000000000000000000, -0.000000000000000000 ) ) ;
#30012 = VERTEX_POINT ( 'NONE', #18848 ) ;
#30013 = CARTESIAN_POINT ( 'NONE',  ( -1.712496953225537633, 3.346456692913386100, -0.6692913385826758654 ) ) ;
#30014 = DIRECTION ( 'NONE',  ( 0.5128992774058948045, 0.000000000000000000, 0.8584487936018727616 ) ) ;
#30015 = CARTESIAN_POINT ( 'NONE',  ( -1.014069264286641570, 0.5905511811023621549, -1.062992125984252301 ) ) ;
#30016 = LINE ( 'NONE', #27143, #19469 ) ;
#30017 = CARTESIAN_POINT ( 'NONE',  ( -1.500395101971645273, 1.546412888404644637, 2.543196936333195435 ) ) ;
#30018 = VERTEX_POINT ( 'NONE', #41836 ) ;
#30019 = DIRECTION ( 'NONE',  ( 1.734723475976806848E-16, -0.000000000000000000, 1.000000000000000000 ) ) ;
#30020 = LINE ( 'NONE', #20556, #31841 ) ;
#30021 = CARTESIAN_POINT ( 'NONE',  ( -2.318790890269176064, 1.563058755309824299, 1.828180962769875739 ) ) ;
#30022 = ORIENTED_EDGE ( 'NONE', *, *, #38861, .F. ) ;
#30023 = DIRECTION ( 'NONE',  ( 1.000000000000000000, 0.000000000000000000, 0.000000000000000000 ) ) ;
#30024 = CARTESIAN_POINT ( 'NONE',  ( -1.166969139818015533, 3.267716535433071279, 0.4724409448818871482 ) ) ;
#30025 = LINE ( 'NONE', #37534, #24673 ) ;
#30026 = ORIENTED_EDGE ( 'NONE', *, *, #7121, .F. ) ;
#30027 = DIRECTION ( 'NONE',  ( 0.000000000000000000, 0.000000000000000000, -1.000000000000000000 ) ) ;
#30028 = PRODUCT_DEFINITION_FORMATION_WITH_SPECIFIED_SOURCE ( 'ANY', '', #14914, .NOT_KNOWN. ) ;
#30029 = VECTOR ( 'NONE', #48503, 39.37007874015748143 ) ;
#30030 = ORIENTED_EDGE ( 'NONE', *, *, #1260, .F. ) ;
#30031 = AXIS2_PLACEMENT_3D ( 'NONE', #16967, #21087, #20827 ) ;
#30032 = CARTESIAN_POINT ( 'NONE',  ( -0.8182917201112819283, 3.346456692913386100, -0.1574803149606301411 ) ) ;
#30033 = CARTESIAN_POINT ( 'NONE',  ( -2.164823134740035737, 6.692913385826772199, -0.04796011690018289753 ) ) ;
#30034 = ORIENTED_EDGE ( 'NONE', *, *, #50962, .T. ) ;
#30035 = CARTESIAN_POINT ( 'NONE',  ( 2.734482843737263025, 1.663397001319319113, -1.115254632218672493 ) ) ;
#30036 = VECTOR ( 'NONE', #14558, 39.37007874015748143 ) ;
#30037 = AXIS2_PLACEMENT_3D ( 'NONE', #25005, #12620, #32251 ) ;
#30038 = CARTESIAN_POINT ( 'NONE',  ( 2.069752515245542046, 1.205361022782829114E-17, -0.5228856972975560735 ) ) ;
#30039 = LINE ( 'NONE', #34922, #28037 ) ;
#30040 = DIRECTION ( 'NONE',  ( -1.000000000000000000, -0.000000000000000000, -0.000000000000000000 ) ) ;
#30041 = EDGE_CURVE ( 'NONE', #20069, #37431, #41581, .T. ) ;
#30042 = VERTEX_POINT ( 'NONE', #22222 ) ;
#30043 = VERTEX_POINT ( 'NONE', #33846 ) ;
#30044 = LINE ( 'NONE', #11184, #43019 ) ;
#30045 = VECTOR ( 'NONE', #48963, 39.37007874015748143 ) ;
#30046 = DIRECTION ( 'NONE',  ( -3.469446951953613696E-16, 0.000000000000000000, -1.000000000000000000 ) ) ;
#30047 = EDGE_CURVE ( 'NONE', #4877, #2471, #26338, .T. ) ;
#30048 = ORIENTED_EDGE ( 'NONE', *, *, #16427, .F. ) ;
#30049 = DIRECTION ( 'NONE',  ( -1.000000000000000000, 0.000000000000000000, -0.000000000000000000 ) ) ;
#30050 = DIRECTION ( 'NONE',  ( -1.000000000000000000, 0.000000000000000000, 0.000000000000000000 ) ) ;
#30051 = CARTESIAN_POINT ( 'NONE',  ( 0.8182917201112819283, 3.346456692913386100, -0.9842519685039348154 ) ) ;
#30052 = EDGE_CURVE ( 'NONE', #38746, #388, #14720, .T. ) ;
#30053 = PRODUCT_RELATED_PRODUCT_CATEGORY ( 'part', '', ( #40108 ) ) ;
#30054 = VERTEX_POINT ( 'NONE', #22465 ) ;
#30055 = VERTEX_POINT ( 'NONE', #14207 ) ;
#30056 = CARTESIAN_POINT ( 'NONE',  ( -2.160501893660597084, 3.267716535433071279, -1.141732283464563791 ) ) ;
#30057 =( BOUNDED_CURVE ( )  B_SPLINE_CURVE ( 3, ( #31690, #47132, #36078, #11804 ),
 .UNSPECIFIED., .F., .F. ) 
 B_SPLINE_CURVE_WITH_KNOTS ( ( 4, 4 ),
 ( 0.5174987408647891973, 0.5682857577414799355 ),
 .UNSPECIFIED. ) 
 CURVE ( )  GEOMETRIC_REPRESENTATION_ITEM ( )  RATIONAL_B_SPLINE_CURVE ( ( 1.000000000000000000, 0.9997850681263177330, 0.9997850681263177330, 1.000000000000000000 ) ) 
 REPRESENTATION_ITEM ( '' )  );
#30058 = DIRECTION ( 'NONE',  ( 1.734723475976806848E-16, -0.000000000000000000, 1.000000000000000000 ) ) ;
#30059 = PLANE ( 'NONE',  #45326 ) ;
#30060 = EDGE_CURVE ( 'NONE', #28528, #22720, #38224, .T. ) ;
#30061 = ORIENTED_EDGE ( 'NONE', *, *, #20243, .T. ) ;
#30062 = FACE_OUTER_BOUND ( 'NONE', #30749, .T. ) ;
#30063 = FACE_BOUND ( 'NONE', #3715, .T. ) ;
#30064 = EDGE_LOOP ( 'NONE', ( #22007, #21948, #34451, #10672 ) ) ;
#30065 = CARTESIAN_POINT ( 'NONE',  ( 0.000000000000000000, 1.574803149606302854, 0.000000000000000000 ) ) ;
#30066 = EDGE_LOOP ( 'NONE', ( #35239, #45432, #37500, #36334 ) ) ;
#30067 = VERTEX_POINT ( 'NONE', #25573 ) ;
#30068 = CARTESIAN_POINT ( 'NONE',  ( -0.03497847339001226852, 0.000000000000000000, 1.180584302963952448 ) ) ;
#30069 = DIRECTION ( 'NONE',  ( -0.01601477604151182663, 0.9998717552508123996, -0.000000000000000000 ) ) ;
#30070 = FACE_OUTER_BOUND ( 'NONE', #11835, .T. ) ;
#30071 = EDGE_CURVE ( 'NONE', #33703, #49472, #45674, .T. ) ;
#30072 = ORIENTED_EDGE ( 'NONE', *, *, #50908, .T. ) ;
#30073 = CARTESIAN_POINT ( 'NONE',  ( -1.325491792074585451, 1.698604322780517650, -2.638988599164751481 ) ) ;
#30074 = DIRECTION ( 'NONE',  ( -0.3166081466550567658, 0.000000000000000000, -0.9485564197619719140 ) ) ;
#30075 = ORIENTED_EDGE ( 'NONE', *, *, #36093, .F. ) ;
#30076 = VECTOR ( 'NONE', #29244, 39.37007874015748143 ) ;
#30077 = ADVANCED_FACE ( 'NONE', ( #5951 ), #21706, .F. ) ;
#30078 = VERTEX_POINT ( 'NONE', #46928 ) ;
#30079 = CARTESIAN_POINT ( 'NONE',  ( 2.106197740627112402, 3.346456692913386100, -0.4724409448818889246 ) ) ;
#30080 = CARTESIAN_POINT ( 'NONE',  ( -1.720314620805551087, 0.000000000000000000, 0.2826945007888154726 ) ) ;
#30081 = VECTOR ( 'NONE', #16452, 39.37007874015748143 ) ;
#30082 = VECTOR ( 'NONE', #10221, 39.37007874015748143 ) ;
#30083 = CARTESIAN_POINT ( 'NONE',  ( -1.472219874544909768, 1.546549606962118517, 2.560030851058948898 ) ) ;
#30084 = DIRECTION ( 'NONE',  ( 0.000000000000000000, -1.000000000000000000, 0.000000000000000000 ) ) ;
#30085 = FACE_OUTER_BOUND ( 'NONE', #33577, .T. ) ;
#30086 = VECTOR ( 'NONE', #30926, 39.37007874015748143 ) ;
#30087 = VERTEX_POINT ( 'NONE', #20092 ) ;
#30088 = FACE_OUTER_BOUND ( 'NONE', #1301, .T. ) ;
#30089 = EDGE_CURVE ( 'NONE', #19068, #9489, #35098, .T. ) ;
#30090 = LINE ( 'NONE', #45802, #46290 ) ;
#30091 = ORIENTED_EDGE ( 'NONE', *, *, #29430, .F. ) ;
#30092 = CARTESIAN_POINT ( 'NONE',  ( -0.1516866087075746383, 1.607047215343822222, -2.234383150555500297 ) ) ;
#30093 = DIRECTION ( 'NONE',  ( 0.000000000000000000, 0.000000000000000000, 1.000000000000000000 ) ) ;
#30094 = ORIENTED_EDGE ( 'NONE', *, *, #32177, .T. ) ;
#30095 = CARTESIAN_POINT ( 'NONE',  ( -0.6808484915247774438, 0.01701463086705359146, 1.674057048625058552 ) ) ;
#30096 = FACE_OUTER_BOUND ( 'NONE', #42800, .T. ) ;
#30097 = CARTESIAN_POINT ( 'NONE',  ( 0.1067246931122726866, 0.02962905676920215767, 0.000000000000000000 ) ) ;
#30098 = VERTEX_POINT ( 'NONE', #50526 ) ;
#30099 = CARTESIAN_POINT ( 'NONE',  ( 0.000000000000000000, 3.267716535433071279, 1.850393700787392293 ) ) ;
#30100 = ORIENTED_EDGE ( 'NONE', *, *, #11858, .F. ) ;
#30101 = FACE_BOUND ( 'NONE', #42172, .T. ) ;
#30102 = LINE ( 'NONE', #2732, #20134 ) ;
#30103 = LINE ( 'NONE', #45821, #44100 ) ;
#30104 = DIRECTION ( 'NONE',  ( 1.000000000000000000, 0.000000000000000000, 0.000000000000000000 ) ) ;
#30105 = ORIENTED_EDGE ( 'NONE', *, *, #39939, .F. ) ;
#30106 = EDGE_LOOP ( 'NONE', ( #43945, #818, #32231, #5763 ) ) ;
#30107 = VECTOR ( 'NONE', #25567, 39.37007874015747433 ) ;
#30108 = DIRECTION ( 'NONE',  ( 1.000000000000000000, 0.000000000000000000, 0.000000000000000000 ) ) ;
#30109 = VECTOR ( 'NONE', #14233, 39.37007874015748143 ) ;
#30110 = VECTOR ( 'NONE', #44601, 39.37007874015748854 ) ;
#30111 = CARTESIAN_POINT ( 'NONE',  ( -1.091055626815042201, 3.346456692913386100, 0.1181102362204705658 ) ) ;
#30112 = FACE_OUTER_BOUND ( 'NONE', #2254, .T. ) ;
#30113 = ORIENTED_EDGE ( 'NONE', *, *, #41186, .T. ) ;
#30114 = CONICAL_SURFACE ( 'NONE', #16931, 1.850107469027523210, 0.6386652850508578450 ) ;
#30115 = EDGE_CURVE ( 'NONE', #37496, #46482, #11597, .T. ) ;
#30116 = CARTESIAN_POINT ( 'NONE',  ( -1.171042467547485311, 1.689145562575557369, 1.864045119995098698 ) ) ;
#30117 = ADVANCED_FACE ( 'NONE', ( #4116 ), #8237, .F. ) ;
#30118 = VERTEX_POINT ( 'NONE', #7230 ) ;
#30119 = CARTESIAN_POINT ( 'NONE',  ( 0.08119777152254364916, 1.623385212329073957, 0.000000000000000000 ) ) ;
#30120 = EDGE_CURVE ( 'NONE', #40985, #43780, #13534, .T. ) ;
#30121 = DIRECTION ( 'NONE',  ( -0.000000000000000000, 1.000000000000000000, -0.000000000000000000 ) ) ;
#30122 = VECTOR ( 'NONE', #2993, 39.37007874015748143 ) ;
#30123 = VERTEX_POINT ( 'NONE', #30969 ) ;
#30124 = FACE_OUTER_BOUND ( 'NONE', #19549, .T. ) ;
#30125 = VERTEX_POINT ( 'NONE', #7476 ) ;
#30126 = ORIENTED_EDGE ( 'NONE', *, *, #25868, .T. ) ;
#30127 = ORIENTED_EDGE ( 'NONE', *, *, #31422, .T. ) ;
#30128 = ORIENTED_EDGE ( 'NONE', *, *, #16576, .F. ) ;
#30129 = DIRECTION ( 'NONE',  ( -0.9839295885986295565, 0.000000000000000000, -0.1785568947986370392 ) ) ;
#30130 = EDGE_LOOP ( 'NONE', ( #3696, #40870, #46681, #37993 ) ) ;
#30131 = DIRECTION ( 'NONE',  ( 0.000000000000000000, 0.000000000000000000, -1.000000000000000000 ) ) ;
#30132 = CARTESIAN_POINT ( 'NONE',  ( 1.560669927219590303, 3.267716535433071279, -1.102362204724405714 ) ) ;
#30133 = EDGE_CURVE ( 'NONE', #11950, #34431, #47177, .T. ) ;
#30134 = CARTESIAN_POINT ( 'NONE',  ( -2.339241080213612101, 1.584370211609867685, 1.802537235681884065 ) ) ;
#30135 = DIRECTION ( 'NONE',  ( -0.000000000000000000, 0.000000000000000000, 1.000000000000000000 ) ) ;
#30136 = DIRECTION ( 'NONE',  ( -0.000000000000000000, 1.000000000000000000, -0.000000000000000000 ) ) ;
#30137 = VECTOR ( 'NONE', #31473, 39.37007874015748143 ) ;
#30138 = EDGE_LOOP ( 'NONE', ( #1450, #6092, #469, #33379 ) ) ;
#30139 = LINE ( 'NONE', #48951, #4151 ) ;
#30140 = FACE_OUTER_BOUND ( 'NONE', #12619, .T. ) ;
#30141 = AXIS2_PLACEMENT_3D ( 'NONE', #30705, #10822, #50020 ) ;
#30142 = DIRECTION ( 'NONE',  ( 0.5877852522924802425, 0.000000000000000000, -0.8090169943749422332 ) ) ;
#30143 = ADVANCED_FACE ( 'NONE', ( #34843 ), #23982, .F. ) ;
#30144 = AXIS2_PLACEMENT_3D ( 'NONE', #16317, #8567, #24320 ) ;
#30145 = CARTESIAN_POINT ( 'NONE',  ( 0.000000000000000000, 3.346456692913386100, 0.000000000000000000 ) ) ;
#30146 = ORIENTED_EDGE ( 'NONE', *, *, #40263, .F. ) ;
#30147 = LINE ( 'NONE', #10776, #9999 ) ;
#30148 = DIRECTION ( 'NONE',  ( 0.000000000000000000, 0.000000000000000000, -1.000000000000000000 ) ) ;
#30149 = ORIENTED_EDGE ( 'NONE', *, *, #4616, .T. ) ;
#30150 = LINE ( 'NONE', #45611, #8157 ) ;
#30151 = AXIS2_PLACEMENT_3D ( 'NONE', #44952, #45199, #41108 ) ;
#30152 = LINE ( 'NONE', #3039, #43205 ) ;
#30153 = AXIS2_PLACEMENT_3D ( 'NONE', #2927, #23050, #46513 ) ;
#30154 = VERTEX_POINT ( 'NONE', #31997 ) ;
#30155 = EDGE_CURVE ( 'NONE', #45550, #9734, #42584, .T. ) ;
#30156 = VERTEX_POINT ( 'NONE', #39733 ) ;
#30157 = PLANE ( 'NONE',  #12404 ) ;
#30158 = EDGE_CURVE ( 'NONE', #11553, #37676, #39058, .T. ) ;
#30159 = CARTESIAN_POINT ( 'NONE',  ( 1.363819533518803251, 0.000000000000000000, 0.1574803149606283648 ) ) ;
#30160 = CARTESIAN_POINT ( 'NONE',  ( -0.5455278134075208785, 0.000000000000000000, 0.6299212598425164567 ) ) ;
#30161 = CARTESIAN_POINT ( 'NONE',  ( 1.181102362204724310, 0.4724409448818893686, -1.062992125984252079 ) ) ;
#30162 = CARTESIAN_POINT ( 'NONE',  ( 1.636583440222563857, 0.000000000000000000, -0.8267716535433055070 ) ) ;
#30163 = EDGE_LOOP ( 'NONE', ( #31895, #1003, #37891, #45452 ) ) ;
#30164 = FACE_OUTER_BOUND ( 'NONE', #47164, .T. ) ;
#30165 = VERTEX_POINT ( 'NONE', #23214 ) ;
#30166 = ORIENTED_EDGE ( 'NONE', *, *, #49200, .T. ) ;
#30167 = CARTESIAN_POINT ( 'NONE',  ( 0.7423782071083084855, 3.346456692913386100, -1.889763779527552812 ) ) ;
#30168 = ORIENTED_EDGE ( 'NONE', *, *, #32880, .T. ) ;
#30169 = CARTESIAN_POINT ( 'NONE',  ( 2.147141360900377105, -3.961648633104548749E-17, 0.3405121111982924997 ) ) ;
#30170 = DIRECTION ( 'NONE',  ( -0.000000000000000000, 1.000000000000000000, -0.000000000000000000 ) ) ;
#30171 = ORIENTED_EDGE ( 'NONE', *, *, #31210, .F. ) ;
#30172 = EDGE_CURVE ( 'NONE', #48863, #15175, #8582, .T. ) ;
#30173 = PLANE ( 'NONE',  #19811 ) ;
#30174 = CARTESIAN_POINT ( 'NONE',  ( 0.000000000000000000, 1.585169487999011917, -2.086614173228346303 ) ) ;
#30175 = EDGE_CURVE ( 'NONE', #47149, #49034, #39218, .T. ) ;
#30176 = EDGE_CURVE ( 'NONE', #23735, #17928, #23464, .T. ) ;
#30177 = FACE_OUTER_BOUND ( 'NONE', #28895, .T. ) ;
#30178 = VECTOR ( 'NONE', #48003, 39.37007874015748143 ) ;
#30179 = VERTEX_POINT ( 'NONE', #3857 ) ;
#30180 = VERTEX_POINT ( 'NONE', #19584 ) ;
#30181 = VECTOR ( 'NONE', #50205, 39.37007874015748143 ) ;
#30182 = DIRECTION ( 'NONE',  ( -0.000000000000000000, 1.000000000000000000, -0.000000000000000000 ) ) ;
#30183 = FACE_BOUND ( 'NONE', #31007, .T. ) ;
#30184 = ORIENTED_EDGE ( 'NONE', *, *, #27830, .T. ) ;
#30185 = AXIS2_PLACEMENT_3D ( 'NONE', #48727, #32534, #44120 ) ;
#30186 = CARTESIAN_POINT ( 'NONE',  ( -0.6214413264104945434, 3.267716535433071279, -1.929133858267710000 ) ) ;
#30187 = CARTESIAN_POINT ( 'NONE',  ( -1.363819533518803029, 3.267716535433071279, 1.220472440944875281 ) ) ;
#30188 = VECTOR ( 'NONE', #28882, 39.37007874015748143 ) ;
#30189 = ORIENTED_EDGE ( 'NONE', *, *, #3290, .F. ) ;
#30190 = ORIENTED_EDGE ( 'NONE', *, *, #28787, .T. ) ;
#30191 = LINE ( 'NONE', #9297, #33214 ) ;
#30192 = AXIS2_PLACEMENT_3D ( 'NONE', #12326, #43805, #7685 ) ;
#30193 = DIRECTION ( 'NONE',  ( -0.000000000000000000, 1.000000000000000000, -0.000000000000000000 ) ) ;
#30194 = ORIENTED_EDGE ( 'NONE', *, *, #20034, .F. ) ;
#30195 = VERTEX_POINT ( 'NONE', #35358 ) ;
#30196 = VERTEX_POINT ( 'NONE', #11348 ) ;
#30197 = PLANE ( 'NONE',  #19435 ) ;
#30198 = DIRECTION ( 'NONE',  ( 0.9005016466594218949, 0.000000000000000000, -0.4348526007323282871 ) ) ;
#30199 = EDGE_CURVE ( 'NONE', #3379, #22305, #51034, .T. ) ;
#30200 = LINE ( 'NONE', #35088, #5782 ) ;
#30201 = ORIENTED_EDGE ( 'NONE', *, *, #36220, .T. ) ;
#30202 = ORIENTED_EDGE ( 'NONE', *, *, #8958, .T. ) ;
#30203 = DIRECTION ( 'NONE',  ( -3.469446951953613696E-16, 0.000000000000000000, -1.000000000000000000 ) ) ;
#30204 = CARTESIAN_POINT ( 'NONE',  ( -0.3739466299075467348, 2.755905511811024056, -1.120342228065320134 ) ) ;
#30205 = CARTESIAN_POINT ( 'NONE',  ( 1.022151107061777253, 1.491913292174420480, 2.770242619046225485 ) ) ;
#30206 = DIRECTION ( 'NONE',  ( 0.9998717552508121775, 0.01601477604151182663, 0.000000000000000000 ) ) ;
#30207 = EDGE_CURVE ( 'NONE', #45537, #13877, #19087, .T. ) ;
#30208 = CARTESIAN_POINT ( 'NONE',  ( -1.487662594350689371, 0.000000000000000000, -0.9622808653958315750 ) ) ;
#30209 = EDGE_CURVE ( 'NONE', #12590, #38358, #15724, .T. ) ;
#30210 = DIRECTION ( 'NONE',  ( 0.04486483035050446017, 0.000000000000000000, 0.9989930665413151445 ) ) ;
#30211 = EDGE_CURVE ( 'NONE', #1329, #31828, #3599, .T. ) ;
#30212 = AXIS2_PLACEMENT_3D ( 'NONE', #8868, #31599, #349 ) ;
#30213 = CARTESIAN_POINT ( 'NONE',  ( 2.867773316779195447, 1.205361022782829114E-17, -0.7050287376752006896 ) ) ;
#30214 = ORIENTED_EDGE ( 'NONE', *, *, #6392, .F. ) ;
#30215 = VECTOR ( 'NONE', #42996, 39.37007874015748143 ) ;
#30216 = DIRECTION ( 'NONE',  ( -0.000000000000000000, 1.000000000000000000, -0.000000000000000000 ) ) ;
#30217 = CARTESIAN_POINT ( 'NONE',  ( 1.909347346926324684, 0.000000000000000000, 0.1574803149606280872 ) ) ;
#30218 = CIRCLE ( 'NONE', #37679, 1.743387098533651480 ) ;
#30219 = VERTEX_POINT ( 'NONE', #40504 ) ;
#30220 = VECTOR ( 'NONE', #50127, 39.37007874015748143 ) ;
#30221 = VERTEX_POINT ( 'NONE', #41019 ) ;
#30222 = CARTESIAN_POINT ( 'NONE',  ( 0.9114270535481910906, 1.729787598242565005, 2.568545968997903994 ) ) ;
#30223 = AXIS2_PLACEMENT_3D ( 'NONE', #38585, #50637, #42694 ) ;
#30224 = VERTEX_POINT ( 'NONE', #24755 ) ;
#30225 = AXIS2_PLACEMENT_3D ( 'NONE', #44001, #43741, #32155 ) ;
#30226 = VERTEX_POINT ( 'NONE', #5643 ) ;
#30227 = DIRECTION ( 'NONE',  ( 0.000000000000000000, -1.000000000000000000, 0.000000000000000000 ) ) ;
#30228 = EDGE_CURVE ( 'NONE', #4915, #16314, #24285, .T. ) ;
#30229 = ORIENTED_EDGE ( 'NONE', *, *, #50311, .T. ) ;
#30230 = EDGE_CURVE ( 'NONE', #46754, #17428, #17701, .T. ) ;
#30231 = LINE ( 'NONE', #50544, #2098 ) ;
#30232 = DIRECTION ( 'NONE',  ( -0.000000000000000000, 0.000000000000000000, 1.000000000000000000 ) ) ;
#30233 = EDGE_CURVE ( 'NONE', #15669, #47219, #42408, .T. ) ;
#30234 = EDGE_CURVE ( 'NONE', #33364, #45220, #44361, .T. ) ;
#30235 = ORIENTED_EDGE ( 'NONE', *, *, #11452, .F. ) ;
#30236 = ORIENTED_EDGE ( 'NONE', *, *, #40489, .T. ) ;
#30237 = CARTESIAN_POINT ( 'NONE',  ( -1.979793062125317693, 1.688404340953838068, 2.191257344206539504 ) ) ;
#30238 = ADVANCED_FACE ( 'NONE', ( #43843 ), #20620, .T. ) ;
#30240 = VERTEX_POINT ( 'NONE', #9260 ) ;
#30239 = EDGE_CURVE ( 'NONE', #32113, #46126, #47946, .T. ) ;
#30241 = ORIENTED_EDGE ( 'NONE', *, *, #40943, .T. ) ;
#30242 = CARTESIAN_POINT ( 'NONE',  ( -1.574237088929739459, 0.000000000000000000, 0.7912475138866331692 ) ) ;
#30243 = CARTESIAN_POINT ( 'NONE',  ( -1.299212598425205423, 3.267716535433071279, -1.732283464566922726 ) ) ;
#30244 = DIRECTION ( 'NONE',  ( -0.000000000000000000, 1.000000000000000000, -0.000000000000000000 ) ) ;
#30245 = DIRECTION ( 'NONE',  ( -0.000000000000000000, 1.000000000000000000, -0.000000000000000000 ) ) ;
#30246 = VERTEX_POINT ( 'NONE', #36892 ) ;
#30247 = DIRECTION ( 'NONE',  ( -3.469446951953613696E-16, 0.000000000000000000, -1.000000000000000000 ) ) ;
#30248 = CARTESIAN_POINT ( 'NONE',  ( -4.268512490100411402E-16, 0.000000000000000000, -2.401574803149598480 ) ) ;
#30249 = DIRECTION ( 'NONE',  ( -1.000000000000000000, 0.000000000000000000, 0.000000000000000000 ) ) ;
#30250 = AXIS2_PLACEMENT_3D ( 'NONE', #31162, #19527, #31672 ) ;
#30251 = EDGE_LOOP ( 'NONE', ( #15204, #38195, #49578, #29888 ) ) ;
#30252 = DIRECTION ( 'NONE',  ( -0.000000000000000000, 1.000000000000000000, -0.000000000000000000 ) ) ;
#30253 = CARTESIAN_POINT ( 'NONE',  ( 1.560669927219590747, 3.267716535433071279, -5.414661521997677271E-16 ) ) ;
#30254 = AXIS2_PLACEMENT_3D ( 'NONE', #36365, #28605, #35849 ) ;
#30255 = ORIENTED_EDGE ( 'NONE', *, *, #8710, .F. ) ;
#30256 = ORIENTED_EDGE ( 'NONE', *, *, #2957, .F. ) ;
#30257 = DIRECTION ( 'NONE',  ( 0.000000000000000000, 0.000000000000000000, 1.000000000000000000 ) ) ;
#30258 = CARTESIAN_POINT ( 'NONE',  ( 0.000000000000000000, 1.574803149606302854, 0.000000000000000000 ) ) ;
#30259 = AXIS2_PLACEMENT_3D ( 'NONE', #46226, #10885, #33891 ) ;
#30260 = PLANE ( 'NONE',  #2224 ) ;
#30261 = DIRECTION ( 'NONE',  ( -1.000000000000000000, 0.000000000000000000, 1.734723475976806848E-16 ) ) ;
#30262 = VERTEX_POINT ( 'NONE', #32774 ) ;
#30263 = ORIENTED_EDGE ( 'NONE', *, *, #50407, .T. ) ;
#30264 = AXIS2_PLACEMENT_3D ( 'NONE', #10372, #26113, #41860 ) ;
#30265 = FILL_AREA_STYLE_COLOUR ( '', #47678 ) ;
#30266 = CARTESIAN_POINT ( 'NONE',  ( 2.501748315610153206, 1.656306346848011035, -1.122817972635221428 ) ) ;
#30267 = ORIENTED_EDGE ( 'NONE', *, *, #37357, .T. ) ;
#30268 = DIRECTION ( 'NONE',  ( 3.986037398843765983E-20, 1.000000000000000000, 1.160734090543304660E-16 ) ) ;
#30269 = DIRECTION ( 'NONE',  ( -0.000000000000000000, 1.000000000000000000, -0.000000000000000000 ) ) ;
#30270 = EDGE_CURVE ( 'NONE', #24599, #23486, #36642, .T. ) ;
#30271 = PLANE ( 'NONE',  #43987 ) ;
#30272 = EDGE_CURVE ( 'NONE', #12169, #7654, #48453, .T. ) ;
#30273 = CARTESIAN_POINT ( 'NONE',  ( 0.8182917201112817063, 0.000000000000000000, -1.732283464566923614 ) ) ;
#30274 = CARTESIAN_POINT ( 'NONE',  ( -0.6214413264104945434, 3.267716535433071279, -1.417322834645664331 ) ) ;
#30275 = EDGE_LOOP ( 'NONE', ( #15337, #36355, #38823, #37698 ) ) ;
#30276 = FACE_OUTER_BOUND ( 'NONE', #24900, .T. ) ;
#30277 =( NAMED_UNIT ( * ) SI_UNIT ( $, .STERADIAN. ) SOLID_ANGLE_UNIT ( ) );
#30278 = DIRECTION ( 'NONE',  ( 0.000000000000000000, -1.000000000000000000, 0.000000000000000000 ) ) ;
#30279 = VERTEX_POINT ( 'NONE', #13390 ) ;
#30280 = DIRECTION ( 'NONE',  ( -0.01601477604151182663, 0.9998717552508123996, -0.000000000000000000 ) ) ;
#30281 = CARTESIAN_POINT ( 'NONE',  ( -1.679154924913551783, 0.000000000000000000, 0.4938453199301923724 ) ) ;
#30282 = CARTESIAN_POINT ( 'NONE',  ( 1.091055626815042645, 0.000000000000000000, 1.062992125984246083 ) ) ;
#30283 = AXIS2_PLACEMENT_3D ( 'NONE', #35700, #35196, #43433 ) ;
#30284 = ORIENTED_EDGE ( 'NONE', *, *, #48495, .T. ) ;
#30285 = DIRECTION ( 'NONE',  ( -3.469446951953613696E-16, 0.000000000000000000, -1.000000000000000000 ) ) ;
#30286 = CIRCLE ( 'NONE', #46713, 2.106299212598425008 ) ;
#30287 = VERTEX_POINT ( 'NONE', #29125 ) ;
#30288 = PLANE ( 'NONE',  #39425 ) ;
#30290 = ORIENTED_EDGE ( 'NONE', *, *, #30294, .F. ) ;
#30289 = EDGE_CURVE ( 'NONE', #4909, #21208, #39702, .T. ) ;
#30291 = B_SPLINE_CURVE_WITH_KNOTS ( 'NONE', 3,
 ( #1259, #48456, #13142, #28873 ),
 .UNSPECIFIED., .F., .F.,
 ( 4, 4 ),
 ( 2.331295889524321270E-07, 0.002500721242867300076 ),
 .UNSPECIFIED. ) ;
#30292 = DIRECTION ( 'NONE',  ( 0.000000000000000000, 0.000000000000000000, 1.000000000000000000 ) ) ;
#30293 = FACE_OUTER_BOUND ( 'NONE', #32386, .T. ) ;
#30294 = EDGE_CURVE ( 'NONE', #33109, #49287, #35824, .T. ) ;
#30295 = CARTESIAN_POINT ( 'NONE',  ( 2.106197740627111958, 0.000000000000000000, 0.9055118110236164419 ) ) ;
#30296 = CARTESIAN_POINT ( 'NONE',  ( -2.182111253630085290, 0.000000000000000000, -0.5118110236220464460 ) ) ;
#30297 = EDGE_CURVE ( 'NONE', #30067, #25537, #24243, .T. ) ;
#30298 = ORIENTED_EDGE ( 'NONE', *, *, #10013, .F. ) ;
#30299 = ORIENTED_EDGE ( 'NONE', *, *, #40711, .F. ) ;
#30300 = DIRECTION ( 'NONE',  ( -1.000000000000000000, 3.986037398843765983E-20, 0.000000000000000000 ) ) ;
#30301 = DIRECTION ( 'NONE',  ( 1.000000000000000000, 0.000000000000000000, -3.469446951953613696E-16 ) ) ;
#30302 = EDGE_CURVE ( 'NONE', #17684, #39256, #44105, .T. ) ;
#30303 = ORIENTED_EDGE ( 'NONE', *, *, #18421, .F. ) ;
#30304 = LINE ( 'NONE', #42167, #11060 ) ;
#30305 = CARTESIAN_POINT ( 'NONE',  ( 1.363819533518803029, 0.000000000000000000, -1.299212598425193210 ) ) ;
#30306 = CARTESIAN_POINT ( 'NONE',  ( -1.068075307999487578, 1.574803149606302854, 1.883606783264637485 ) ) ;
#30307 = VECTOR ( 'NONE', #1115, 39.37007874015748143 ) ;
#30308 = VERTEX_POINT ( 'NONE', #36376 ) ;
#30309 = VERTEX_POINT ( 'NONE', #4620 ) ;
#30310 = B_SPLINE_CURVE_WITH_KNOTS ( 'NONE', 3,
 ( #5809, #14579, #14064, #22070 ),
 .UNSPECIFIED., .F., .F.,
 ( 4, 4 ),
 ( 0.0001266523219680714730, 0.002626713048324111777 ),
 .UNSPECIFIED. ) ;
#30311 = CARTESIAN_POINT ( 'NONE',  ( 0.07982360342473591996, 1.709180471932028711, 0.000000000000000000 ) ) ;
#30312 = FACE_OUTER_BOUND ( 'NONE', #12213, .T. ) ;
#30313 = DIRECTION ( 'NONE',  ( 1.734723475976806848E-16, -0.000000000000000000, 1.000000000000000000 ) ) ;
#30314 = ORIENTED_EDGE ( 'NONE', *, *, #21537, .T. ) ;
#30315 = DIRECTION ( 'NONE',  ( -1.000000000000000000, -0.000000000000000000, -0.000000000000000000 ) ) ;
#30316 = FACE_BOUND ( 'NONE', #49469, .T. ) ;
#30317 = ORIENTED_EDGE ( 'NONE', *, *, #21093, .T. ) ;
#30318 = DIRECTION ( 'NONE',  ( 1.000000000000000000, -0.000000000000000000, 0.000000000000000000 ) ) ;
#30319 = ORIENTED_EDGE ( 'NONE', *, *, #28274, .F. ) ;
#30320 = ORIENTED_EDGE ( 'NONE', *, *, #12605, .F. ) ;
#30321 = FACE_OUTER_BOUND ( 'NONE', #26748, .T. ) ;
#30322 = CARTESIAN_POINT ( 'NONE',  ( -1.166969139818015755, 3.346456692913386100, 0.5905511811023582691 ) ) ;
#30323 = CARTESIAN_POINT ( 'NONE',  ( 0.000000000000000000, 1.595182601976580683, 2.089297179032357121 ) ) ;
#30324 = VECTOR ( 'NONE', #49423, 39.37007874015748143 ) ;
#30325 = AXIS2_PLACEMENT_3D ( 'NONE', #16567, #8043, #8299 ) ;
#30326 = DIRECTION ( 'NONE',  ( 0.000000000000000000, 0.000000000000000000, 1.000000000000000000 ) ) ;
#30327 = PRODUCT_DEFINITION_CONTEXT ( 'detailed design', #39127, 'design' ) ;
#30328 = CARTESIAN_POINT ( 'NONE',  ( 0.4696143004045484348, 0.000000000000000000, 1.850393700787392293 ) ) ;
#30329 = ORIENTED_EDGE ( 'NONE', *, *, #12383, .T. ) ;
#30330 = AXIS2_PLACEMENT_3D ( 'NONE', #519, #23756, #8778 ) ;
#30331 = ORIENTED_EDGE ( 'NONE', *, *, #21062, .F. ) ;
#30332 = CARTESIAN_POINT ( 'NONE',  ( -0.1553040931457698726, 0.000000000000000000, -1.907653760764371986 ) ) ;
#30333 = CARTESIAN_POINT ( 'NONE',  ( 1.905671854841463730, 1.650492703781866632, 2.256015092822682089 ) ) ;
#30334 = CARTESIAN_POINT ( 'NONE',  ( -1.661821349926434932, 1.574803149606302854, 1.388203579611951843 ) ) ;
#30335 = CIRCLE ( 'NONE', #15510, 1.743387098533651480 ) ;
#30336 = EDGE_CURVE ( 'NONE', #47970, #22386, #1513, .T. ) ;
#30337 = DIRECTION ( 'NONE',  ( 0.9998717552508121775, 0.01601477604151182663, 0.000000000000000000 ) ) ;
#30338 = DIRECTION ( 'NONE',  ( -1.000000000000000000, 0.000000000000000000, -0.000000000000000000 ) ) ;
#30339 = VERTEX_POINT ( 'NONE', #21394 ) ;
#30340 = ADVANCED_FACE ( 'NONE', ( #4879 ), #12363, .F. ) ;
#30341 = FACE_OUTER_BOUND ( 'NONE', #5366, .T. ) ;
#30342 = B_SPLINE_CURVE_WITH_KNOTS ( 'NONE', 3,
 ( #1618, #37255, #5749, #29497 ),
 .UNSPECIFIED., .F., .F.,
 ( 4, 4 ),
 ( 0.0003115223527231955440, 0.04960045202335521680 ),
 .UNSPECIFIED. ) ;
#30343 = VECTOR ( 'NONE', #1442, 39.37007874015748143 ) ;
#30344 = DIRECTION ( 'NONE',  ( -1.000000000000000000, 0.000000000000000000, 0.000000000000000000 ) ) ;
#30345 = ADVANCED_FACE ( 'NONE', ( #20363 ), #15220, .T. ) ;
#30346 = ORIENTED_EDGE ( 'NONE', *, *, #41523, .F. ) ;
#30347 = DIRECTION ( 'NONE',  ( -1.000000000000000000, 0.000000000000000000, 0.000000000000000000 ) ) ;
#30348 = CARTESIAN_POINT ( 'NONE',  ( 1.602753508900452317, 0.000000000000000000, 1.341098548255033496 ) ) ;
#30349 = ORIENTED_EDGE ( 'NONE', *, *, #12069, .T. ) ;
#30350 = LINE ( 'NONE', #14091, #12236 ) ;
#30351 = DIRECTION ( 'NONE',  ( -1.000000000000000000, 0.000000000000000000, 0.000000000000000000 ) ) ;
#30352 = DIRECTION ( 'NONE',  ( 1.000000000000000000, 0.000000000000000000, 0.000000000000000000 ) ) ;
#30353 = ORIENTED_EDGE ( 'NONE', *, *, #27386, .T. ) ;
#30354 = DIRECTION ( 'NONE',  ( 1.000000000000000000, 0.000000000000000000, 0.000000000000000000 ) ) ;
#30355 = ORIENTED_EDGE ( 'NONE', *, *, #25040, .T. ) ;
#30356 = FACE_BOUND ( 'NONE', #42850, .T. ) ;
#30357 = DIRECTION ( 'NONE',  ( 0.000000000000000000, 0.000000000000000000, -1.000000000000000000 ) ) ;
#30358 = ADVANCED_FACE ( 'NONE', ( #34289 ), #6149, .T. ) ;
#30359 = DIRECTION ( 'NONE',  ( -0.000000000000000000, 1.000000000000000000, -0.000000000000000000 ) ) ;
#30360 =( BOUNDED_CURVE ( )  B_SPLINE_CURVE ( 3, ( #38591, #49900, #30332, #18958 ),
 .UNSPECIFIED., .F., .F. ) 
 B_SPLINE_CURVE_WITH_KNOTS ( ( 4, 4 ),
 ( 4.494890529461359030, 4.545835423895593586 ),
 .UNSPECIFIED. ) 
 CURVE ( )  GEOMETRIC_REPRESENTATION_ITEM ( )  RATIONAL_B_SPLINE_CURVE ( ( 1.000000000000000000, 0.9997837298384644189, 0.9997837298384644189, 1.000000000000000000 ) ) 
 REPRESENTATION_ITEM ( '' )  );
#30361 = VECTOR ( 'NONE', #12696, 39.37007874015748143 ) ;
#30362 = VECTOR ( 'NONE', #28754, 39.37007874015748143 ) ;
#30363 = B_SPLINE_CURVE_WITH_KNOTS ( 'NONE', 3,
 ( #15986, #39740, #35362, #8500 ),
 .UNSPECIFIED., .F., .F.,
 ( 4, 4 ),
 ( 0.001110332479353618330, 0.04732555827936550663 ),
 .UNSPECIFIED. ) ;
#30364 = ORIENTED_EDGE ( 'NONE', *, *, #29236, .T. ) ;
#30365 = ORIENTED_EDGE ( 'NONE', *, *, #3229, .T. ) ;
#30366 = CARTESIAN_POINT ( 'NONE',  ( -0.2727639067037602727, 3.267716535433071279, 1.850393700787392293 ) ) ;
#30367 = CARTESIAN_POINT ( 'NONE',  ( -2.441132277248549087, 1.049488665752825067, 0.7414267697872314322 ) ) ;
#30368 = EDGE_CURVE ( 'NONE', #32019, #37382, #6909, .T. ) ;
#30369 = VECTOR ( 'NONE', #44077, 39.37007874015748143 ) ;
#30370 = CARTESIAN_POINT ( 'NONE',  ( 1.015142113812069091, 0.000000000000000000, -1.614173228346451605 ) ) ;
#30371 = DIRECTION ( 'NONE',  ( 0.000000000000000000, 1.000000000000000000, 0.000000000000000000 ) ) ;
#30372 = CARTESIAN_POINT ( 'NONE',  ( -1.091055626815042645, 3.346456692913386100, 1.889763779527550147 ) ) ;
#30373 = AXIS2_PLACEMENT_3D ( 'NONE', #43659, #36195, #28172 ) ;
#30374 = ORIENTED_EDGE ( 'NONE', *, *, #14346, .T. ) ;
#30375 = ORIENTED_EDGE ( 'NONE', *, *, #22604, .F. ) ;
#30376 = DIRECTION ( 'NONE',  ( -0.9998717552508121775, -0.01601477604151182316, 0.000000000000000000 ) ) ;
#30377 = AXIS2_PLACEMENT_3D ( 'NONE', #40484, #5365, #16223 ) ;
#30378 = CARTESIAN_POINT ( 'NONE',  ( -1.363819533518803029, 3.346456692913386100, 0.1574803149606287811 ) ) ;
#30379 = ORIENTED_EDGE ( 'NONE', *, *, #6356, .T. ) ;
#30380 = LINE ( 'NONE', #41487, #41390 ) ;
#30381 = ORIENTED_EDGE ( 'NONE', *, *, #32170, .F. ) ;
#30382 = EDGE_LOOP ( 'NONE', ( #14321, #21987, #42659, #38679 ) ) ;
#30383 = AXIS2_PLACEMENT_3D ( 'NONE', #39277, #36889, #1512 ) ;
#30384 = EDGE_CURVE ( 'NONE', #46418, #50585, #17770, .T. ) ;
#30385 = ORIENTED_EDGE ( 'NONE', *, *, #43802, .F. ) ;
#30386 = ORIENTED_EDGE ( 'NONE', *, *, #39873, .F. ) ;
#30387 = CARTESIAN_POINT ( 'NONE',  ( -1.636583440222563635, 3.267716535433071279, -0.1968503937007879123 ) ) ;
#30388 = DIRECTION ( 'NONE',  ( -0.000000000000000000, 1.000000000000000000, -0.000000000000000000 ) ) ;
#30389 = CARTESIAN_POINT ( 'NONE',  ( 1.033984067356529257, 1.658846302404568318, -2.033666571521502764 ) ) ;
#30390 = AXIS2_PLACEMENT_3D ( 'NONE', #40715, #5849, #24716 ) ;
#30391 = CARTESIAN_POINT ( 'NONE',  ( -0.6214413264104939882, 3.346456692913386100, 0.4724409448818872592 ) ) ;
#30392 = DIRECTION ( 'NONE',  ( -0.9998717552508122886, -0.01601477604151185785, 0.000000000000000000 ) ) ;
#30393 = DIRECTION ( 'NONE',  ( 0.9009688679024218105, 5.032645177658756258E-17, -0.4338837391175526803 ) ) ;
#30394 = ORIENTED_EDGE ( 'NONE', *, *, #2722, .T. ) ;
#30395 = EDGE_CURVE ( 'NONE', #34149, #41494, #9773, .T. ) ;
#30396 = LINE ( 'NONE', #34528, #7670 ) ;
#30397 = CARTESIAN_POINT ( 'NONE',  ( -0.07591351300297333182, 3.346456692913386100, -0.1574803149606301411 ) ) ;
#30398 = AXIS2_PLACEMENT_3D ( 'NONE', #32009, #23226, #50792 ) ;
#30399 = CARTESIAN_POINT ( 'NONE',  ( -0.3486774197067347147, 3.267716535433071279, 1.209717811016581790E-16 ) ) ;
#30400 = FACE_OUTER_BOUND ( 'NONE', #38610, .T. ) ;
#30401 = ADVANCED_FACE ( 'NONE', ( #45870 ), #25767, .F. ) ;
#30402 = AXIS2_PLACEMENT_3D ( 'NONE', #1014, #5143, #45129 ) ;
#30403 = VERTEX_POINT ( 'NONE', #6411 ) ;
#30404 = LINE ( 'NONE', #42521, #6718 ) ;
#30405 = EDGE_CURVE ( 'NONE', #48779, #24292, #46510, .T. ) ;
#30406 = DIRECTION ( 'NONE',  ( -0.000000000000000000, 0.000000000000000000, 1.000000000000000000 ) ) ;
#30407 = ORIENTED_EDGE ( 'NONE', *, *, #36534, .T. ) ;
#30408 = LINE ( 'NONE', #2782, #38639 ) ;
#30409 = EDGE_CURVE ( 'NONE', #47890, #23722, #2032, .T. ) ;
#30410 = DIRECTION ( 'NONE',  ( 0.000000000000000000, 1.000000000000000000, 0.000000000000000000 ) ) ;
#30411 = VECTOR ( 'NONE', #25564, 39.37007874015748143 ) ;
#30412 = ORIENTED_EDGE ( 'NONE', *, *, #34608, .F. ) ;
#30413 = CARTESIAN_POINT ( 'NONE',  ( -0.07591351300297284610, 3.346456692913386100, 0.9055118110236167750 ) ) ;
#30414 = VECTOR ( 'NONE', #2020, 39.37007874015748143 ) ;
#30415 = ORIENTED_EDGE ( 'NONE', *, *, #49537, .F. ) ;
#30416 = DIRECTION ( 'NONE',  ( -1.000000000000000000, -0.000000000000000000, -0.000000000000000000 ) ) ;
#30417 = DIRECTION ( 'NONE',  ( -1.000000000000000000, 0.000000000000000000, -0.000000000000000000 ) ) ;
#30418 = DIRECTION ( 'NONE',  ( -1.000000000000000000, 0.000000000000000000, 1.734723475976806848E-16 ) ) ;
#30419 = DIRECTION ( 'NONE',  ( 0.000000000000000000, -1.000000000000000000, -1.156482317317871478E-16 ) ) ;
#30420 = ADVANCED_FACE ( 'NONE', ( #49468 ), #14379, .F. ) ;
#30421 = LINE ( 'NONE', #46135, #5494 ) ;
#30422 = ORIENTED_EDGE ( 'NONE', *, *, #33342, .T. ) ;
#30423 = LINE ( 'NONE', #45883, #38878 ) ;
#30424 = VERTEX_POINT ( 'NONE', #33277 ) ;
#30425 = ORIENTED_EDGE ( 'NONE', *, *, #32335, .T. ) ;
#30426 = DIRECTION ( 'NONE',  ( -1.000000000000000000, -0.000000000000000000, -0.000000000000000000 ) ) ;
#30427 = ORIENTED_EDGE ( 'NONE', *, *, #2722, .F. ) ;
#30428 = EDGE_CURVE ( 'NONE', #5151, #40849, #30152, .T. ) ;
#30429 = CARTESIAN_POINT ( 'NONE',  ( -2.182111253630085734, 3.267716535433071279, -0.9448818897637762948 ) ) ;
#30430 = FACE_OUTER_BOUND ( 'NONE', #50990, .T. ) ;
#30431 = EDGE_LOOP ( 'NONE', ( #6942, #10190, #22405, #10263 ) ) ;
#30432 = LINE ( 'NONE', #10801, #15696 ) ;
#30433 = VECTOR ( 'NONE', #10861, 39.37007874015748143 ) ;
#30434 = EDGE_CURVE ( 'NONE', #122, #16050, #21644, .T. ) ;
#30435 = CARTESIAN_POINT ( 'NONE',  ( 2.298430379965446857, 1.646290322915411997, 0.3610056012771685197 ) ) ;
#30436 = DIRECTION ( 'NONE',  ( -0.000000000000000000, 1.000000000000000000, -0.000000000000000000 ) ) ;
#30437 = EDGE_LOOP ( 'NONE', ( #41565, #20838, #34226, #29911 ) ) ;
#30438 = ORIENTED_EDGE ( 'NONE', *, *, #19604, .T. ) ;
#30439 = B_SPLINE_CURVE_WITH_KNOTS ( 'NONE', 3,
 ( #1267, #32783, #13150, #6163 ),
 .UNSPECIFIED., .F., .F.,
 ( 4, 4 ),
 ( 0.03325564439065060995, 0.03551576279684434678 ),
 .UNSPECIFIED. ) ;
#30440 = CARTESIAN_POINT ( 'NONE',  ( 1.560669927219590303, 3.186757942779276043, -1.929133858267710666 ) ) ;
#30441 = FACE_BOUND ( 'NONE', #49912, .T. ) ;
#30442 = ORIENTED_EDGE ( 'NONE', *, *, #42731, .F. ) ;
#30443 = EDGE_CURVE ( 'NONE', #47349, #9370, #37913, .T. ) ;
#30444 = VECTOR ( 'NONE', #23820, 39.37007874015748143 ) ;
#30445 = VECTOR ( 'NONE', #23579, 39.37007874015748143 ) ;
#30446 = DIRECTION ( 'NONE',  ( -0.5407162030609373726, -0.6444004775717707689, -0.5407162030609374836 ) ) ;
#30447 = CARTESIAN_POINT ( 'NONE',  ( 0.000000000000000000, 5.905511811023623991, 0.000000000000000000 ) ) ;
#30448 = ORIENTED_EDGE ( 'NONE', *, *, #14763, .T. ) ;
#30449 = ORIENTED_EDGE ( 'NONE', *, *, #40611, .F. ) ;
#30450 = VECTOR ( 'NONE', #50417, 39.37007874015748143 ) ;
#30451 = DIRECTION ( 'NONE',  ( -0.000000000000000000, 1.000000000000000000, -0.000000000000000000 ) ) ;
#30452 = LINE ( 'NONE', #46410, #36121 ) ;
#30453 = ADVANCED_FACE ( 'NONE', ( #14148 ), #45613, .F. ) ;
#30454 = ORIENTED_EDGE ( 'NONE', *, *, #43731, .T. ) ;
#30455 = AXIS2_PLACEMENT_3D ( 'NONE', #33912, #38042, #49600 ) ;
#30457 = EDGE_CURVE ( 'NONE', #50243, #9222, #37659, .T. ) ;
#30456 = ORIENTED_EDGE ( 'NONE', *, *, #19647, .F. ) ;
#30458 = CARTESIAN_POINT ( 'NONE',  ( 1.698878324176545718, 1.702304198788448186, -1.556207456470257267 ) ) ;
#30459 = CARTESIAN_POINT ( 'NONE',  ( -1.940243258964476247, 1.049866565877818347, 0.5786780621199733021 ) ) ;
#30460 = CARTESIAN_POINT ( 'NONE',  ( -2.623503965249869729, 1.579940539283962053, 1.355882097269835107 ) ) ;
#30461 = VERTEX_POINT ( 'NONE', #2785 ) ;
#30462 = VERTEX_POINT ( 'NONE', #37403 ) ;
#30463 = DIRECTION ( 'NONE',  ( 0.000000000000000000, 0.000000000000000000, 1.000000000000000000 ) ) ;
#30464 = CARTESIAN_POINT ( 'NONE',  ( 0.2727639067037602172, 3.267716535433071279, -1.732283464566922726 ) ) ;
#30465 = CARTESIAN_POINT ( 'NONE',  ( -0.8182917201112821504, 3.346456692913386100, 1.940849049717691344 ) ) ;
#30466 = CARTESIAN_POINT ( 'NONE',  ( 0.000000000000000000, 3.267716535433071279, 0.000000000000000000 ) ) ;
#30467 = CARTESIAN_POINT ( 'NONE',  ( -1.091055626815042201, 3.346456692913386100, 0.6299212598425164567 ) ) ;
#30468 = EDGE_CURVE ( 'NONE', #35037, #35668, #26522, .T. ) ;
#30469 = CARTESIAN_POINT ( 'NONE',  ( -2.878724150143177507, 5.905511811023623991, -0.6570500018395222241 ) ) ;
#30470 = AXIS2_PLACEMENT_3D ( 'NONE', #32418, #6940, #28263 ) ;
#30471 = EDGE_CURVE ( 'NONE', #33027, #31047, #26024, .T. ) ;
#30472 = CARTESIAN_POINT ( 'NONE',  ( -0.5455278134075214336, 3.267716535433071279, 2.007874015748021268 ) ) ;
#30473 = ORIENTED_EDGE ( 'NONE', *, *, #30489, .F. ) ;
#30474 = CARTESIAN_POINT ( 'NONE',  ( -1.091055626815042645, 3.346456692913386100, -0.1968503937007881899 ) ) ;
#30475 = CARTESIAN_POINT ( 'NONE',  ( -1.166969139818015755, 3.267716535433071279, 4.048737525165545662E-16 ) ) ;
#30476 = VERTEX_POINT ( 'NONE', #18535 ) ;
#30477 = ORIENTED_EDGE ( 'NONE', *, *, #23990, .T. ) ;
#30478 = FACE_OUTER_BOUND ( 'NONE', #11072, .T. ) ;
#30479 = VECTOR ( 'NONE', #41124, 39.37007874015748143 ) ;
#30480 = B_SPLINE_CURVE_WITH_KNOTS ( 'NONE', 3,
 ( #47635, #16957, #12310, #43782 ),
 .UNSPECIFIED., .F., .F.,
 ( 4, 4 ),
 ( 0.0001946104268145259239, 0.004916092170850017672 ),
 .UNSPECIFIED. ) ;
#30481 = LINE ( 'NONE', #6981, #43494 ) ;
#30482 = ORIENTED_EDGE ( 'NONE', *, *, #5584, .F. ) ;
#30483 = ORIENTED_EDGE ( 'NONE', *, *, #39538, .F. ) ;
#30484 = CARTESIAN_POINT ( 'NONE',  ( 1.287906020515830141, 0.000000000000000000, 0.1181102362204704270 ) ) ;
#30485 = VECTOR ( 'NONE', #41406, 39.37007874015748143 ) ;
#30486 = VERTEX_POINT ( 'NONE', #49976 ) ;
#30487 = CARTESIAN_POINT ( 'NONE',  ( -2.122091976112999490, 1.205361022782829114E-17, 0.4338754535132819390 ) ) ;
#30488 = CARTESIAN_POINT ( 'NONE',  ( -1.536664496436148184E-16, 0.000000000000000000, -0.5118110236220465570 ) ) ;
#30489 = EDGE_CURVE ( 'NONE', #49749, #20873, #44626, .T. ) ;
#30490 = VERTEX_POINT ( 'NONE', #14402 ) ;
#30491 = CARTESIAN_POINT ( 'NONE',  ( 1.909347346926324684, 3.346456692913386100, 1.102362204724403938 ) ) ;
#30492 = ORIENTED_EDGE ( 'NONE', *, *, #15883, .T. ) ;
#30493 = ORIENTED_EDGE ( 'NONE', *, *, #6405, .F. ) ;
#30494 = DIRECTION ( 'NONE',  ( -1.000000000000000000, -0.000000000000000000, -0.000000000000000000 ) ) ;
#30495 = DIRECTION ( 'NONE',  ( -0.01601477604151182663, 0.9998717552508123996, -0.000000000000000000 ) ) ;
#30496 = CARTESIAN_POINT ( 'NONE',  ( 0.3530705266098149164, 2.755905511811024056, -0.1234057657284599735 ) ) ;
#30497 = CARTESIAN_POINT ( 'NONE',  ( 3.927031490892378253E-16, 3.346456692913386100, 1.377952755905504256 ) ) ;
#30498 = EDGE_CURVE ( 'NONE', #35392, #31998, #42268, .T. ) ;
#30499 = ORIENTED_EDGE ( 'NONE', *, *, #47110, .T. ) ;
#30500 = EDGE_CURVE ( 'NONE', #39563, #36975, #46439, .T. ) ;
#30501 = CARTESIAN_POINT ( 'NONE',  ( -2.182111253630085734, 0.000000000000000000, -0.6299212598425177889 ) ) ;
#30502 = DIRECTION ( 'NONE',  ( -1.000000000000000000, 0.000000000000000000, 1.734723475976806848E-16 ) ) ;
#30503 = AXIS2_PLACEMENT_3D ( 'NONE', #42429, #7072, #22818 ) ;
#30504 = DIRECTION ( 'NONE',  ( -3.469446951953613696E-16, 0.000000000000000000, -1.000000000000000000 ) ) ;
#30505 = EDGE_CURVE ( 'NONE', #209, #29472, #34139, .T. ) ;
#30506 = ORIENTED_EDGE ( 'NONE', *, *, #22437, .F. ) ;
#30507 = CYLINDRICAL_SURFACE ( 'NONE', #42248, 2.165354330708661568 ) ;
#30508 = EDGE_CURVE ( 'NONE', #14034, #13750, #13197, .T. ) ;
#30509 = ORIENTED_EDGE ( 'NONE', *, *, #22784, .F. ) ;
#30510 = ORIENTED_EDGE ( 'NONE', *, *, #35858, .F. ) ;
#30511 = DIRECTION ( 'NONE',  ( 0.000000000000000000, -1.000000000000000000, 0.000000000000000000 ) ) ;
#30512 = VECTOR ( 'NONE', #39718, 39.37007874015748143 ) ;
#30513 = LINE ( 'NONE', #46225, #29966 ) ;
#30514 = VECTOR ( 'NONE', #46292, 39.37007874015748143 ) ;
#30515 = CARTESIAN_POINT ( 'NONE',  ( -1.977278193622379332, 1.577807025067274882, -0.8986486843887250275 ) ) ;
#30516 = DIRECTION ( 'NONE',  ( 0.000000000000000000, 0.000000000000000000, -1.000000000000000000 ) ) ;
#30517 = EDGE_LOOP ( 'NONE', ( #8625, #21873, #48875, #9073 ) ) ;
#30518 = VERTEX_POINT ( 'NONE', #4058 ) ;
#30519 = CARTESIAN_POINT ( 'NONE',  ( 1.747029694980739345, 5.905511811023623991, 1.330264415365525421 ) ) ;
#30520 = CARTESIAN_POINT ( 'NONE',  ( -0.7331725592709618100, 1.597733653658881758, 2.093588567519426569 ) ) ;
#30521 = VECTOR ( 'NONE', #49041, 39.37007874015748143 ) ;
#30522 = VERTEX_POINT ( 'NONE', #50470 ) ;
#30523 = LINE ( 'NONE', #38025, #18355 ) ;
#30524 = CARTESIAN_POINT ( 'NONE',  ( -2.889674983507169337, 1.575089141731351505, -0.6090712660038034576 ) ) ;
#30525 = EDGE_CURVE ( 'NONE', #11498, #37571, #27022, .T. ) ;
#30526 = ADVANCED_FACE ( 'NONE', ( #39160 ), #43531, .F. ) ;
#30527 = CARTESIAN_POINT ( 'NONE',  ( -1.936544984245357481, 1.681005499398536829, 1.481397815340367963 ) ) ;
#30528 = DIRECTION ( 'NONE',  ( 1.000000000000000000, 0.000000000000000000, 0.000000000000000000 ) ) ;
#30529 = FACE_OUTER_BOUND ( 'NONE', #40443, .T. ) ;
#30530 = ORIENTED_EDGE ( 'NONE', *, *, #16592, .T. ) ;
#30531 = EDGE_CURVE ( 'NONE', #12924, #24123, #43340, .T. ) ;
#30532 = CARTESIAN_POINT ( 'NONE',  ( -2.454875160333845674, 0.000000000000000000, -0.1574803149606298636 ) ) ;
#30533 = CARTESIAN_POINT ( 'NONE',  ( 1.030376884852512109, 0.4561333243160193840, 1.046684505418381539 ) ) ;
#30534 = DIRECTION ( 'NONE',  ( 1.000000000000000000, 0.000000000000000000, 0.000000000000000000 ) ) ;
#30535 = EDGE_LOOP ( 'NONE', ( #593, #2402, #2796, #26666 ) ) ;
#30536 = CARTESIAN_POINT ( 'NONE',  ( 0.002207914879453961969, 5.905511811023623991, 0.04916304461325442243 ) ) ;
#30537 = CARTESIAN_POINT ( 'NONE',  ( -1.678197894094463738, 0.0003569711654407151991, 0.4935343617671685834 ) ) ;
#30538 = DIRECTION ( 'NONE',  ( -3.469446951953613696E-16, 0.000000000000000000, -1.000000000000000000 ) ) ;
#30539 = ORIENTED_EDGE ( 'NONE', *, *, #14149, .T. ) ;
#30540 = CARTESIAN_POINT ( 'NONE',  ( -0.2727639067037608278, 0.000000000000000000, -0.6692913385826758654 ) ) ;
#30541 = ORIENTED_EDGE ( 'NONE', *, *, #20368, .F. ) ;
#30542 = DIRECTION ( 'NONE',  ( -0.9998717552508122886, -0.01601477604151185785, 0.000000000000000000 ) ) ;
#30543 = ORIENTED_EDGE ( 'NONE', *, *, #32585, .F. ) ;
#30544 = CARTESIAN_POINT ( 'NONE',  ( 0.000000000000000000, 3.267716535433071279, 0.000000000000000000 ) ) ;
#30545 = AXIS2_PLACEMENT_3D ( 'NONE', #2768, #4042, #24428 ) ;
#30546 = DIRECTION ( 'NONE',  ( -9.390536051998861478E-17, -1.000000000000000000, 6.822623802544654332E-17 ) ) ;
#30547 = DIRECTION ( 'NONE',  ( 0.000000000000000000, 0.000000000000000000, -1.000000000000000000 ) ) ;
#30548 = LINE ( 'NONE', #18924, #36755 ) ;
#30549 = VECTOR ( 'NONE', #15807, 39.37007874015748143 ) ;
#30550 = ORIENTED_EDGE ( 'NONE', *, *, #20051, .F. ) ;
#30551 = EDGE_LOOP ( 'NONE', ( #6446, #46137, #686, #22545 ) ) ;
#30552 = ORIENTED_EDGE ( 'NONE', *, *, #14564, .T. ) ;
#30553 = LINE ( 'NONE', #18173, #38912 ) ;
#30554 = FACE_OUTER_BOUND ( 'NONE', #21059, .T. ) ;
#30555 = VERTEX_POINT ( 'NONE', #30661 ) ;
#30556 = CARTESIAN_POINT ( 'NONE',  ( -0.6214413264104945434, 3.346456692913386100, -0.4724409448818886470 ) ) ;
#30557 = CARTESIAN_POINT ( 'NONE',  ( 1.956098637639549720, 1.739232450405700847, -1.232242025355393844 ) ) ;
#30558 = VECTOR ( 'NONE', #2555, 39.37007874015748143 ) ;
#30559 = CARTESIAN_POINT ( 'NONE',  ( 0.000000000000000000, 1.574803149606302854, 0.000000000000000000 ) ) ;
#30560 = EDGE_LOOP ( 'NONE', ( #36705, #25647 ) ) ;
#30561 = ORIENTED_EDGE ( 'NONE', *, *, #20604, .F. ) ;
#30562 = ADVANCED_FACE ( 'NONE', ( #8182 ), #50977, .F. ) ;
#30563 = CARTESIAN_POINT ( 'NONE',  ( -0.8182917201112819283, 3.267716535433071279, 2.004783788421104163 ) ) ;
#30564 = DIRECTION ( 'NONE',  ( -1.000000000000000000, 0.000000000000000000, 0.000000000000000000 ) ) ;
#30565 = DIRECTION ( 'NONE',  ( 0.5128992774059071280, 0.000000000000000000, -0.8584487936018655452 ) ) ;
#30566 = EDGE_CURVE ( 'NONE', #46130, #38271, #47063, .T. ) ;
#30567 = ORIENTED_EDGE ( 'NONE', *, *, #25610, .F. ) ;
#30568 = LINE ( 'NONE', #46282, #7585 ) ;
#30569 = ADVANCED_FACE ( 'NONE', ( #31168 ), #7170, .F. ) ;
#30570 = LINE ( 'NONE', #37565, #19399 ) ;
#30571 = ORIENTED_EDGE ( 'NONE', *, *, #4062, .F. ) ;
#30572 = CARTESIAN_POINT ( 'NONE',  ( -0.8152639642640674422, 0.5238118319854313532, 2.032205794941940535 ) ) ;
#30573 = EDGE_LOOP ( 'NONE', ( #43111, #21075, #1575, #43151 ) ) ;
#30574 = ORIENTED_EDGE ( 'NONE', *, *, #8055, .F. ) ;
#30575 = DIRECTION ( 'NONE',  ( 1.734723475976806848E-16, 0.000000000000000000, 1.000000000000000000 ) ) ;
#30576 = DIRECTION ( 'NONE',  ( -0.01601477604151182663, 0.9998717552508123996, -0.000000000000000000 ) ) ;
#30577 = B_SPLINE_CURVE_WITH_KNOTS ( 'NONE', 3,
 ( #26391, #50093, #30527, #3150 ),
 .UNSPECIFIED., .F., .F.,
 ( 4, 4 ),
 ( 2.558111556691897706E-07, 0.01962445202192432056 ),
 .UNSPECIFIED. ) ;
#30578 = FACE_OUTER_BOUND ( 'NONE', #49717, .T. ) ;
#30579 = FACE_OUTER_BOUND ( 'NONE', #36862, .T. ) ;
#30580 = CARTESIAN_POINT ( 'NONE',  ( -1.439733046521777027, 3.346456692913386100, -1.456692913385822186 ) ) ;
#30581 = VERTEX_POINT ( 'NONE', #11542 ) ;
#30582 = EDGE_CURVE ( 'NONE', #46126, #23094, #40767, .T. ) ;
#30583 = ORIENTED_EDGE ( 'NONE', *, *, #10934, .F. ) ;
#30584 = CARTESIAN_POINT ( 'NONE',  ( -0.8182917201112819283, 0.000000000000000000, -2.047244094488181343 ) ) ;
#30585 = DIRECTION ( 'NONE',  ( -0.9195277725514489076, 4.565640798866420661E-17, -0.3930250316539278810 ) ) ;
#30586 = AXIS2_PLACEMENT_3D ( 'NONE', #41832, #33337, #29447 ) ;
#30587 = ADVANCED_FACE ( 'NONE', ( #42527 ), #23156, .F. ) ;
#30588 = CIRCLE ( 'NONE', #918, 2.165354330708661568 ) ;
#30589 = DIRECTION ( 'NONE',  ( -0.000000000000000000, 1.000000000000000000, -0.000000000000000000 ) ) ;
#30590 = EDGE_CURVE ( 'NONE', #20664, #47540, #43988, .T. ) ;
#30591 = CARTESIAN_POINT ( 'NONE',  ( -0.8182917201112819283, 3.346456692913386100, -0.03937007874015895081 ) ) ;
#30592 = LINE ( 'NONE', #30842, #22093 ) ;
#30593 = VERTEX_POINT ( 'NONE', #22910 ) ;
#30594 = DIRECTION ( 'NONE',  ( 0.000000000000000000, -1.000000000000000000, 0.000000000000000000 ) ) ;
#30595 = EDGE_CURVE ( 'NONE', #7931, #11610, #40359, .T. ) ;
#30596 = VECTOR ( 'NONE', #2240, 39.37007874015748143 ) ;
#30597 = FACE_OUTER_BOUND ( 'NONE', #33061, .T. ) ;
#30598 = ORIENTED_EDGE ( 'NONE', *, *, #36542, .T. ) ;
#30599 = CARTESIAN_POINT ( 'NONE',  ( -0.8942052331142552601, 3.346456692913386100, -7.512581982576723358E-16 ) ) ;
#30600 = DIRECTION ( 'NONE',  ( -0.000000000000000000, 0.000000000000000000, 1.000000000000000000 ) ) ;
#30601 = DIRECTION ( 'NONE',  ( 0.000000000000000000, 0.000000000000000000, -1.000000000000000000 ) ) ;
#30602 = DIRECTION ( 'NONE',  ( 0.000000000000000000, 0.000000000000000000, 1.000000000000000000 ) ) ;
#30603 = DIRECTION ( 'NONE',  ( -3.469446951953613696E-16, 0.000000000000000000, -1.000000000000000000 ) ) ;
#30604 = CARTESIAN_POINT ( 'NONE',  ( 0.4435105686220198740, 6.692913385826772199, 2.168331686854578333 ) ) ;
#30605 = ORIENTED_EDGE ( 'NONE', *, *, #1727, .F. ) ;
#30606 = LINE ( 'NONE', #49920, #39496 ) ;
#30607 = ORIENTED_EDGE ( 'NONE', *, *, #37802, .F. ) ;
#30608 = FACE_BOUND ( 'NONE', #28533, .T. ) ;
#30609 = DIRECTION ( 'NONE',  ( -0.9998717552508121775, -0.01601477604151182316, 0.000000000000000000 ) ) ;
#30610 = DIRECTION ( 'NONE',  ( -8.032339854997460071E-17, 1.000000000000000000, 1.007223559679395367E-16 ) ) ;
#30611 = ORIENTED_EDGE ( 'NONE', *, *, #29948, .F. ) ;
#30612 = ORIENTED_EDGE ( 'NONE', *, *, #32631, .F. ) ;
#30613 = DIRECTION ( 'NONE',  ( -0.000000000000000000, 0.000000000000000000, 1.000000000000000000 ) ) ;
#30614 = CARTESIAN_POINT ( 'NONE',  ( 0.2727639067037604947, 0.000000000000000000, 0.1574803149606283648 ) ) ;
#30615 = LINE ( 'NONE', #22869, #29146 ) ;
#30616 = CARTESIAN_POINT ( 'NONE',  ( -1.712496953225537633, 3.267716535433071279, -0.7874015748031470974 ) ) ;
#30617 = PLANE ( 'NONE',  #11246 ) ;
#30618 = VECTOR ( 'NONE', #8724, 39.37007874015748143 ) ;
#30619 = AXIS2_PLACEMENT_3D ( 'NONE', #22901, #46866, #3535 ) ;
#30620 = LINE ( 'NONE', #23886, #28102 ) ;
#30621 = VECTOR ( 'NONE', #13734, 39.37007874015748143 ) ;
#30622 = ORIENTED_EDGE ( 'NONE', *, *, #8296, .F. ) ;
#30623 = ORIENTED_EDGE ( 'NONE', *, *, #38559, .T. ) ;
#30624 = DIRECTION ( 'NONE',  ( 0.000000000000000000, 0.000000000000000000, -1.000000000000000000 ) ) ;
#30625 = CARTESIAN_POINT ( 'NONE',  ( 0.4696143004045484903, 0.000000000000000000, 1.417322834645662777 ) ) ;
#30626 = ADVANCED_FACE ( 'NONE', ( #19530 ), #43273, .F. ) ;
#30627 = VECTOR ( 'NONE', #48303, 39.37007874015748143 ) ;
#30628 = VERTEX_POINT ( 'NONE', #12561 ) ;
#30629 = EDGE_CURVE ( 'NONE', #31910, #9471, #2767, .T. ) ;
#30630 = LINE ( 'NONE', #49192, #25728 ) ;
#30631 = VERTEX_POINT ( 'NONE', #8944 ) ;
#30632 = VECTOR ( 'NONE', #4389, 39.37007874015748143 ) ;
#30633 = ORIENTED_EDGE ( 'NONE', *, *, #11771, .T. ) ;
#30634 = ADVANCED_FACE ( 'NONE', ( #12824 ), #689, .F. ) ;
#30635 = AXIS2_PLACEMENT_3D ( 'NONE', #5640, #48705, #13385 ) ;
#30636 = VERTEX_POINT ( 'NONE', #1200 ) ;
#30637 = ORIENTED_EDGE ( 'NONE', *, *, #31882, .F. ) ;
#30638 = DIRECTION ( 'NONE',  ( -1.000000000000000000, -0.000000000000000000, -0.000000000000000000 ) ) ;
#30639 = B_SPLINE_CURVE_WITH_KNOTS ( 'NONE', 3,
 ( #42973, #27998, #23362, #3751 ),
 .UNSPECIFIED., .F., .F.,
 ( 4, 4 ),
 ( 0.01429305550857794260, 0.03074760744400447526 ),
 .UNSPECIFIED. ) ;
#30640 = FACE_OUTER_BOUND ( 'NONE', #23586, .T. ) ;
#30641 = CARTESIAN_POINT ( 'NONE',  ( 0.6235241006192022706, 0.000000000000000000, 2.074304693190358151 ) ) ;
#30642 = ADVANCED_FACE ( 'NONE', ( #20302 ), #31941, .F. ) ;
#30643 = PLANE ( 'NONE',  #33034 ) ;
#30644 = B_SPLINE_CURVE_WITH_KNOTS ( 'NONE', 3,
 ( #480, #32763, #47681, #21128 ),
 .UNSPECIFIED., .F., .F.,
 ( 4, 4 ),
 ( 2.032841712500688428E-07, 0.01831524776319553433 ),
 .UNSPECIFIED. ) ;
#30645 = CARTESIAN_POINT ( 'NONE',  ( 1.015142113812069091, 0.000000000000000000, -2.244094488188969283 ) ) ;
#30646 = DIRECTION ( 'NONE',  ( -4.561975526775755056E-17, -1.000000000000000000, 1.067327232801816862E-16 ) ) ;
#30647 = VERTEX_POINT ( 'NONE', #4303 ) ;
#30648 = CARTESIAN_POINT ( 'NONE',  ( -1.166969139818016199, 3.346456692913386100, -1.299212598425192544 ) ) ;
#30649 = LINE ( 'NONE', #8609, #22555 ) ;
#30650 = EDGE_CURVE ( 'NONE', #9488, #19294, #30480, .T. ) ;
#30652 = ADVANCED_FACE ( 'NONE', ( #40193 ), #48395, .F. ) ;
#30651 = CARTESIAN_POINT ( 'NONE',  ( 0.1155636338427008941, -0.5222242541845523167, 0.000000000000000000 ) ) ;
#30653 = CARTESIAN_POINT ( 'NONE',  ( -1.690941099774203815, 0.0008361491594236539725, -0.4364244636917575804 ) ) ;
#30654 = AXIS2_PLACEMENT_3D ( 'NONE', #2150, #33656, #49348 ) ;
#30655 = ORIENTED_EDGE ( 'NONE', *, *, #964, .F. ) ;
#30656 = AXIS2_PLACEMENT_3D ( 'NONE', #908, #9167, #21045 ) ;
#30657 = DIRECTION ( 'NONE',  ( 1.734723475976806848E-16, 0.000000000000000000, 1.000000000000000000 ) ) ;
#30658 = LINE ( 'NONE', #11538, #15392 ) ;
#30659 = ORIENTED_EDGE ( 'NONE', *, *, #25323, .F. ) ;
#30660 = CARTESIAN_POINT ( 'NONE',  ( -1.742423195192579266, 0.000000000000000000, 0.06108742340491801065 ) ) ;
#30661 = CARTESIAN_POINT ( 'NONE',  ( -2.032045338671488288, 3.346456692913386100, 0.7480314960629874665 ) ) ;
#30662 = VECTOR ( 'NONE', #40221, 39.37007874015748143 ) ;
#30663 = CARTESIAN_POINT ( 'NONE',  ( 1.723188456408574210, 6.692913385826772199, 1.311251662046226452 ) ) ;
#30664 = EDGE_LOOP ( 'NONE', ( #18448, #22859, #23528, #50877 ) ) ;
#30665 = DIRECTION ( 'NONE',  ( 0.000000000000000000, 0.000000000000000000, -1.000000000000000000 ) ) ;
#30666 = CARTESIAN_POINT ( 'NONE',  ( -0.9602959360900468200, 0.01253876862113688373, 1.511314840084332145 ) ) ;
#30667 = VECTOR ( 'NONE', #50345, 39.37007874015748143 ) ;
#30668 = CARTESIAN_POINT ( 'NONE',  ( -1.712496953225537188, 3.346456692913386100, 1.102362204724404160 ) ) ;
#30669 = DIRECTION ( 'NONE',  ( 1.000000000000000000, 0.000000000000000000, 0.000000000000000000 ) ) ;
#30670 = CARTESIAN_POINT ( 'NONE',  ( 0.000000000000000000, 3.267716535433071279, 0.000000000000000000 ) ) ;
#30671 = ORIENTED_EDGE ( 'NONE', *, *, #49108, .T. ) ;
#30672 = FACE_OUTER_BOUND ( 'NONE', #46658, .T. ) ;
#30673 = ORIENTED_EDGE ( 'NONE', *, *, #19116, .T. ) ;
#30674 = ORIENTED_EDGE ( 'NONE', *, *, #28452, .T. ) ;
#30675 = CARTESIAN_POINT ( 'NONE',  ( 2.734482843737263025, 5.905511811023623991, -1.115254632218672048 ) ) ;
#30676 = ORIENTED_EDGE ( 'NONE', *, *, #32867, .T. ) ;
#30677 = DIRECTION ( 'NONE',  ( 1.734723475976806848E-16, -0.000000000000000000, 1.000000000000000000 ) ) ;
#30678 = CARTESIAN_POINT ( 'NONE',  ( 1.287906020515830141, 3.346456692913386100, -1.141732283464564013 ) ) ;
#30679 = ORIENTED_EDGE ( 'NONE', *, *, #30690, .T. ) ;
#30680 = LINE ( 'NONE', #49244, #37976 ) ;
#30681 = DIRECTION ( 'NONE',  ( -0.000000000000000000, 0.000000000000000000, 1.000000000000000000 ) ) ;
#30682 = EDGE_CURVE ( 'NONE', #42385, #11104, #32973, .T. ) ;
#30683 = PLANE ( 'NONE',  #39555 ) ;
#30684 = EDGE_LOOP ( 'NONE', ( #1105, #12707, #25813, #37940 ) ) ;
#30686 = VERTEX_POINT ( 'NONE', #28815 ) ;
#30685 = EDGE_CURVE ( 'NONE', #31188, #47699, #45672, .T. ) ;
#30687 = CARTESIAN_POINT ( 'NONE',  ( 0.7423782071083091516, 3.267716535433071279, 1.692913385826762873 ) ) ;
#30688 = FACE_BOUND ( 'NONE', #37616, .T. ) ;
#30689 = ORIENTED_EDGE ( 'NONE', *, *, #37580, .T. ) ;
#30690 = EDGE_CURVE ( 'NONE', #11339, #33436, #29065, .T. ) ;
#30691 = PRODUCT_RELATED_PRODUCT_CATEGORY ( 'part', '', ( #14914 ) ) ;
#30692 = VECTOR ( 'NONE', #39000, 39.37007874015748143 ) ;
#30693 = CARTESIAN_POINT ( 'NONE',  ( 1.067222945471691053, 0.5249316475426858419, -1.552631840522197493 ) ) ;
#30694 = EDGE_CURVE ( 'NONE', #36614, #46376, #4562, .T. ) ;
#30696 = VERTEX_POINT ( 'NONE', #44807 ) ;
#30695 = EDGE_CURVE ( 'NONE', #39823, #286, #942, .T. ) ;
#30697 = EDGE_LOOP ( 'NONE', ( #29418, #25054, #15633, #32255, #46010, #13757 ) ) ;
#30698 = FACE_OUTER_BOUND ( 'NONE', #35966, .T. ) ;
#30699 = CONICAL_SURFACE ( 'NONE', #5116, 2.165354330708661568, 0.2617993877991570129 ) ;
#30700 = DIRECTION ( 'NONE',  ( 1.734723475976806848E-16, -0.000000000000000000, 1.000000000000000000 ) ) ;
#30701 = EDGE_LOOP ( 'NONE', ( #7981, #47265, #26879, #3099, #38198 ) ) ;
#30702 = VECTOR ( 'NONE', #22323, 39.37007874015748143 ) ;
#30703 = DIRECTION ( 'NONE',  ( 0.000000000000000000, 0.000000000000000000, -1.000000000000000000 ) ) ;
#30704 = ORIENTED_EDGE ( 'NONE', *, *, #23648, .T. ) ;
#30705 = CARTESIAN_POINT ( 'NONE',  ( -0.5455278134075216556, 0.000000000000000000, -2.401574803149598036 ) ) ;
#30706 = VECTOR ( 'NONE', #14097, 39.37007874015748143 ) ;
#30707 = CARTESIAN_POINT ( 'NONE',  ( 0.000000000000000000, 3.267716535433071279, 1.574803149606291974 ) ) ;
#30708 = ADVANCED_FACE ( 'NONE', ( #44553 ), #16443, .F. ) ;
#30709 = CARTESIAN_POINT ( 'NONE',  ( -1.936750629140493007, 1.578456148182591168, 0.9863243683714766341 ) ) ;
#30710 = VERTEX_POINT ( 'NONE', #40700 ) ;
#30711 = ORIENTED_EDGE ( 'NONE', *, *, #13763, .F. ) ;
#30712 = CARTESIAN_POINT ( 'NONE',  ( 2.100403847690402337, 3.267716535433071279, 0.1574803149606280872 ) ) ;
#30713 = DIRECTION ( 'NONE',  ( -0.000000000000000000, 1.000000000000000000, -0.000000000000000000 ) ) ;
#30714 = DIRECTION ( 'NONE',  ( 1.000000000000000000, 0.000000000000000000, 0.000000000000000000 ) ) ;
#30715 = EDGE_CURVE ( 'NONE', #12697, #21513, #28301, .T. ) ;
#30716 = DIRECTION ( 'NONE',  ( -7.105427357601001859E-15, 0.000000000000000000, 1.000000000000000000 ) ) ;
#30717 = DIRECTION ( 'NONE',  ( 1.734723475976806848E-16, -0.000000000000000000, 1.000000000000000000 ) ) ;
#30718 = DIRECTION ( 'NONE',  ( 0.000000000000000000, -1.000000000000000000, 0.000000000000000000 ) ) ;
#30719 = EDGE_CURVE ( 'NONE', #21756, #32019, #5326, .T. ) ;
#30720 = LINE ( 'NONE', #37721, #3644 ) ;
#30721 = ORIENTED_EDGE ( 'NONE', *, *, #13570, .F. ) ;
#30722 = LINE ( 'NONE', #14467, #48097 ) ;
#30723 = CARTESIAN_POINT ( 'NONE',  ( 0.1067246931122726866, 0.02962905676920215767, 0.000000000000000000 ) ) ;
#30724 = ORIENTED_EDGE ( 'NONE', *, *, #10049, .T. ) ;
#30725 = EDGE_CURVE ( 'NONE', #38443, #23660, #23064, .T. ) ;
#30726 = EDGE_LOOP ( 'NONE', ( #17180, #42787, #6899, #15446 ) ) ;
#30727 = PLANE ( 'NONE',  #27473 ) ;
#30728 = CIRCLE ( 'NONE', #19980, 2.165354330708661568 ) ;
#30729 = DIRECTION ( 'NONE',  ( -0.000000000000000000, 1.000000000000000000, -0.000000000000000000 ) ) ;
#30730 = VERTEX_POINT ( 'NONE', #9459 ) ;
#30731 = AXIS2_PLACEMENT_3D ( 'NONE', #30119, #49437, #21868 ) ;
#30732 = ORIENTED_EDGE ( 'NONE', *, *, #13783, .F. ) ;
#30733 = CARTESIAN_POINT ( 'NONE',  ( 2.059322335531026837, 3.267716535433071279, -0.6692913385826764205 ) ) ;
#30734 = AXIS2_PLACEMENT_3D ( 'NONE', #5487, #36734, #8338 ) ;
#30735 = ORIENTED_EDGE ( 'NONE', *, *, #29518, .F. ) ;
#30736 = VECTOR ( 'NONE', #19637, 39.37007874015748143 ) ;
#30737 = VECTOR ( 'NONE', #29177, 39.37007874015748143 ) ;
#30738 = PLANE ( 'NONE',  #15286 ) ;
#30739 = LINE ( 'NONE', #41849, #38737 ) ;
#30740 = ORIENTED_EDGE ( 'NONE', *, *, #47301, .F. ) ;
#30741 = CONICAL_SURFACE ( 'NONE', #37361, 1.850107469027523210, 0.6386652850508578450 ) ;
#30742 = CARTESIAN_POINT ( 'NONE',  ( 0.04921259842519667277, 1.716250793712470912, 2.716745896894408929 ) ) ;
#30743 = ORIENTED_EDGE ( 'NONE', *, *, #3978, .T. ) ;
#30744 = ORIENTED_EDGE ( 'NONE', *, *, #36807, .F. ) ;
#30745 = PLANE ( 'NONE',  #24354 ) ;
#30746 = FACE_OUTER_BOUND ( 'NONE', #21333, .T. ) ;
#30747 = CARTESIAN_POINT ( 'NONE',  ( 2.793030215715258446, 2.755905511811027164, 0.9592557174602682757 ) ) ;
#30748 = EDGE_CURVE ( 'NONE', #14850, #23656, #16185, .T. ) ;
#30749 = EDGE_LOOP ( 'NONE', ( #34161, #31561, #28162, #34882 ) ) ;
#30750 = CARTESIAN_POINT ( 'NONE',  ( 2.182111253630085290, 0.000000000000000000, 0.6299212598425161236 ) ) ;
#30751 = CARTESIAN_POINT ( 'NONE',  ( -2.623503965249869729, 1.579940539283962053, 1.355882097269835107 ) ) ;
#30752 = EDGE_CURVE ( 'NONE', #17416, #11581, #13842, .T. ) ;
#30753 = EDGE_CURVE ( 'NONE', #19187, #48689, #5837, .T. ) ;
#30754 = ORIENTED_EDGE ( 'NONE', *, *, #44650, .T. ) ;
#30755 = CARTESIAN_POINT ( 'NONE',  ( 0.1968503937007870241, 3.346456692913386100, -1.889763779527552146 ) ) ;
#30756 = ORIENTED_EDGE ( 'NONE', *, *, #8555, .F. ) ;
#30757 = ORIENTED_EDGE ( 'NONE', *, *, #1423, .F. ) ;
#30758 = B_SPLINE_CURVE_WITH_KNOTS ( 'NONE', 3,
 ( #13580, #29317, #29579, #45046 ),
 .UNSPECIFIED., .F., .F.,
 ( 4, 4 ),
 ( 0.0007776637210865601979, 0.04825954388179014287 ),
 .UNSPECIFIED. ) ;
#30759 = CARTESIAN_POINT ( 'NONE',  ( 1.730339651593417072, 29.45029292834837875, 74.39472130795488169 ) ) ;
#30760 = DIRECTION ( 'NONE',  ( 1.000000000000000000, 0.000000000000000000, 0.000000000000000000 ) ) ;
#30761 = DIRECTION ( 'NONE',  ( -3.986037398843765983E-20, -1.000000000000000000, -1.160734090543304660E-16 ) ) ;
#30762 = FACE_OUTER_BOUND ( 'NONE', #40371, .T. ) ;
#30763 = DIRECTION ( 'NONE',  ( -1.000000000000000000, 0.000000000000000000, -0.000000000000000000 ) ) ;
#30764 = ORIENTED_EDGE ( 'NONE', *, *, #12507, .F. ) ;
#30765 = ORIENTED_EDGE ( 'NONE', *, *, #7421, .T. ) ;
#30766 = VECTOR ( 'NONE', #39573, 39.37007874015748143 ) ;
#30767 = LINE ( 'NONE', #3144, #36193 ) ;
#30768 = CARTESIAN_POINT ( 'NONE',  ( 0.000000000000000000, 3.267716535433071279, 1.259842519685033135 ) ) ;
#30769 = ORIENTED_EDGE ( 'NONE', *, *, #26902, .F. ) ;
#30770 = LINE ( 'NONE', #33897, #6827 ) ;
#30771 = CARTESIAN_POINT ( 'NONE',  ( -0.5455278134075214336, 3.346456692913386100, 2.095509194042718182 ) ) ;
#30772 = AXIS2_PLACEMENT_3D ( 'NONE', #46416, #34583, #14705 ) ;
#30773 = CIRCLE ( 'NONE', #37387, 2.106299212598425008 ) ;
#30774 = EDGE_CURVE ( 'NONE', #35146, #9349, #25826, .T. ) ;
#30775 = FACE_OUTER_BOUND ( 'NONE', #22924, .T. ) ;
#30776 = CARTESIAN_POINT ( 'NONE',  ( 1.500384305836228060, 1.644172902614663867, 2.543203386723825066 ) ) ;
#30777 = DIRECTION ( 'NONE',  ( 0.000000000000000000, 0.000000000000000000, -1.000000000000000000 ) ) ;
#30778 = EDGE_LOOP ( 'NONE', ( #5888, #31267, #940, #27208, #11926, #19291, #11451, #27321, #10123, #24729, #13486, #14677, #21009 ) ) ;
#30779 = CARTESIAN_POINT ( 'NONE',  ( -1.636583440222563857, 3.267716535433071279, 2.839019714148966584E-16 ) ) ;
#30780 = LINE ( 'NONE', #46491, #22768 ) ;
#30781 = CARTESIAN_POINT ( 'NONE',  ( 1.909347346926324684, 3.346456692913386100, 0.5905511811023582691 ) ) ;
#30782 = EDGE_CURVE ( 'NONE', #9931, #43660, #33220, .T. ) ;
#30783 = EDGE_LOOP ( 'NONE', ( #48208, #11710, #3833, #9694 ) ) ;
#30784 = PLANE ( 'NONE',  #2622 ) ;
#30785 = CARTESIAN_POINT ( 'NONE',  ( -1.636583440222564301, 0.000000000000000000, -0.3149606299212592275 ) ) ;
#30786 = LINE ( 'NONE', #31039, #49347 ) ;
#30788 = EDGE_CURVE ( 'NONE', #42563, #28312, #19927, .T. ) ;
#30787 = VERTEX_POINT ( 'NONE', #14602 ) ;
#30789 = FACE_OUTER_BOUND ( 'NONE', #46063, .T. ) ;
#30790 = EDGE_CURVE ( 'NONE', #23693, #34628, #29326, .T. ) ;
#30791 = ORIENTED_EDGE ( 'NONE', *, *, #47626, .F. ) ;
#30792 = DIRECTION ( 'NONE',  ( 0.7526474967735860000, 0.000000000000000000, -0.6584236824419781309 ) ) ;
#30793 = ORIENTED_EDGE ( 'NONE', *, *, #12567, .F. ) ;
#30794 = CARTESIAN_POINT ( 'NONE',  ( -0.8182917201112819283, 3.346456692913386100, -0.4724409448818886470 ) ) ;
#30795 = EDGE_LOOP ( 'NONE', ( #30454, #34970, #48915, #15863 ) ) ;
#30796 = EDGE_CURVE ( 'NONE', #8785, #15117, #48903, .T. ) ;
#30797 = DIRECTION ( 'NONE',  ( -0.000000000000000000, 1.000000000000000000, -0.000000000000000000 ) ) ;
#30798 = FACE_OUTER_BOUND ( 'NONE', #44482, .T. ) ;
#30799 = CARTESIAN_POINT ( 'NONE',  ( -1.195183497228115035E-16, 3.346456692913386100, -0.3149606299212591165 ) ) ;
#30800 = ORIENTED_EDGE ( 'NONE', *, *, #50002, .F. ) ;
#30801 = VECTOR ( 'NONE', #44456, 39.37007874015748143 ) ;
#30802 = ORIENTED_EDGE ( 'NONE', *, *, #23387, .T. ) ;
#30803 = ORIENTED_EDGE ( 'NONE', *, *, #15711, .T. ) ;
#30804 = LINE ( 'NONE', #11937, #49588 ) ;
#30805 = CARTESIAN_POINT ( 'NONE',  ( -0.5455278134075217666, 3.226699998040866824, -2.401574803149598036 ) ) ;
#30806 = ORIENTED_EDGE ( 'NONE', *, *, #34267, .T. ) ;
#30807 = AXIS2_PLACEMENT_3D ( 'NONE', #35235, #50414, #10977 ) ;
#30808 = PLANE ( 'NONE',  #26882 ) ;
#30809 = CARTESIAN_POINT ( 'NONE',  ( 0.5455278134075208785, 3.346456692913386100, -2.034427629037600660 ) ) ;
#30810 = AXIS2_PLACEMENT_3D ( 'NONE', #27490, #26734, #15121 ) ;
#30811 = EDGE_CURVE ( 'NONE', #6824, #17653, #2723, .T. ) ;
#30812 = VECTOR ( 'NONE', #17890, 39.37007874015748143 ) ;
#30813 = VERTEX_POINT ( 'NONE', #25966 ) ;
#30814 = ORIENTED_EDGE ( 'NONE', *, *, #7152, .T. ) ;
#30815 = CARTESIAN_POINT ( 'NONE',  ( 2.540858811888025759, 1.656921574833092992, -1.032495749324521706 ) ) ;
#30816 = DIRECTION ( 'NONE',  ( -1.000000000000000000, 0.000000000000000000, 1.734723475976806848E-16 ) ) ;
#30817 = FACE_OUTER_BOUND ( 'NONE', #38545, .T. ) ;
#30818 = ADVANCED_FACE ( 'NONE', ( #10477 ), #36677, .T. ) ;
#30819 = EDGE_CURVE ( 'NONE', #8060, #23582, #13592, .T. ) ;
#30820 = ORIENTED_EDGE ( 'NONE', *, *, #1603, .T. ) ;
#30821 = CARTESIAN_POINT ( 'NONE',  ( -2.721588301569279444, 1.676830576168054865, -1.145422913327642567 ) ) ;
#30822 = LINE ( 'NONE', #16083, #22777 ) ;
#30823 = VECTOR ( 'NONE', #3728, 39.37007874015748143 ) ;
#30824 = ORIENTED_EDGE ( 'NONE', *, *, #8915, .F. ) ;
#30825 = ADVANCED_FACE ( 'NONE', ( #29841 ), #2225, .F. ) ;
#30826 = CARTESIAN_POINT ( 'NONE',  ( 2.951990591674675368, 1.666783180044518087, -0.08331184815398359755 ) ) ;
#30827 = ORIENTED_EDGE ( 'NONE', *, *, #6922, .F. ) ;
#30828 = ORIENTED_EDGE ( 'NONE', *, *, #6348, .T. ) ;
#30829 = B_SPLINE_CURVE_WITH_KNOTS ( 'NONE', 3,
 ( #22820, #15070, #30821, #12721 ),
 .UNSPECIFIED., .F., .F.,
 ( 4, 4 ),
 ( 2.175073774845426906E-07, 0.002500264446635720034 ),
 .UNSPECIFIED. ) ;
#30830 = FACE_OUTER_BOUND ( 'NONE', #49333, .T. ) ;
#30831 = CARTESIAN_POINT ( 'NONE',  ( 0.7423782071083091516, 3.267716535433071279, -2.575641807848711673E-16 ) ) ;
#30832 = CARTESIAN_POINT ( 'NONE',  ( 0.08139965876239094178, 1.610780518492231694, 0.000000000000000000 ) ) ;
#30833 = CARTESIAN_POINT ( 'NONE',  ( 2.695799277629594037, 1.205361022782829114E-17, -1.205759334241453651 ) ) ;
#30834 = CARTESIAN_POINT ( 'NONE',  ( 2.106197740627111958, 0.000000000000000000, -0.6692913385826764205 ) ) ;
#30835 = ORIENTED_EDGE ( 'NONE', *, *, #19244, .T. ) ;
#30836 = ORIENTED_EDGE ( 'NONE', *, *, #9433, .F. ) ;
#30837 = CARTESIAN_POINT ( 'NONE',  ( 1.287906020515830141, 3.267716535433071279, -8.878505979408855953E-16 ) ) ;
#30838 = DIRECTION ( 'NONE',  ( 0.04486483035050446017, -1.160734090543304660E-16, 0.9989930665413151445 ) ) ;
#30839 = EDGE_CURVE ( 'NONE', #13030, #16254, #29143, .T. ) ;
#30840 = VECTOR ( 'NONE', #11207, 39.37007874015748143 ) ;
#30841 = DIRECTION ( 'NONE',  ( 1.000000000000000000, 0.000000000000000000, -3.469446951953613696E-16 ) ) ;
#30842 = CARTESIAN_POINT ( 'NONE',  ( -1.205290937646081417, -0.2057703422145253647, 0.1726618182594312212 ) ) ;
#30843 = ORIENTED_EDGE ( 'NONE', *, *, #29300, .F. ) ;
#30844 = AXIS2_PLACEMENT_3D ( 'NONE', #12406, #28143, #5172 ) ;
#30845 = DIRECTION ( 'NONE',  ( 1.734723475976806848E-16, -0.000000000000000000, 1.000000000000000000 ) ) ;
#30846 = AXIS2_PLACEMENT_3D ( 'NONE', #50727, #35810, #4310 ) ;
#30847 = CARTESIAN_POINT ( 'NONE',  ( -2.152441353505195387, 6.692913385826772199, -0.2419059403265105823 ) ) ;
#30848 = EDGE_CURVE ( 'NONE', #30279, #14307, #49915, .T. ) ;
#30849 = VECTOR ( 'NONE', #628, 39.37007874015748143 ) ;
#30850 = AXIS2_PLACEMENT_3D ( 'NONE', #19335, #46680, #27084 ) ;
#30851 = ORIENTED_EDGE ( 'NONE', *, *, #13629, .F. ) ;
#30852 = CARTESIAN_POINT ( 'NONE',  ( -1.166969139818015755, 3.267716535433071279, 0.9055118110236167750 ) ) ;
#30853 = EDGE_CURVE ( 'NONE', #33984, #17233, #35933, .T. ) ;
#30854 = CARTESIAN_POINT ( 'NONE',  ( 1.636583440222563635, 3.267716535433071279, -0.9448818897637765168 ) ) ;
#30855 = CARTESIAN_POINT ( 'NONE',  ( -1.597750071202345135, 0.000000000000000000, -0.7364305798568749895 ) ) ;
#30856 = EDGE_CURVE ( 'NONE', #42332, #30287, #21336, .T. ) ;
#30857 = CARTESIAN_POINT ( 'NONE',  ( -1.909347346926324906, 0.000000000000000000, -1.102362204724405492 ) ) ;
#30858 = PLANE ( 'NONE',  #28291 ) ;
#30859 = ADVANCED_FACE ( 'NONE', ( #30096 ), #25709, .F. ) ;
#30860 = FACE_OUTER_BOUND ( 'NONE', #43545, .T. ) ;
#30861 = VECTOR ( 'NONE', #6537, 39.37007874015748143 ) ;
#30862 = ORIENTED_EDGE ( 'NONE', *, *, #13774, .T. ) ;
#30863 = PLANE ( 'NONE',  #1585 ) ;
#30864 = ORIENTED_EDGE ( 'NONE', *, *, #23847, .T. ) ;
#30865 = DIRECTION ( 'NONE',  ( 0.6579387259397027066, 0.000000000000000000, 0.7530714660036195163 ) ) ;
#30866 = CARTESIAN_POINT ( 'NONE',  ( 0.4696143004045476577, 3.267716535433071279, -1.629301903132386767E-16 ) ) ;
#30867 = CARTESIAN_POINT ( 'NONE',  ( -1.363819533518803473, 3.346456692913386100, -1.102362204724405270 ) ) ;
#30868 = EDGE_CURVE ( 'NONE', #49388, #47496, #6353, .T. ) ;
#30869 = ORIENTED_EDGE ( 'NONE', *, *, #10596, .T. ) ;
#30870 = ORIENTED_EDGE ( 'NONE', *, *, #19717, .F. ) ;
#30871 = CARTESIAN_POINT ( 'NONE',  ( 1.905671854841463730, 1.650492703781866632, 2.256015092822682089 ) ) ;
#30872 = DIRECTION ( 'NONE',  ( 0.000000000000000000, 0.000000000000000000, -1.000000000000000000 ) ) ;
#30873 = CARTESIAN_POINT ( 'NONE',  ( 0.04921259842519613847, 5.905511811023623991, 2.213282802432569252 ) ) ;
#30874 = DIRECTION ( 'NONE',  ( -1.000000000000000000, 0.000000000000000000, -0.000000000000000000 ) ) ;
#30875 = ADVANCED_FACE ( 'NONE', ( #46813 ), #15103, .F. ) ;
#30876 = DIRECTION ( 'NONE',  ( 1.000000000000000000, 0.000000000000000000, 0.000000000000000000 ) ) ;
#30877 = DIRECTION ( 'NONE',  ( -0.7071067811865482389, 0.000000000000000000, 0.7071067811865467956 ) ) ;
#30878 = EDGE_CURVE ( 'NONE', #43653, #15242, #15359, .T. ) ;
#30879 = EDGE_LOOP ( 'NONE', ( #25548, #26771, #4837, #46272 ) ) ;
#30880 = CARTESIAN_POINT ( 'NONE',  ( 2.949046667275482481, 1.446726060616999154, -0.1488634180638622739 ) ) ;
#30881 = LINE ( 'NONE', #38378, #8471 ) ;
#30882 = EDGE_CURVE ( 'NONE', #42090, #33404, #7362, .T. ) ;
#30883 = PLANE ( 'NONE',  #21561 ) ;
#30884 = VECTOR ( 'NONE', #48823, 39.37007874015748143 ) ;
#30885 = ORIENTED_EDGE ( 'NONE', *, *, #42419, .F. ) ;
#30886 = EDGE_CURVE ( 'NONE', #14806, #23260, #277, .T. ) ;
#30887 = PLANE ( 'NONE',  #34824 ) ;
#30888 = AXIS2_PLACEMENT_3D ( 'NONE', #15671, #3804, #19535 ) ;
#30889 = ORIENTED_EDGE ( 'NONE', *, *, #8547, .T. ) ;
#30890 = VERTEX_POINT ( 'NONE', #14858 ) ;
#30891 = VECTOR ( 'NONE', #25776, 39.37007874015748143 ) ;
#30892 = VECTOR ( 'NONE', #43334, 39.37007874015748143 ) ;
#30893 = ORIENTED_EDGE ( 'NONE', *, *, #42412, .T. ) ;
#30894 = VERTEX_POINT ( 'NONE', #18732 ) ;
#30895 = PLANE ( 'NONE',  #47483 ) ;
#30896 = AXIS2_PLACEMENT_3D ( 'NONE', #31481, #24246, #39991 ) ;
#30897 = CARTESIAN_POINT ( 'NONE',  ( 0.4517796511351843680, 1.715138028758778521, 2.213898087213642007 ) ) ;
#30898 = DIRECTION ( 'NONE',  ( 0.000000000000000000, -0.000000000000000000, 1.000000000000000000 ) ) ;
#30899 = LINE ( 'NONE', #15402, #48124 ) ;
#30900 = CARTESIAN_POINT ( 'NONE',  ( 2.321319991045708075, 1.679465340878977919, -0.1535128031905659829 ) ) ;
#30901 = CARTESIAN_POINT ( 'NONE',  ( 0.000000000000000000, 3.267716535433071279, 1.889763779527550147 ) ) ;
#30902 = CARTESIAN_POINT ( 'NONE',  ( 1.833433833923351353, 3.267716535433071279, 1.377952755905504256 ) ) ;
#30903 = ORIENTED_EDGE ( 'NONE', *, *, #21647, .F. ) ;
#30904 = CARTESIAN_POINT ( 'NONE',  ( -1.025452293874513199, 0.5070346321433201187, 0.9794755770252113747 ) ) ;
#30905 = CARTESIAN_POINT ( 'NONE',  ( 0.1067246931122726866, 0.02962905676920215767, 0.000000000000000000 ) ) ;
#30906 = CARTESIAN_POINT ( 'NONE',  ( -2.793030215715272213, 1.577298709702483093, 0.9592557174602283077 ) ) ;
#30907 = FACE_OUTER_BOUND ( 'NONE', #45379, .T. ) ;
#30908 = ORIENTED_EDGE ( 'NONE', *, *, #44155, .T. ) ;
#30909 = CARTESIAN_POINT ( 'NONE',  ( -0.7380211471543357549, 0.01609890615456165824, -1.645940171248041928 ) ) ;
#30910 = EDGE_CURVE ( 'NONE', #28307, #49731, #20062, .T. ) ;
#30911 = LINE ( 'NONE', #46620, #48335 ) ;
#30912 = ORIENTED_EDGE ( 'NONE', *, *, #31110, .T. ) ;
#30913 = LINE ( 'NONE', #47116, #50947 ) ;
#30914 = CARTESIAN_POINT ( 'NONE',  ( 1.900276455977023549, 1.738338356005314722, -1.313328886422038710 ) ) ;
#30915 = ADVANCED_FACE ( 'NONE', ( #38854 ), #11487, .F. ) ;
#30916 = VECTOR ( 'NONE', #43128, 39.37007874015748143 ) ;
#30917 = EDGE_CURVE ( 'NONE', #20275, #4372, #11015, .T. ) ;
#30918 = AXIS2_PLACEMENT_3D ( 'NONE', #35916, #546, #16293 ) ;
#30919 = CARTESIAN_POINT ( 'NONE',  ( 0.000000000000000000, 3.267716535433071279, -1.259842519685035134 ) ) ;
#30920 = ORIENTED_EDGE ( 'NONE', *, *, #26822, .F. ) ;
#30921 = LINE ( 'NONE', #22415, #17388 ) ;
#30922 = VECTOR ( 'NONE', #29850, 39.37007874015748143 ) ;
#30923 = CARTESIAN_POINT ( 'NONE',  ( 0.08119777152254364916, 1.623385212329073957, 0.000000000000000000 ) ) ;
#30924 = DIRECTION ( 'NONE',  ( 0.000000000000000000, 1.000000000000000000, 0.000000000000000000 ) ) ;
#30925 = CARTESIAN_POINT ( 'NONE',  ( 0.04921259842519603439, 6.692913385826772199, 2.213282802432569252 ) ) ;
#30926 = DIRECTION ( 'NONE',  ( 0.000000000000000000, 1.000000000000000000, 0.000000000000000000 ) ) ;
#30927 = EDGE_LOOP ( 'NONE', ( #9938, #17166, #1866, #13470, #47468, #50138, #40650, #40064, #45126, #9533, #44275, #36478, #11977 ) ) ;
#30928 = AXIS2_PLACEMENT_3D ( 'NONE', #177, #31683, #8193 ) ;
#30929 = ORIENTED_EDGE ( 'NONE', *, *, #8071, .T. ) ;
#30930 = VERTEX_POINT ( 'NONE', #6852 ) ;
#30931 = DIRECTION ( 'NONE',  ( 0.000000000000000000, 0.000000000000000000, -1.000000000000000000 ) ) ;
#30932 = VERTEX_POINT ( 'NONE', #23345 ) ;
#30933 = CARTESIAN_POINT ( 'NONE',  ( 1.698224779224786429, 1.735102128624146811, -1.555582603516539875 ) ) ;
#30934 = ADVANCED_FACE ( 'NONE', ( #19725 ), #30858, .F. ) ;
#30935 = CARTESIAN_POINT ( 'NONE',  ( -0.2727639067037607723, 3.346456692913386100, 0.1574803149606283648 ) ) ;
#30936 = ORIENTED_EDGE ( 'NONE', *, *, #35774, .F. ) ;
#30937 = LINE ( 'NONE', #7191, #24805 ) ;
#30938 = EDGE_CURVE ( 'NONE', #11395, #33586, #26718, .T. ) ;
#30939 = CARTESIAN_POINT ( 'NONE',  ( -1.181102362204724310, 0.5905511811023621549, -1.062992125984252301 ) ) ;
#30940 = VERTEX_POINT ( 'NONE', #46565 ) ;
#30941 = VERTEX_POINT ( 'NONE', #46317 ) ;
#30942 = EDGE_CURVE ( 'NONE', #20401, #47345, #27220, .T. ) ;
#30943 = DIRECTION ( 'NONE',  ( 1.734723475976806848E-16, -0.000000000000000000, 1.000000000000000000 ) ) ;
#30944 = FACE_BOUND ( 'NONE', #35969, .T. ) ;
#30945 = ORIENTED_EDGE ( 'NONE', *, *, #34491, .F. ) ;
#30946 = EDGE_CURVE ( 'NONE', #20050, #50754, #42957, .T. ) ;
#30947 = CARTESIAN_POINT ( 'NONE',  ( 0.8182917201112819283, 3.346456692913386100, -1.102362204724405714 ) ) ;
#30948 = VERTEX_POINT ( 'NONE', #7109 ) ;
#30949 = ORIENTED_EDGE ( 'NONE', *, *, #39385, .F. ) ;
#30950 = CARTESIAN_POINT ( 'NONE',  ( -0.5110594979943671179, 0.000000000000000000, -1.666798357583582524 ) ) ;
#30951 = FACE_OUTER_BOUND ( 'NONE', #45085, .T. ) ;
#30952 = CIRCLE ( 'NONE', #47378, 2.165354330708661568 ) ;
#30953 = EDGE_LOOP ( 'NONE', ( #13458, #27883, #50904, #29063 ) ) ;
#30954 = LINE ( 'NONE', #42311, #41870 ) ;
#30955 = AXIS2_PLACEMENT_3D ( 'NONE', #41596, #34368, #7244 ) ;
#30956 = VERTEX_POINT ( 'NONE', #43213 ) ;
#30957 = PLANE ( 'NONE',  #30141 ) ;
#30958 = PLANE ( 'NONE',  #27477 ) ;
#30959 = CARTESIAN_POINT ( 'NONE',  ( 0.9794755770252102645, 0.000000000000000000, -1.097585813245683717 ) ) ;
#30960 = ORIENTED_EDGE ( 'NONE', *, *, #2924, .F. ) ;
#30961 = ORIENTED_EDGE ( 'NONE', *, *, #46005, .T. ) ;
#30962 = VECTOR ( 'NONE', #10676, 39.37007874015748143 ) ;
#30963 = DIRECTION ( 'NONE',  ( 1.000000000000000000, 0.000000000000000000, 0.000000000000000000 ) ) ;
#30964 = DIRECTION ( 'NONE',  ( 0.000000000000000000, 0.000000000000000000, 1.000000000000000000 ) ) ;
#30965 = CARTESIAN_POINT ( 'NONE',  ( -2.141381699469527167, 0.5249902829290868933, -0.1454317651979360748 ) ) ;
#30966 = FACE_OUTER_BOUND ( 'NONE', #44783, .T. ) ;
#30967 = DIRECTION ( 'NONE',  ( 0.000000000000000000, 0.000000000000000000, -1.000000000000000000 ) ) ;
#30968 = CARTESIAN_POINT ( 'NONE',  ( 0.9218113296639885990, 0.000000000000000000, -1.800737481590852118 ) ) ;
#30969 = CARTESIAN_POINT ( 'NONE',  ( 0.5455278134075212115, 3.346456692913386100, -0.6299212598425181220 ) ) ;
#30970 = EDGE_CURVE ( 'NONE', #36606, #19754, #31363, .T. ) ;
#30971 = ORIENTED_EDGE ( 'NONE', *, *, #35650, .F. ) ;
#30972 = CARTESIAN_POINT ( 'NONE',  ( 0.7423782071083087075, 3.346456692913386100, -6.146657985744592735E-16 ) ) ;
#30973 = ADVANCED_FACE ( 'NONE', ( #2982 ), #38606, .F. ) ;
#30975 = EDGE_CURVE ( 'NONE', #8227, #48919, #22855, .T. ) ;
#30974 = ORIENTED_EDGE ( 'NONE', *, *, #19384, .F. ) ;
#30976 = EDGE_CURVE ( 'NONE', #1350, #22076, #35487, .T. ) ;
#30977 = ORIENTED_EDGE ( 'NONE', *, *, #4004, .F. ) ;
#30978 = CARTESIAN_POINT ( 'NONE',  ( 0.5905511811023621549, 0.000000000000000000, -4.133858267716536083 ) ) ;
#30979 = CARTESIAN_POINT ( 'NONE',  ( 0.000000000000000000, 3.267716535433071279, -0.6299212598425175669 ) ) ;
#30980 = ORIENTED_EDGE ( 'NONE', *, *, #33980, .F. ) ;
#30981 = EDGE_CURVE ( 'NONE', #49145, #27965, #26465, .T. ) ;
#30982 = DIRECTION ( 'NONE',  ( -0.000000000000000000, 1.000000000000000000, -0.000000000000000000 ) ) ;
#30983 = VECTOR ( 'NONE', #7110, 39.37007874015748143 ) ;
#30984 = EDGE_LOOP ( 'NONE', ( #7832, #31808, #31275, #24054 ) ) ;
#30985 = PLANE ( 'NONE',  #50936 ) ;
#30986 = VECTOR ( 'NONE', #31379, 39.37007874015748143 ) ;
#30987 = ORIENTED_EDGE ( 'NONE', *, *, #1344, .F. ) ;
#30988 = CARTESIAN_POINT ( 'NONE',  ( 1.015142113812069091, 3.346456692913386100, -2.047244094488181343 ) ) ;
#30989 = LINE ( 'NONE', #11867, #46974 ) ;
#30990 = EDGE_CURVE ( 'NONE', #42728, #14441, #20752, .T. ) ;
#30991 = VECTOR ( 'NONE', #37756, 39.37007874015748143 ) ;
#30992 = VERTEX_POINT ( 'NONE', #12496 ) ;
#30993 = VECTOR ( 'NONE', #824, 39.37007874015748143 ) ;
#30994 = PLANE ( 'NONE',  #33800 ) ;
#30995 = ORIENTED_EDGE ( 'NONE', *, *, #22472, .F. ) ;
#30996 = ORIENTED_EDGE ( 'NONE', *, *, #45422, .T. ) ;
#30997 = EDGE_CURVE ( 'NONE', #16032, #19475, #41495, .T. ) ;
#30998 = CARTESIAN_POINT ( 'NONE',  ( -2.014631844979636988, 1.610017137301174017, -0.8075755495219558711 ) ) ;
#30999 = CARTESIAN_POINT ( 'NONE',  ( -0.1184164328040565317, 0.000000000000000000, -0.3547750388873516791 ) ) ;
#31000 = CARTESIAN_POINT ( 'NONE',  ( 1.997134316236881091, 3.267716535433071279, -0.6692913385826764205 ) ) ;
#31001 = ORIENTED_EDGE ( 'NONE', *, *, #140, .F. ) ;
#31002 = DIRECTION ( 'NONE',  ( 0.000000000000000000, -1.000000000000000000, -0.000000000000000000 ) ) ;
#31003 = DIRECTION ( 'NONE',  ( 0.000000000000000000, 0.000000000000000000, 1.000000000000000000 ) ) ;
#31004 = VERTEX_POINT ( 'NONE', #32388 ) ;
#31005 = CARTESIAN_POINT ( 'NONE',  ( 0.1067246931122726866, 0.02962905676920215767, 0.000000000000000000 ) ) ;
#31006 = ORIENTED_EDGE ( 'NONE', *, *, #42585, .F. ) ;
#31007 = EDGE_LOOP ( 'NONE', ( #29804, #31090, #5808, #16252 ) ) ;
#31008 = ADVANCED_FACE ( 'NONE', ( #32648 ), #48080, .F. ) ;
#31009 = ORIENTED_EDGE ( 'NONE', *, *, #21580, .F. ) ;
#31010 = PLANE ( 'NONE',  #11938 ) ;
#31011 = ADVANCED_BREP_SHAPE_REPRESENTATION ( '', ( #41044, #26741 ), #43195 ) ;
#31012 = LINE ( 'NONE', #34637, #21713 ) ;
#31014 = LINE ( 'NONE', #8534, #11882 ) ;
#31013 = CIRCLE ( 'NONE', #29360, 2.165354330708661568 ) ;
#31015 = DIRECTION ( 'NONE',  ( 1.000000000000000000, 0.000000000000000000, 0.000000000000000000 ) ) ;
#31016 = ORIENTED_EDGE ( 'NONE', *, *, #19408, .F. ) ;
#31017 = VERTEX_POINT ( 'NONE', #12761 ) ;
#31018 = VECTOR ( 'NONE', #6474, 39.37007874015748143 ) ;
#31019 = CARTESIAN_POINT ( 'NONE',  ( -1.909347346926324462, 3.267716535433071279, 0.5905511811023582691 ) ) ;
#31020 = AXIS2_PLACEMENT_3D ( 'NONE', #45347, #21881, #48942 ) ;
#31021 = FACE_OUTER_BOUND ( 'NONE', #42143, .T. ) ;
#31022 = ORIENTED_EDGE ( 'NONE', *, *, #10764, .F. ) ;
#31023 = LINE ( 'NONE', #3147, #17547 ) ;
#31024 = CARTESIAN_POINT ( 'NONE',  ( -0.8182917201112819283, 3.267716535433071279, 2.047244094488179567 ) ) ;
#31025 = AXIS2_PLACEMENT_3D ( 'NONE', #28190, #4196, #16329 ) ;
#31026 = AXIS2_PLACEMENT_3D ( 'NONE', #14159, #6919, #45622 ) ;
#31027 = CARTESIAN_POINT ( 'NONE',  ( -0.8182917201112819283, 3.346456692913386100, 0.1574803149606285035 ) ) ;
#31028 = CARTESIAN_POINT ( 'NONE',  ( -0.5455278134075216556, 3.346456692913386100, -2.401574803149598036 ) ) ;
#31029 = CARTESIAN_POINT ( 'NONE',  ( -2.950847925457031007, 1.574821451496988933, -0.08326053095501942392 ) ) ;
#31030 = CONICAL_SURFACE ( 'NONE', #22781, 3.033577403570480779, 1.554780866114618743 ) ;
#31031 = EDGE_LOOP ( 'NONE', ( #43464, #20732, #30769, #12955 ) ) ;
#31032 = CARTESIAN_POINT ( 'NONE',  ( 2.106197740627112402, 3.346456692913386100, -0.5026832550384014997 ) ) ;
#31033 = LINE ( 'NONE', #30533, #37600 ) ;
#31034 = EDGE_CURVE ( 'NONE', #45523, #34367, #365, .T. ) ;
#31035 = ADVANCED_FACE ( 'NONE', ( #47825 ), #44241, .F. ) ;
#31036 = ORIENTED_EDGE ( 'NONE', *, *, #40882, .F. ) ;
#31037 = DIRECTION ( 'NONE',  ( -3.469446951953613696E-16, 0.000000000000000000, -1.000000000000000000 ) ) ;
#31038 = CARTESIAN_POINT ( 'NONE',  ( -1.677240863121680414, 0.0007139418753273822464, 0.4932234035542065742 ) ) ;
#31039 = CARTESIAN_POINT ( 'NONE',  ( 0.3381173457103284763, 6.692913385826772199, 2.138793126519850318 ) ) ;
#31040 = EDGE_CURVE ( 'NONE', #36016, #27696, #18010, .T. ) ;
#31041 = ORIENTED_EDGE ( 'NONE', *, *, #37032, .F. ) ;
#31042 = EDGE_CURVE ( 'NONE', #41514, #44911, #28233, .T. ) ;
#31043 = VERTEX_POINT ( 'NONE', #11988 ) ;
#31044 = LINE ( 'NONE', #18916, #27141 ) ;
#31045 = ORIENTED_EDGE ( 'NONE', *, *, #3521, .T. ) ;
#31046 = CARTESIAN_POINT ( 'NONE',  ( 1.091055626815042645, 3.267716535433071279, -1.892679809432644882E-16 ) ) ;
#31047 = VERTEX_POINT ( 'NONE', #47570 ) ;
#31048 = LINE ( 'NONE', #10922, #7037 ) ;
#31049 = PLANE ( 'NONE',  #33007 ) ;
#31050 = CARTESIAN_POINT ( 'NONE',  ( 0.000000000000000000, 3.267716535433071279, -1.417322834645664331 ) ) ;
#31051 = EDGE_CURVE ( 'NONE', #20003, #31330, #5009, .T. ) ;
#31052 = AXIS2_PLACEMENT_3D ( 'NONE', #29838, #9712, #45805 ) ;
#31053 = EDGE_LOOP ( 'NONE', ( #45569, #19458, #31387, #50058 ) ) ;
#31054 = ORIENTED_EDGE ( 'NONE', *, *, #33150, .T. ) ;
#31055 = VERTEX_POINT ( 'NONE', #32133 ) ;
#31056 = CARTESIAN_POINT ( 'NONE',  ( -0.8182917201112814842, 0.000000000000000000, 1.732283464566921172 ) ) ;
#31057 = VECTOR ( 'NONE', #46671, 39.37007874015748143 ) ;
#31058 = DIRECTION ( 'NONE',  ( 0.000000000000000000, 0.000000000000000000, -1.000000000000000000 ) ) ;
#31059 = VECTOR ( 'NONE', #25188, 39.37007874015748143 ) ;
#31060 = ORIENTED_EDGE ( 'NONE', *, *, #50311, .F. ) ;
#31061 = ORIENTED_EDGE ( 'NONE', *, *, #30234, .F. ) ;
#31062 = EDGE_CURVE ( 'NONE', #37485, #19157, #1127, .T. ) ;
#31063 = DIRECTION ( 'NONE',  ( 0.000000000000000000, 1.000000000000000000, 0.000000000000000000 ) ) ;
#31064 = CARTESIAN_POINT ( 'NONE',  ( -1.636583440222564301, 3.346456692913386100, -1.417869535855831975 ) ) ;
#31065 = DIRECTION ( 'NONE',  ( -1.000000000000000000, -0.000000000000000000, -0.000000000000000000 ) ) ;
#31066 = VERTEX_POINT ( 'NONE', #24376 ) ;
#31067 = VERTEX_POINT ( 'NONE', #16891 ) ;
#31068 = DIRECTION ( 'NONE',  ( -1.206139481778036182E-16, 1.000000000000000000, -4.526717189434842013E-17 ) ) ;
#31069 = DIRECTION ( 'NONE',  ( -1.000000000000000000, -0.000000000000000000, -0.000000000000000000 ) ) ;
#31070 = VECTOR ( 'NONE', #24288, 39.37007874015748143 ) ;
#31071 = EDGE_CURVE ( 'NONE', #25341, #17674, #44493, .T. ) ;
#31072 = CARTESIAN_POINT ( 'NONE',  ( 0.4696143004045479352, 3.267716535433071279, -0.4724409448818886470 ) ) ;
#31073 = VERTEX_POINT ( 'NONE', #8374 ) ;
#31074 = DIRECTION ( 'NONE',  ( -0.01601477604151182663, 0.9998717552508123996, -0.000000000000000000 ) ) ;
#31076 = AXIS2_PLACEMENT_3D ( 'NONE', #45767, #10432, #26177 ) ;
#31075 = PLANE ( 'NONE',  #41729 ) ;
#31077 = ORIENTED_EDGE ( 'NONE', *, *, #45721, .F. ) ;
#31078 = LINE ( 'NONE', #46285, #39792 ) ;
#31079 = ORIENTED_EDGE ( 'NONE', *, *, #45651, .T. ) ;
#31080 = ORIENTED_EDGE ( 'NONE', *, *, #36585, .T. ) ;
#31081 = LINE ( 'NONE', #23831, #26236 ) ;
#31082 = LINE ( 'NONE', #23572, #13525 ) ;
#31083 = EDGE_CURVE ( 'NONE', #2673, #23176, #37134, .T. ) ;
#31084 = DIRECTION ( 'NONE',  ( 0.000000000000000000, 0.000000000000000000, -1.000000000000000000 ) ) ;
#31085 = DIRECTION ( 'NONE',  ( -0.01601477604151182663, 0.9998717552508123996, -0.000000000000000000 ) ) ;
#31086 = DIRECTION ( 'NONE',  ( 0.01601477604151182663, -0.9998717552508123996, 0.000000000000000000 ) ) ;
#31087 = ORIENTED_EDGE ( 'NONE', *, *, #11572, .T. ) ;
#31088 = VERTEX_POINT ( 'NONE', #24117 ) ;
#31089 = EDGE_CURVE ( 'NONE', #13729, #23291, #23581, .T. ) ;
#31090 = ORIENTED_EDGE ( 'NONE', *, *, #19890, .F. ) ;
#31091 = DIRECTION ( 'NONE',  ( -0.000000000000000000, 0.000000000000000000, 1.000000000000000000 ) ) ;
#31092 = LINE ( 'NONE', #46795, #25091 ) ;
#31093 = EDGE_CURVE ( 'NONE', #728, #19354, #19972, .T. ) ;
#31094 = AXIS2_PLACEMENT_3D ( 'NONE', #44993, #25137, #21264 ) ;
#31095 = CARTESIAN_POINT ( 'NONE',  ( -1.909347346926324906, 3.346456692913386100, -0.4724409448818884805 ) ) ;
#31096 = LINE ( 'NONE', #34219, #47559 ) ;
#31097 = CARTESIAN_POINT ( 'NONE',  ( 1.743145509346915256, 0.000000000000000000, -0.02902255290747513330 ) ) ;
#31098 = AXIS2_PLACEMENT_3D ( 'NONE', #39088, #38096, #6841 ) ;
#31099 = ORIENTED_EDGE ( 'NONE', *, *, #28361, .F. ) ;
#31100 = DIRECTION ( 'NONE',  ( -3.469446951953613696E-16, 0.000000000000000000, -1.000000000000000000 ) ) ;
#31101 = CARTESIAN_POINT ( 'NONE',  ( -0.2727639067037607723, 3.346456692913386100, -0.4724409448818883694 ) ) ;
#31102 = EDGE_CURVE ( 'NONE', #1336, #18633, #880, .T. ) ;
#31103 = ORIENTED_EDGE ( 'NONE', *, *, #16362, .T. ) ;
#31104 = LINE ( 'NONE', #42712, #34723 ) ;
#31105 = CARTESIAN_POINT ( 'NONE',  ( 1.929629134066521701, 6.692913385826772199, 0.9824921284572420976 ) ) ;
#31106 =( BOUNDED_CURVE ( )  B_SPLINE_CURVE ( 3, ( #5824, #33967, #17954, #48889 ),
 .UNSPECIFIED., .F., .F. ) 
 B_SPLINE_CURVE_WITH_KNOTS ( ( 4, 4 ),
 ( 2.833434655505596034, 2.884195265334674740 ),
 .UNSPECIFIED. ) 
 CURVE ( )  GEOMETRIC_REPRESENTATION_ITEM ( )  RATIONAL_B_SPLINE_CURVE ( ( 1.000000000000000000, 0.9997852915667326812, 0.9997852915667326812, 1.000000000000000000 ) ) 
 REPRESENTATION_ITEM ( '' )  );
#31107 = LINE ( 'NONE', #46811, #32072 ) ;
#31108 = CARTESIAN_POINT ( 'NONE',  ( 0.08119777152254364916, 1.623385212329073957, 0.000000000000000000 ) ) ;
#31109 = DIRECTION ( 'NONE',  ( -0.000000000000000000, 1.000000000000000000, -0.000000000000000000 ) ) ;
#31110 = EDGE_CURVE ( 'NONE', #44277, #35032, #23863, .T. ) ;
#31111 = CARTESIAN_POINT ( 'NONE',  ( -1.439733046521776361, 3.267716535433071279, -0.1968503937007879123 ) ) ;
#31112 = ORIENTED_EDGE ( 'NONE', *, *, #6619, .F. ) ;
#31113 = CARTESIAN_POINT ( 'NONE',  ( 0.1968503937007878568, 3.267716535433071279, 2.204724409448808764 ) ) ;
#31114 = ORIENTED_EDGE ( 'NONE', *, *, #35445, .F. ) ;
#31115 = VECTOR ( 'NONE', #23716, 39.37007874015748143 ) ;
#31116 = CARTESIAN_POINT ( 'NONE',  ( -0.6214413264104945434, 3.267716535433071279, -2.074263738136479240 ) ) ;
#31117 = B_SPLINE_CURVE_WITH_KNOTS ( 'NONE', 3,
 ( #9173, #44529, #24924, #28271 ),
 .UNSPECIFIED., .F., .F.,
 ( 4, 4 ),
 ( 0.01076910417452579295, 0.03073582141358097153 ),
 .UNSPECIFIED. ) ;
#31118 = LINE ( 'NONE', #42724, #48199 ) ;
#31119 = DIRECTION ( 'NONE',  ( -0.000000000000000000, 0.000000000000000000, 1.000000000000000000 ) ) ;
#31120 = VERTEX_POINT ( 'NONE', #626 ) ;
#31121 = ORIENTED_EDGE ( 'NONE', *, *, #39094, .F. ) ;
#31122 = DIRECTION ( 'NONE',  ( -1.000000000000000000, -0.000000000000000000, -0.000000000000000000 ) ) ;
#31123 = CARTESIAN_POINT ( 'NONE',  ( 0.1067246931122726866, 0.02962905676920215767, 0.000000000000000000 ) ) ;
#31124 = CARTESIAN_POINT ( 'NONE',  ( 0.4696143004045476577, 0.000000000000000000, -2.047244094488182231 ) ) ;
#31125 = PLANE ( 'NONE',  #17801 ) ;
#31126 = DIRECTION ( 'NONE',  ( 0.000000000000000000, 0.000000000000000000, 1.000000000000000000 ) ) ;
#31127 = DIRECTION ( 'NONE',  ( -3.469446951953613696E-16, 0.000000000000000000, -1.000000000000000000 ) ) ;
#31128 = EDGE_LOOP ( 'NONE', ( #18354, #22819, #39486, #14118 ) ) ;
#31129 = EDGE_LOOP ( 'NONE', ( #9424, #4505, #4608, #32582 ) ) ;
#31130 = DIRECTION ( 'NONE',  ( -3.469446951953613696E-16, 0.000000000000000000, -1.000000000000000000 ) ) ;
#31131 = VECTOR ( 'NONE', #68, 39.37007874015748143 ) ;
#31132 = VECTOR ( 'NONE', #42093, 39.37007874015748143 ) ;
#31133 = EDGE_CURVE ( 'NONE', #24903, #50014, #20501, .T. ) ;
#31134 = LINE ( 'NONE', #3509, #20736 ) ;
#31135 = EDGE_LOOP ( 'NONE', ( #32744, #25139, #5037, #2187 ) ) ;
#31136 = CARTESIAN_POINT ( 'NONE',  ( 0.4696143004045479352, 3.267716535433071279, 0.1574803149606283648 ) ) ;
#31137 = VERTEX_POINT ( 'NONE', #38730 ) ;
#31138 = ORIENTED_EDGE ( 'NONE', *, *, #21799, .F. ) ;
#31139 = EDGE_CURVE ( 'NONE', #39972, #40324, #25141, .T. ) ;
#31140 = EDGE_CURVE ( 'NONE', #20851, #20050, #166, .T. ) ;
#31141 = ADVANCED_FACE ( 'NONE', ( #46190 ), #30727, .F. ) ;
#31142 = ORIENTED_EDGE ( 'NONE', *, *, #34159, .F. ) ;
#31143 = ORIENTED_EDGE ( 'NONE', *, *, #23643, .F. ) ;
#31144 = DIRECTION ( 'NONE',  ( -0.000000000000000000, 1.000000000000000000, -0.000000000000000000 ) ) ;
#31145 = VERTEX_POINT ( 'NONE', #25645 ) ;
#31147 = CARTESIAN_POINT ( 'NONE',  ( -2.823445274216743073, 1.576824725690453954, 0.8656477926280276014 ) ) ;
#31146 = AXIS2_PLACEMENT_3D ( 'NONE', #14900, #42761, #46360 ) ;
#31148 = DIRECTION ( 'NONE',  ( -0.000000000000000000, 0.000000000000000000, 1.000000000000000000 ) ) ;
#31149 = CARTESIAN_POINT ( 'NONE',  ( 2.274988110810610031, 1.744340048923221920, -0.4687729985174870495 ) ) ;
#31150 = LINE ( 'NONE', #18258, #4964 ) ;
#31151 = ADVANCED_FACE ( 'NONE', ( #45241 ), #17647, .F. ) ;
#31152 = DIRECTION ( 'NONE',  ( 0.000000000000000000, 0.000000000000000000, 1.000000000000000000 ) ) ;
#31153 = DIRECTION ( 'NONE',  ( 0.000000000000000000, 0.000000000000000000, 1.000000000000000000 ) ) ;
#31154 = ORIENTED_EDGE ( 'NONE', *, *, #10507, .T. ) ;
#31155 = DIRECTION ( 'NONE',  ( 0.000000000000000000, 0.000000000000000000, -1.000000000000000000 ) ) ;
#31156 = CARTESIAN_POINT ( 'NONE',  ( -1.936703619043268043, 1.611265300635113862, 0.9862990711594324944 ) ) ;
#31157 = CARTESIAN_POINT ( 'NONE',  ( -0.8182917201112814842, 3.346456692913386100, 1.220472440944875281 ) ) ;
#31158 = LINE ( 'NONE', #11535, #6705 ) ;
#31159 = EDGE_CURVE ( 'NONE', #47282, #23728, #1641, .T. ) ;
#31160 = ORIENTED_EDGE ( 'NONE', *, *, #34008, .F. ) ;
#31161 = CARTESIAN_POINT ( 'NONE',  ( -0.07591351300297333182, 3.346456692913386100, 0.4724409448818869817 ) ) ;
#31162 = CARTESIAN_POINT ( 'NONE',  ( 1.015142113812069313, 0.000000000000000000, -0.1574803149606301411 ) ) ;
#31163 = ORIENTED_EDGE ( 'NONE', *, *, #40780, .F. ) ;
#31164 = LINE ( 'NONE', #50976, #32037 ) ;
#31165 = AXIS2_PLACEMENT_3D ( 'NONE', #112, #27732, #23869 ) ;
#31166 = CONICAL_SURFACE ( 'NONE', #37774, 3.033577403570480779, 1.554780866114618743 ) ;
#31167 = EDGE_CURVE ( 'NONE', #8328, #24653, #18604, .T. ) ;
#31168 = FACE_OUTER_BOUND ( 'NONE', #50920, .T. ) ;
#31169 = ADVANCED_FACE ( 'NONE', ( #22474 ), #22976, .T. ) ;
#31170 = EDGE_CURVE ( 'NONE', #48162, #24696, #5760, .T. ) ;
#31171 = VECTOR ( 'NONE', #34570, 39.37007874015748143 ) ;
#31172 = DIRECTION ( 'NONE',  ( -3.469446951953613696E-16, 0.000000000000000000, -1.000000000000000000 ) ) ;
#31173 = VERTEX_POINT ( 'NONE', #50045 ) ;
#31174 = CARTESIAN_POINT ( 'NONE',  ( -1.377952755905510918, 0.000000000000000000, -4.133858267716536083 ) ) ;
#31175 = LINE ( 'NONE', #11547, #40728 ) ;
#31176 = AXIS2_PLACEMENT_3D ( 'NONE', #47703, #12377, #43602 ) ;
#31177 = CARTESIAN_POINT ( 'NONE',  ( -0.2727639067037608278, 3.346456692913386100, -0.6692913385826758654 ) ) ;
#31178 = FACE_OUTER_BOUND ( 'NONE', #677, .T. ) ;
#31179 = ORIENTED_EDGE ( 'NONE', *, *, #9433, .T. ) ;
#31180 = VECTOR ( 'NONE', #22697, 39.37007874015748143 ) ;
#31181 = EDGE_LOOP ( 'NONE', ( #36941, #32655, #12720, #24470 ) ) ;
#31182 = VERTEX_POINT ( 'NONE', #1899 ) ;
#31183 = DIRECTION ( 'NONE',  ( 1.000000000000000000, 0.000000000000000000, 0.000000000000000000 ) ) ;
#31184 = VERTEX_POINT ( 'NONE', #5519 ) ;
#31185 = FACE_OUTER_BOUND ( 'NONE', #7549, .T. ) ;
#31186 = CONICAL_SURFACE ( 'NONE', #39436, 1.850107469027523210, 0.6386652850508578450 ) ;
#31187 = DIRECTION ( 'NONE',  ( 1.734723475976806848E-16, 0.000000000000000000, 1.000000000000000000 ) ) ;
#31188 = VERTEX_POINT ( 'NONE', #13523 ) ;
#31189 = FACE_OUTER_BOUND ( 'NONE', #19528, .T. ) ;
#31190 = ORIENTED_EDGE ( 'NONE', *, *, #30508, .T. ) ;
#31191 = CARTESIAN_POINT ( 'NONE',  ( 4.268512490100411402E-16, 0.000000000000000000, 1.574803149606291974 ) ) ;
#31192 = ORIENTED_EDGE ( 'NONE', *, *, #25136, .T. ) ;
#31193 = ORIENTED_EDGE ( 'NONE', *, *, #45874, .T. ) ;
#31194 = FACE_OUTER_BOUND ( 'NONE', #22645, .T. ) ;
#31195 = VERTEX_POINT ( 'NONE', #3353 ) ;
#31196 = DIRECTION ( 'NONE',  ( 1.000000000000000000, 0.000000000000000000, 0.000000000000000000 ) ) ;
#31197 = ADVANCED_FACE ( 'NONE', ( #21268 ), #48587, .F. ) ;
#31198 = AXIS2_PLACEMENT_3D ( 'NONE', #43408, #23801, #39549 ) ;
#31199 = EDGE_CURVE ( 'NONE', #47188, #45998, #19093, .T. ) ;
#31200 = VERTEX_POINT ( 'NONE', #38233 ) ;
#31201 = ORIENTED_EDGE ( 'NONE', *, *, #47084, .F. ) ;
#31202 = DIRECTION ( 'NONE',  ( 0.000000000000000000, 0.000000000000000000, 1.000000000000000000 ) ) ;
#31203 = ADVANCED_FACE ( 'NONE', ( #30478 ), #9905, .F. ) ;
#31204 = PLANE ( 'NONE',  #48419 ) ;
#31205 = ORIENTED_EDGE ( 'NONE', *, *, #28530, .F. ) ;
#31206 = AXIS2_PLACEMENT_3D ( 'NONE', #46158, #34067, #26556 ) ;
#31207 = PLANE ( 'NONE',  #45965 ) ;
#31208 = ORIENTED_EDGE ( 'NONE', *, *, #36996, .T. ) ;
#31209 = FACE_OUTER_BOUND ( 'NONE', #36848, .T. ) ;
#31210 = EDGE_CURVE ( 'NONE', #50014, #20106, #50530, .T. ) ;
#31211 = DIRECTION ( 'NONE',  ( 1.000000000000000000, 0.000000000000000000, 0.000000000000000000 ) ) ;
#31212 = VECTOR ( 'NONE', #13028, 39.37007874015748143 ) ;
#31213 = B_SPLINE_CURVE_WITH_KNOTS ( 'NONE', 3,
 ( #17006, #32766, #32243, #16750 ),
 .UNSPECIFIED., .F., .F.,
 ( 4, 4 ),
 ( 5.967759774831694495E-07, 2.699383640232303923E-05 ),
 .UNSPECIFIED. ) ;
#31214 = CARTESIAN_POINT ( 'NONE',  ( 0.7506868623604561197, 1.205361022782829114E-17, 1.860140722251951484 ) ) ;
#31215 = AXIS2_PLACEMENT_3D ( 'NONE', #29368, #49702, #30131 ) ;
#31216 = ORIENTED_EDGE ( 'NONE', *, *, #5967, .F. ) ;
#31217 = ORIENTED_EDGE ( 'NONE', *, *, #15240, .F. ) ;
#31218 = CARTESIAN_POINT ( 'NONE',  ( 0.000000000000000000, 2.755905511811024056, 0.000000000000000000 ) ) ;
#31219 = CARTESIAN_POINT ( 'NONE',  ( 2.168245791271197209, 0.000000000000000000, -2.004968704497248400 ) ) ;
#31220 = DIRECTION ( 'NONE',  ( -0.01601477604151182663, 0.9998717552508123996, -0.000000000000000000 ) ) ;
#31221 = EDGE_CURVE ( 'NONE', #14810, #21120, #14980, .T. ) ;
#31222 = AXIS2_PLACEMENT_3D ( 'NONE', #49913, #37856, #9966 ) ;
#31223 = DIRECTION ( 'NONE',  ( 0.1342332658176522420, 1.288287287306305530E-16, 0.9909497617679352555 ) ) ;
#31224 = PLANE ( 'NONE',  #23162 ) ;
#31225 = EDGE_CURVE ( 'NONE', #35542, #10793, #5774, .T. ) ;
#31226 = AXIS2_PLACEMENT_3D ( 'NONE', #51024, #19078, #15469 ) ;
#31227 = DIRECTION ( 'NONE',  ( -1.000000000000000000, 0.000000000000000000, 1.734723475976806848E-16 ) ) ;
#31228 = ORIENTED_EDGE ( 'NONE', *, *, #6864, .F. ) ;
#31229 = B_SPLINE_CURVE_WITH_KNOTS ( 'NONE', 3,
 ( #10173, #2176, #40914, #32928 ),
 .UNSPECIFIED., .F., .F.,
 ( 4, 4 ),
 ( 0.1211873102087489551, 0.1625992483279400380 ),
 .UNSPECIFIED. ) ;
#31230 = CARTESIAN_POINT ( 'NONE',  ( -2.134236802639925212, 0.000000000000000000, -2.040539317874611847 ) ) ;
#31231 = ADVANCED_FACE ( 'NONE', ( #31238 ), #19342, .F. ) ;
#31232 = VERTEX_POINT ( 'NONE', #31483 ) ;
#31233 = LINE ( 'NONE', #752, #21797 ) ;
#31234 = ADVANCED_FACE ( 'NONE', ( #20101 ), #34850, .T. ) ;
#31235 = EDGE_CURVE ( 'NONE', #19884, #6227, #12117, .T. ) ;
#31236 = ORIENTED_EDGE ( 'NONE', *, *, #19547, .F. ) ;
#31237 = ORIENTED_EDGE ( 'NONE', *, *, #14068, .T. ) ;
#31238 = FACE_OUTER_BOUND ( 'NONE', #44635, .T. ) ;
#31239 = CARTESIAN_POINT ( 'NONE',  ( 0.1968503937007877735, 0.000000000000000000, 0.7480314960629874665 ) ) ;
#31240 = VECTOR ( 'NONE', #28767, 39.37007874015748143 ) ;
#31241 = ORIENTED_EDGE ( 'NONE', *, *, #20167, .T. ) ;
#31242 = LINE ( 'NONE', #47701, #32889 ) ;
#31243 = ORIENTED_EDGE ( 'NONE', *, *, #25198, .F. ) ;
#31244 = CARTESIAN_POINT ( 'NONE',  ( -0.9147270545203428638, 1.660442526372950311, -2.012873768794291252 ) ) ;
#31245 = ORIENTED_EDGE ( 'NONE', *, *, #5679, .T. ) ;
#31246 = VECTOR ( 'NONE', #5217, 39.37007874015748143 ) ;
#31247 = AXIS2_PLACEMENT_3D ( 'NONE', #25621, #37765, #25367 ) ;
#31248 = CARTESIAN_POINT ( 'NONE',  ( 4.268512490100411402E-16, 3.346456692913386100, 1.574803149606291974 ) ) ;
#31249 = LINE ( 'NONE', #19603, #38770 ) ;
#31250 = VECTOR ( 'NONE', #21060, 39.37007874015748143 ) ;
#31251 = ORIENTED_EDGE ( 'NONE', *, *, #38399, .T. ) ;
#31252 = CARTESIAN_POINT ( 'NONE',  ( 0.7423782071083091516, 3.267716535433071279, 1.062992125984246083 ) ) ;
#31253 = ORIENTED_EDGE ( 'NONE', *, *, #26758, .T. ) ;
#31254 = ORIENTED_EDGE ( 'NONE', *, *, #34925, .F. ) ;
#31255 = CARTESIAN_POINT ( 'NONE',  ( -0.2834077913992259501, -0.6299212598425202314, -0.2440651625074179987 ) ) ;
#31256 = LINE ( 'NONE', #777, #23174 ) ;
#31257 = LINE ( 'NONE', #7503, #34287 ) ;
#31258 = VECTOR ( 'NONE', #8876, 39.37007874015748143 ) ;
#31259 = ORIENTED_EDGE ( 'NONE', *, *, #20034, .T. ) ;
#31260 = DIRECTION ( 'NONE',  ( 1.000000000000000000, 0.000000000000000000, -3.469446951953613696E-16 ) ) ;
#31261 = DIRECTION ( 'NONE',  ( -0.000000000000000000, 1.000000000000000000, 0.000000000000000000 ) ) ;
#31262 = EDGE_LOOP ( 'NONE', ( #10791, #29165, #49763, #26170, #46052, #1034, #38312, #14562, #9505, #33432, #2372, #44822, #12539 ) ) ;
#31263 = DIRECTION ( 'NONE',  ( -0.01601477604151182663, 0.9998717552508123996, -0.000000000000000000 ) ) ;
#31264 = EDGE_CURVE ( 'NONE', #49792, #20204, #11357, .T. ) ;
#31265 = EDGE_CURVE ( 'NONE', #16316, #14514, #30363, .T. ) ;
#31266 = ORIENTED_EDGE ( 'NONE', *, *, #8958, .F. ) ;
#31267 = ORIENTED_EDGE ( 'NONE', *, *, #27531, .F. ) ;
#31268 = ADVANCED_FACE ( 'NONE', ( #24251 ), #27508, .T. ) ;
#31269 = ORIENTED_EDGE ( 'NONE', *, *, #40385, .F. ) ;
#31270 = CARTESIAN_POINT ( 'NONE',  ( -0.5905738936209794510, 0.01846054376545745376, 1.713635781666723146 ) ) ;
#31271 = CARTESIAN_POINT ( 'NONE',  ( 0.2727639067037604947, 3.346456692913386100, -0.4724409448818886470 ) ) ;
#31272 = VECTOR ( 'NONE', #48540, 39.37007874015748143 ) ;
#31273 = CARTESIAN_POINT ( 'NONE',  ( 0.000000000000000000, 10.31496062992126284, 0.000000000000000000 ) ) ;
#31274 = LINE ( 'NONE', #39261, #31282 ) ;
#31275 = ORIENTED_EDGE ( 'NONE', *, *, #16264, .T. ) ;
#31276 = EDGE_LOOP ( 'NONE', ( #3895, #43622, #35813, #46286, #21772, #22986, #40330, #45377, #22082, #36270, #23005 ) ) ;
#31277 = CARTESIAN_POINT ( 'NONE',  ( -1.105178190331685961, 1.205361022782829114E-17, -1.437421806808603542 ) ) ;
#31278 = CARTESIAN_POINT ( 'NONE',  ( 1.833433833923351353, 0.000000000000000000, -1.259842519685035800 ) ) ;
#31279 = ORIENTED_EDGE ( 'NONE', *, *, #30120, .F. ) ;
#31280 = LINE ( 'NONE', #5880, #45565 ) ;
#31281 = CARTESIAN_POINT ( 'NONE',  ( 0.08139965876239094178, 1.610780518492231694, 0.000000000000000000 ) ) ;
#31282 = VECTOR ( 'NONE', #27376, 39.37007874015748143 ) ;
#31283 = ADVANCED_FACE ( 'NONE', ( #47183 ), #8244, .F. ) ;
#31284 = VECTOR ( 'NONE', #6549, 39.37007874015748143 ) ;
#31285 = CARTESIAN_POINT ( 'NONE',  ( 0.4696143004045478797, 3.346456692913386100, -0.6692913385826760875 ) ) ;
#31286 = DIRECTION ( 'NONE',  ( 1.000000000000000000, 0.000000000000000000, 0.000000000000000000 ) ) ;
#31287 = DIRECTION ( 'NONE',  ( -1.000000000000000000, 0.000000000000000000, -0.000000000000000000 ) ) ;
#31288 = VERTEX_POINT ( 'NONE', #46687 ) ;
#31289 = CARTESIAN_POINT ( 'NONE',  ( -0.8942052331142552601, 0.000000000000000000, -1.141732283464563569 ) ) ;
#31290 = EDGE_CURVE ( 'NONE', #1678, #44472, #15229, .T. ) ;
#31291 = ADVANCED_FACE ( 'NONE', ( #27341 ), #43339, .F. ) ;
#31292 = AXIS2_PLACEMENT_3D ( 'NONE', #49363, #33425, #40643 ) ;
#31293 = EDGE_LOOP ( 'NONE', ( #23179, #18339, #48686, #20014 ) ) ;
#31294 = ORIENTED_EDGE ( 'NONE', *, *, #17215, .F. ) ;
#31295 = LINE ( 'NONE', #27654, #13384 ) ;
#31296 = DIRECTION ( 'NONE',  ( -0.000000000000000000, 1.000000000000000000, -0.000000000000000000 ) ) ;
#31297 = CARTESIAN_POINT ( 'NONE',  ( 1.695772546416037363, 1.745688802946234297, -2.417756147381349141 ) ) ;
#31298 = ORIENTED_EDGE ( 'NONE', *, *, #14401, .T. ) ;
#31299 = VERTEX_POINT ( 'NONE', #11854 ) ;
#31300 = FACE_OUTER_BOUND ( 'NONE', #29425, .T. ) ;
#31301 = ORIENTED_EDGE ( 'NONE', *, *, #20305, .T. ) ;
#31302 = FACE_OUTER_BOUND ( 'NONE', #16630, .T. ) ;
#31303 = VERTEX_POINT ( 'NONE', #23221 ) ;
#31304 = LINE ( 'NONE', #11676, #41690 ) ;
#31305 = LINE ( 'NONE', #50855, #23918 ) ;
#31306 = CARTESIAN_POINT ( 'NONE',  ( 2.378961647330872786, 3.267716535433071279, -8.253681236146643855E-16 ) ) ;
#31307 = VECTOR ( 'NONE', #29416, 39.37007874015748143 ) ;
#31308 = EDGE_LOOP ( 'NONE', ( #27368, #25301, #2382, #25839 ) ) ;
#31309 = ORIENTED_EDGE ( 'NONE', *, *, #39092, .T. ) ;
#31310 = ORIENTED_EDGE ( 'NONE', *, *, #7848, .T. ) ;
#31311 = DIRECTION ( 'NONE',  ( 1.000000000000000000, 0.000000000000000000, 0.000000000000000000 ) ) ;
#31312 = CARTESIAN_POINT ( 'NONE',  ( -1.439733046521776583, 0.000000000000000000, -1.259842519685034468 ) ) ;
#31313 = VERTEX_POINT ( 'NONE', #39994 ) ;
#31314 = EDGE_LOOP ( 'NONE', ( #1742, #22671, #15348, #28250 ) ) ;
#31315 = CARTESIAN_POINT ( 'NONE',  ( -1.788632549858358844, 3.346456692913386100, 1.220472440944875059 ) ) ;
#31316 = CARTESIAN_POINT ( 'NONE',  ( 1.956903606557731878, 1.706436945410369166, -1.232773380686051690 ) ) ;
#31317 = LINE ( 'NONE', #8069, #6355 ) ;
#31318 = AXIS2_PLACEMENT_3D ( 'NONE', #22209, #44655, #25052 ) ;
#31319 = ORIENTED_EDGE ( 'NONE', *, *, #39791, .T. ) ;
#31320 = ORIENTED_EDGE ( 'NONE', *, *, #35758, .F. ) ;
#31321 = CARTESIAN_POINT ( 'NONE',  ( 0.8338860768354398045, 1.049866565067838264, -1.845005748911692667 ) ) ;
#31322 = LINE ( 'NONE', #50132, #44752 ) ;
#31323 = LINE ( 'NONE', #36219, #38541 ) ;
#31324 = EDGE_LOOP ( 'NONE', ( #3005, #6178, #33567, #50418 ) ) ;
#31325 = CARTESIAN_POINT ( 'NONE',  ( -1.780101451746625152, 0.000000000000000000, 1.234002060668493828 ) ) ;
#31326 = CARTESIAN_POINT ( 'NONE',  ( 0.1968503937007874405, 0.000000000000000000, 0.000000000000000000 ) ) ;
#31327 = VERTEX_POINT ( 'NONE', #4626 ) ;
#31328 = ADVANCED_FACE ( 'NONE', ( #19846 ), #43848, .F. ) ;
#31329 = DIRECTION ( 'NONE',  ( -0.01601477604151182663, 0.9998717552508123996, -0.000000000000000000 ) ) ;
#31330 = VERTEX_POINT ( 'NONE', #32003 ) ;
#31331 = ORIENTED_EDGE ( 'NONE', *, *, #1216, .T. ) ;
#31332 = VECTOR ( 'NONE', #6296, 39.37007874015748143 ) ;
#31333 = DIRECTION ( 'NONE',  ( 1.000000000000000000, -0.000000000000000000, 0.000000000000000000 ) ) ;
#31334 = CARTESIAN_POINT ( 'NONE',  ( 1.636583440222563635, 0.000000000000000000, -1.141732283464564013 ) ) ;
#31335 = ADVANCED_FACE ( 'NONE', ( #51041 ), #50785, .T. ) ;
#31336 = PRODUCT_DEFINITION ( 'UNKNOWN', '', #30028, #30327 ) ;
#31337 = LINE ( 'NONE', #50887, #11564 ) ;
#31338 = EDGE_CURVE ( 'NONE', #15353, #35113, #35103, .T. ) ;
#31339 = CARTESIAN_POINT ( 'NONE',  ( -0.2783729501556720387, 0.02346101323895649626, 1.809574371873096110 ) ) ;
#31340 = EDGE_CURVE ( 'NONE', #33624, #37378, #27090, .T. ) ;
#31341 = CARTESIAN_POINT ( 'NONE',  ( 0.8182917201112819283, 3.346456692913386100, -1.102362204724405714 ) ) ;
#31342 = ORIENTED_EDGE ( 'NONE', *, *, #17996, .T. ) ;
#31343 = ORIENTED_EDGE ( 'NONE', *, *, #27007, .F. ) ;
#31344 = VERTEX_POINT ( 'NONE', #43593 ) ;
#31345 = FACE_OUTER_BOUND ( 'NONE', #38488, .T. ) ;
#31346 = CARTESIAN_POINT ( 'NONE',  ( -1.723188456408593527, 6.692913385826772199, 1.311251662046200472 ) ) ;
#31347 = EDGE_CURVE ( 'NONE', #8483, #19508, #7482, .T. ) ;
#31348 = DIRECTION ( 'NONE',  ( 1.734723475976806848E-16, 0.000000000000000000, 1.000000000000000000 ) ) ;
#31349 = DIRECTION ( 'NONE',  ( 0.5407162030609372616, -0.6444004775717706579, 0.5407162030609374836 ) ) ;
#31350 = ORIENTED_EDGE ( 'NONE', *, *, #41127, .T. ) ;
#31351 = CARTESIAN_POINT ( 'NONE',  ( 0.2727639067037609943, 3.267716535433071279, 1.220472440944875281 ) ) ;
#31352 = ADVANCED_FACE ( 'NONE', ( #20881 ), #33033, .F. ) ;
#31353 = CARTESIAN_POINT ( 'NONE',  ( 1.735113842587030497, 0.05571068913886997875, 0.8778189866238004235 ) ) ;
#31354 = VECTOR ( 'NONE', #12870, 39.37007874015748143 ) ;
#31355 = EDGE_LOOP ( 'NONE', ( #42233, #46560, #29744, #21020 ) ) ;
#31356 = CARTESIAN_POINT ( 'NONE',  ( -0.2727639067037607168, 3.267716535433071279, 4.731699523581612823E-17 ) ) ;
#31357 = CIRCLE ( 'NONE', #33844, 2.165354330708661568 ) ;
#31358 = DIRECTION ( 'NONE',  ( -1.156482317317871478E-16, 0.000000000000000000, -1.000000000000000000 ) ) ;
#31359 = CARTESIAN_POINT ( 'NONE',  ( 2.878724150143186833, 0.000000000000000000, -0.6570500018394808128 ) ) ;
#31360 = ADVANCED_FACE ( 'NONE', ( #48970 ), #12625, .F. ) ;
#31361 = ORIENTED_EDGE ( 'NONE', *, *, #46049, .F. ) ;
#31362 = LINE ( 'NONE', #11486, #48136 ) ;
#31363 = LINE ( 'NONE', #11233, #6041 ) ;
#31364 = DIRECTION ( 'NONE',  ( -0.000000000000000000, 1.000000000000000000, -0.000000000000000000 ) ) ;
#31365 = VERTEX_POINT ( 'NONE', #5392 ) ;
#31366 = FACE_OUTER_BOUND ( 'NONE', #5966, .T. ) ;
#31367 = AXIS2_PLACEMENT_3D ( 'NONE', #17535, #33300, #48224 ) ;
#31368 = VERTEX_POINT ( 'NONE', #17022 ) ;
#31369 = DIRECTION ( 'NONE',  ( 0.000000000000000000, 0.000000000000000000, -1.000000000000000000 ) ) ;
#31370 = EDGE_CURVE ( 'NONE', #11723, #12457, #44110, .T. ) ;
#31371 = DIRECTION ( 'NONE',  ( 0.01601477604151182663, -0.9998717552508123996, 0.000000000000000000 ) ) ;
#31372 = LINE ( 'NONE', #39622, #22709 ) ;
#31373 = VERTEX_POINT ( 'NONE', #1004 ) ;
#31374 = ORIENTED_EDGE ( 'NONE', *, *, #10975, .T. ) ;
#31375 = LINE ( 'NONE', #22364, #37229 ) ;
#31376 = LINE ( 'NONE', #11746, #11446 ) ;
#31377 = ORIENTED_EDGE ( 'NONE', *, *, #39951, .F. ) ;
#31378 = PLANE ( 'NONE',  #36567 ) ;
#31379 = DIRECTION ( 'NONE',  ( -0.000000000000000000, 1.000000000000000000, -0.000000000000000000 ) ) ;
#31380 = DIRECTION ( 'NONE',  ( 0.000000000000000000, 0.000000000000000000, -1.000000000000000000 ) ) ;
#31381 = DIRECTION ( 'NONE',  ( -3.469446951953613696E-16, 0.000000000000000000, -1.000000000000000000 ) ) ;
#31382 = ORIENTED_EDGE ( 'NONE', *, *, #7563, .T. ) ;
#31383 = B_SPLINE_CURVE_WITH_KNOTS ( 'NONE', 3,
 ( #16516, #17286, #33043, #48725 ),
 .UNSPECIFIED., .F., .F.,
 ( 4, 4 ),
 ( 0.0002445083414965676209, 0.0004292220583399663668 ),
 .UNSPECIFIED. ) ;
#31384 = ORIENTED_EDGE ( 'NONE', *, *, #26444, .T. ) ;
#31385 = CARTESIAN_POINT ( 'NONE',  ( 0.8182917201112819283, 3.346456692913386100, 0.5905511811023579360 ) ) ;
#31386 = CARTESIAN_POINT ( 'NONE',  ( 1.091055626815042423, 0.000000000000000000, -1.259842519685035134 ) ) ;
#31387 = ORIENTED_EDGE ( 'NONE', *, *, #24584, .F. ) ;
#31388 = CARTESIAN_POINT ( 'NONE',  ( 2.345377178086121450, 1.748857782376721071, -0.9489428892520402892 ) ) ;
#31389 = VERTEX_POINT ( 'NONE', #12888 ) ;
#31390 = ORIENTED_EDGE ( 'NONE', *, *, #14027, .T. ) ;
#31391 = CARTESIAN_POINT ( 'NONE',  ( -1.985260859929298016, 3.267716535433071279, -0.7037298423582233342 ) ) ;
#31392 = ADVANCED_FACE ( 'NONE', ( #8750 ), #32780, .F. ) ;
#31393 = AXIS2_PLACEMENT_3D ( 'NONE', #13320, #33720, #45044 ) ;
#31394 = CONICAL_SURFACE ( 'NONE', #1692, 3.483074324928249421, 1.244861948955335196 ) ;
#31395 = ORIENTED_EDGE ( 'NONE', *, *, #9491, .F. ) ;
#31396 = ORIENTED_EDGE ( 'NONE', *, *, #3340, .F. ) ;
#31397 = FACE_OUTER_BOUND ( 'NONE', #6947, .T. ) ;
#31398 = EDGE_CURVE ( 'NONE', #40626, #11395, #35296, .T. ) ;
#31399 = ORIENTED_EDGE ( 'NONE', *, *, #25080, .T. ) ;
#31400 = PLANE ( 'NONE',  #25430 ) ;
#31401 = CARTESIAN_POINT ( 'NONE',  ( -1.876501151069718265, 1.583532498426239998, 1.559405008154286953 ) ) ;
#31402 = DIRECTION ( 'NONE',  ( 0.000000000000000000, 1.000000000000000000, 0.000000000000000000 ) ) ;
#31403 =( BOUNDED_CURVE ( )  B_SPLINE_CURVE ( 3, ( #10593, #30208, #10337, #44919 ),
 .UNSPECIFIED., .F., .F. ) 
 B_SPLINE_CURVE_WITH_KNOTS ( ( 4, 4 ),
 ( 3.643597954878999623, 3.694401143243455810 ),
 .UNSPECIFIED. ) 
 CURVE ( )  GEOMETRIC_REPRESENTATION_ITEM ( )  RATIONAL_B_SPLINE_CURVE ( ( 1.000000000000000000, 0.9997849312356386076, 0.9997849312356386076, 1.000000000000000000 ) ) 
 REPRESENTATION_ITEM ( '' )  );
#31404 = LINE ( 'NONE', #27514, #21480 ) ;
#31405 = CARTESIAN_POINT ( 'NONE',  ( -0.6214413264104945434, 3.346456692913386100, 0.1574803149606285035 ) ) ;
#31406 = CARTESIAN_POINT ( 'NONE',  ( 1.613190494119344232, 1.049866565067837820, 1.223531214289272695 ) ) ;
#31407 = VERTEX_POINT ( 'NONE', #16763 ) ;
#31408 = CARTESIAN_POINT ( 'NONE',  ( 1.363819533518803251, 3.267716535433071279, -0.1574803149606304187 ) ) ;
#31409 = CARTESIAN_POINT ( 'NONE',  ( 2.361042194882304379, 3.267716535433071279, 0.6299212598425161236 ) ) ;
#31410 = PLANE ( 'NONE',  #30619 ) ;
#31411 = ORIENTED_EDGE ( 'NONE', *, *, #22776, .T. ) ;
#31412 = DIRECTION ( 'NONE',  ( -1.000000000000000000, 0.000000000000000000, 0.000000000000000000 ) ) ;
#31413 = CARTESIAN_POINT ( 'NONE',  ( -0.7582255214199161708, 0.000000000000000000, -1.687894986714875811 ) ) ;
#31414 = VERTEX_POINT ( 'NONE', #24507 ) ;
#31415 = DIRECTION ( 'NONE',  ( 1.734723475976806848E-16, 0.000000000000000000, 1.000000000000000000 ) ) ;
#31416 = ADVANCED_FACE ( 'NONE', ( #5135 ), #41026, .F. ) ;
#31417 = DIRECTION ( 'NONE',  ( 1.000000000000000000, 0.000000000000000000, 0.000000000000000000 ) ) ;
#31418 = FACE_OUTER_BOUND ( 'NONE', #49407, .T. ) ;
#31419 = CARTESIAN_POINT ( 'NONE',  ( 1.905671854841464175, 0.000000000000000000, 2.256015092822681645 ) ) ;
#31420 = ORIENTED_EDGE ( 'NONE', *, *, #22288, .T. ) ;
#31421 = CARTESIAN_POINT ( 'NONE',  ( 1.139183960333101098, 3.346456692913386100, -1.771653543307081691 ) ) ;
#31422 = EDGE_CURVE ( 'NONE', #16438, #27482, #16806, .T. ) ;
#31423 = CARTESIAN_POINT ( 'NONE',  ( -1.091055626815042645, 0.000000000000000000, -0.3149606299212593941 ) ) ;
#31424 = CIRCLE ( 'NONE', #1724, 2.165354330708661568 ) ;
#31425 = VECTOR ( 'NONE', #14115, 39.37007874015748143 ) ;
#31426 = ADVANCED_FACE ( 'NONE', ( #48213 ), #20625, .T. ) ;
#31427 = CARTESIAN_POINT ( 'NONE',  ( 2.531258147843939089E-16, 0.000000000000000000, 2.066929133858268042 ) ) ;
#31428 = LINE ( 'NONE', #19537, #17738 ) ;
#31429 = EDGE_LOOP ( 'NONE', ( #35099, #28590, #41491, #3932 ) ) ;
#31430 = EDGE_CURVE ( 'NONE', #50129, #4115, #24761, .T. ) ;
#31431 = VERTEX_POINT ( 'NONE', #25520 ) ;
#31432 = ORIENTED_EDGE ( 'NONE', *, *, #29471, .F. ) ;
#31433 = CARTESIAN_POINT ( 'NONE',  ( 1.255350140850374441, 0.03167824151409264627, 1.511661998497999537 ) ) ;
#31434 = EDGE_LOOP ( 'NONE', ( #27675, #18629, #43468, #19815 ) ) ;
#31435 = EDGE_CURVE ( 'NONE', #29680, #2567, #48461, .T. ) ;
#31436 = CARTESIAN_POINT ( 'NONE',  ( 0.000000000000000000, 3.267716535433071279, -0.3543307086614175816 ) ) ;
#31437 = AXIS2_PLACEMENT_3D ( 'NONE', #8647, #43742, #24142 ) ;
#31438 = CARTESIAN_POINT ( 'NONE',  ( 0.5455278134075208785, 0.000000000000000000, -1.889763779527552812 ) ) ;
#31439 = VERTEX_POINT ( 'NONE', #9522 ) ;
#31440 = EDGE_CURVE ( 'NONE', #12590, #19157, #29393, .T. ) ;
#31441 = PLANE ( 'NONE',  #47829 ) ;
#31442 = CONICAL_SURFACE ( 'NONE', #39695, 1.850107469027523210, 0.6386652850508578450 ) ;
#31443 = EDGE_LOOP ( 'NONE', ( #21306, #40337, #4130, #7762 ) ) ;
#31444 = CARTESIAN_POINT ( 'NONE',  ( 0.000000000000000000, 3.267716535433071279, 0.2755905511810995412 ) ) ;
#31445 = B_SPLINE_CURVE_WITH_KNOTS ( 'NONE', 3,
 ( #49911, #26462, #42713, #30348 ),
 .UNSPECIFIED., .F., .F.,
 ( 4, 4 ),
 ( 0.0006330831653206172183, 0.004889894717019593537 ),
 .UNSPECIFIED. ) ;
#31446 = DIRECTION ( 'NONE',  ( 0.000000000000000000, -1.000000000000000000, -0.000000000000000000 ) ) ;
#31447 = EDGE_LOOP ( 'NONE', ( #8844, #12521, #29174, #33075 ) ) ;
#31448 = ORIENTED_EDGE ( 'NONE', *, *, #36957, .T. ) ;
#31449 = LINE ( 'NONE', #47145, #4275 ) ;
#31450 = ORIENTED_EDGE ( 'NONE', *, *, #36085, .T. ) ;
#31451 = EDGE_CURVE ( 'NONE', #48631, #24742, #10300, .T. ) ;
#31452 = CARTESIAN_POINT ( 'NONE',  ( 1.636583440222563857, 0.000000000000000000, 0.3149606299212576177 ) ) ;
#31453 = ORIENTED_EDGE ( 'NONE', *, *, #17998, .T. ) ;
#31454 = ORIENTED_EDGE ( 'NONE', *, *, #43889, .T. ) ;
#31455 = ADVANCED_FACE ( 'NONE', ( #21399 ), #15142, .T. ) ;
#31456 = CARTESIAN_POINT ( 'NONE',  ( 1.909347346926324684, 3.346456692913386100, -0.03937007874015936021 ) ) ;
#31457 = CARTESIAN_POINT ( 'NONE',  ( -1.843346842069858216, 1.645568979423359446, -1.157815216737156483 ) ) ;
#31458 = VERTEX_POINT ( 'NONE', #36126 ) ;
#31459 = CARTESIAN_POINT ( 'NONE',  ( -0.07591351300297327631, 3.267716535433071279, 2.633779063002566366E-17 ) ) ;
#31460 = ORIENTED_EDGE ( 'NONE', *, *, #17885, .F. ) ;
#31461 = CARTESIAN_POINT ( 'NONE',  ( 1.091055626815042423, 3.346456692913386100, -1.259842519685035134 ) ) ;
#31462 = AXIS2_PLACEMENT_3D ( 'NONE', #16436, #2218, #22095 ) ;
#31463 = CARTESIAN_POINT ( 'NONE',  ( 1.560669927219590525, 3.267716535433071279, 0.9055118110236164419 ) ) ;
#31464 = CONICAL_SURFACE ( 'NONE', #1797, 3.483074324928249421, 1.244861948955335196 ) ;
#31465 = FACE_OUTER_BOUND ( 'NONE', #7009, .T. ) ;
#31466 = EDGE_LOOP ( 'NONE', ( #23327, #13172, #37109, #2055 ) ) ;
#31467 = ORIENTED_EDGE ( 'NONE', *, *, #34303, .T. ) ;
#31468 = VECTOR ( 'NONE', #33172, 39.37007874015748143 ) ;
#31469 = CARTESIAN_POINT ( 'NONE',  ( 1.068075307999460488, 1.574803149606302854, 1.883606783264653028 ) ) ;
#31470 = LINE ( 'NONE', #11088, #46848 ) ;
#31471 = LINE ( 'NONE', #11839, #32413 ) ;
#31472 = VECTOR ( 'NONE', #6690, 39.37007874015748143 ) ;
#31473 = DIRECTION ( 'NONE',  ( 1.734723475976806848E-16, -0.000000000000000000, 1.000000000000000000 ) ) ;
#31474 = PLANE ( 'NONE',  #4183 ) ;
#31475 = AXIS2_PLACEMENT_3D ( 'NONE', #2913, #2409, #34661 ) ;
#31476 = CARTESIAN_POINT ( 'NONE',  ( -0.07591351300297363713, 3.267716535433071279, -2.164023224473873963 ) ) ;
#31477 = ORIENTED_EDGE ( 'NONE', *, *, #43547, .T. ) ;
#31478 = ADVANCED_FACE ( 'NONE', ( #755 ), #32256, .F. ) ;
#31479 = DIRECTION ( 'NONE',  ( -3.469446951953613696E-16, 0.000000000000000000, -1.000000000000000000 ) ) ;
#31480 = VERTEX_POINT ( 'NONE', #30666 ) ;
#31481 = CARTESIAN_POINT ( 'NONE',  ( 0.000000000000000000, 3.346456692913386100, 0.000000000000000000 ) ) ;
#31482 = ORIENTED_EDGE ( 'NONE', *, *, #5250, .F. ) ;
#31483 = CARTESIAN_POINT ( 'NONE',  ( -1.091055626815042201, 3.267716535433071279, 0.9448818897637749625 ) ) ;
#31484 = FACE_OUTER_BOUND ( 'NONE', #38989, .T. ) ;
#31485 = ADVANCED_FACE ( 'NONE', ( #29905 ), #46378, .F. ) ;
#31486 = EDGE_LOOP ( 'NONE', ( #48046, #20479, #10373, #5729 ) ) ;
#31487 = EDGE_CURVE ( 'NONE', #37100, #2160, #41779, .T. ) ;
#31488 = EDGE_CURVE ( 'NONE', #45769, #40209, #27864, .T. ) ;
#31489 = CARTESIAN_POINT ( 'NONE',  ( 0.2727639067037609943, 3.267716535433071279, 2.165354330708650910 ) ) ;
#31490 = ORIENTED_EDGE ( 'NONE', *, *, #6210, .F. ) ;
#31491 = CARTESIAN_POINT ( 'NONE',  ( 2.327376634978634673, 0.9888095434482767621, 1.196529185699396036 ) ) ;
#31492 = ORIENTED_EDGE ( 'NONE', *, *, #1701, .T. ) ;
#31493 = CARTESIAN_POINT ( 'NONE',  ( 1.363819533518803251, 0.000000000000000000, 0.7874015748031454320 ) ) ;
#31494 = DIRECTION ( 'NONE',  ( -3.469446951953613696E-16, 0.000000000000000000, -1.000000000000000000 ) ) ;
#31495 = CIRCLE ( 'NONE', #34781, 2.246510896728926010 ) ;
#31496 = ORIENTED_EDGE ( 'NONE', *, *, #16667, .F. ) ;
#31497 = CONICAL_SURFACE ( 'NONE', #9247, 3.033577403570480779, 1.554780866114618743 ) ;
#31498 = CARTESIAN_POINT ( 'NONE',  ( 0.1250607540065018508, 1.205361022782829114E-17, -1.938545675207280272 ) ) ;
#31499 = VERTEX_POINT ( 'NONE', #2792 ) ;
#31500 = ORIENTED_EDGE ( 'NONE', *, *, #15716, .F. ) ;
#31501 = CARTESIAN_POINT ( 'NONE',  ( 1.526813663045976766, 0.5226730630971984093, 1.672780703928434143 ) ) ;
#31503 = CARTESIAN_POINT ( 'NONE',  ( 1.091055626815042645, 3.346456692913386100, -1.141732283464564013 ) ) ;
#31502 = VECTOR ( 'NONE', #30318, 39.37007874015748143 ) ;
#31504 = LINE ( 'NONE', #30497, #48236 ) ;
#31505 = EDGE_CURVE ( 'NONE', #29688, #27355, #45618, .T. ) ;
#31506 = VECTOR ( 'NONE', #42777, 39.37007874015748143 ) ;
#31507 = ORIENTED_EDGE ( 'NONE', *, *, #50492, .T. ) ;
#31508 = EDGE_CURVE ( 'NONE', #48466, #28575, #18793, .T. ) ;
#31509 = CARTESIAN_POINT ( 'NONE',  ( 0.07982360342473591996, 1.709180471932028711, 0.000000000000000000 ) ) ;
#31510 = CARTESIAN_POINT ( 'NONE',  ( 0.000000000000000000, 0.000000000000000000, 0.000000000000000000 ) ) ;
#31511 = VERTEX_POINT ( 'NONE', #37409 ) ;
#31512 = ADVANCED_FACE ( 'NONE', ( #25773 ), #14411, .F. ) ;
#31513 = DIRECTION ( 'NONE',  ( 0.000000000000000000, -1.000000000000000000, 0.000000000000000000 ) ) ;
#31514 = EDGE_CURVE ( 'NONE', #14497, #850, #37666, .T. ) ;
#31515 = B_SPLINE_CURVE_WITH_KNOTS ( 'NONE', 3,
 ( #413, #44535, #8931, #24166 ),
 .UNSPECIFIED., .F., .F.,
 ( 4, 4 ),
 ( 0.001649814413565570993, 0.04583418734355550889 ),
 .UNSPECIFIED. ) ;
#31516 = ADVANCED_FACE ( 'NONE', ( #2284 ), #49983, .F. ) ;
#31517 = ORIENTED_EDGE ( 'NONE', *, *, #20694, .T. ) ;
#31518 = VERTEX_POINT ( 'NONE', #45875 ) ;
#31519 = CONTEXT_DEPENDENT_SHAPE_REPRESENTATION ( #27578, #38833 ) ;
#31520 = VERTEX_POINT ( 'NONE', #18033 ) ;
#31521 = CARTESIAN_POINT ( 'NONE',  ( -2.142805232260985182, 6.692913385826772199, 0.3399247426648309700 ) ) ;
#31522 = LINE ( 'NONE', #27374, #43948 ) ;
#31523 = LINE ( 'NONE', #27129, #34393 ) ;
#31524 = LINE ( 'NONE', #50083, #21411 ) ;
#31525 = ORIENTED_EDGE ( 'NONE', *, *, #6771, .F. ) ;
#31526 = ORIENTED_EDGE ( 'NONE', *, *, #31732, .T. ) ;
#31527 = FACE_OUTER_BOUND ( 'NONE', #18024, .T. ) ;
#31528 = LINE ( 'NONE', #46481, #35011 ) ;
#31529 = ORIENTED_EDGE ( 'NONE', *, *, #41261, .T. ) ;
#31530 = CARTESIAN_POINT ( 'NONE',  ( 0.1968503937007873850, 0.000000000000000000, -0.1968503937007874405 ) ) ;
#31531 = LINE ( 'NONE', #14589, #872 ) ;
#31532 = AXIS2_PLACEMENT_3D ( 'NONE', #46219, #10878, #42362 ) ;
#31533 = DIRECTION ( 'NONE',  ( -0.000000000000000000, -1.000000000000000000, 0.000000000000000000 ) ) ;
#31534 = CARTESIAN_POINT ( 'NONE',  ( -0.3486774197067347147, 3.267716535433071279, 1.209717811016581790E-16 ) ) ;
#31536 = CARTESIAN_POINT ( 'NONE',  ( 1.083598637574782142, 1.491270273546293046, 2.747180975113346246 ) ) ;
#31535 = VECTOR ( 'NONE', #29615, 39.37007874015748143 ) ;
#31537 = ORIENTED_EDGE ( 'NONE', *, *, #4126, .T. ) ;
#31538 = CARTESIAN_POINT ( 'NONE',  ( -0.2727639067037607723, 3.346456692913386100, -1.102362204724405714 ) ) ;
#31539 = DIRECTION ( 'NONE',  ( 1.000000000000000000, 0.000000000000000000, 0.000000000000000000 ) ) ;
#31540 = VECTOR ( 'NONE', #2122, 39.37007874015748143 ) ;
#31541 = ORIENTED_EDGE ( 'NONE', *, *, #9700, .T. ) ;
#31542 = VECTOR ( 'NONE', #23265, 39.37007874015748143 ) ;
#31543 = ORIENTED_EDGE ( 'NONE', *, *, #26216, .T. ) ;
#31544 = VECTOR ( 'NONE', #17569, 39.37007874015748143 ) ;
#31545 = DIRECTION ( 'NONE',  ( 0.000000000000000000, 0.000000000000000000, 1.000000000000000000 ) ) ;
#31546 = LINE ( 'NONE', #4428, #9688 ) ;
#31547 = CARTESIAN_POINT ( 'NONE',  ( 1.738729679588007171, 0.000000000000000000, -0.1273486421339826147 ) ) ;
#31548 = ORIENTED_EDGE ( 'NONE', *, *, #48938, .F. ) ;
#31549 = ADVANCED_FACE ( 'NONE', ( #42276 ), #2031, .F. ) ;
#31550 = ADVANCED_FACE ( 'NONE', ( #14667 ), #50228, .F. ) ;
#31551 = ORIENTED_EDGE ( 'NONE', *, *, #37671, .T. ) ;
#31552 = FACE_OUTER_BOUND ( 'NONE', #36569, .T. ) ;
#31553 = EDGE_LOOP ( 'NONE', ( #6383, #11808, #32738, #18342 ) ) ;
#31554 = CARTESIAN_POINT ( 'NONE',  ( 1.015142113812069313, 0.000000000000000000, -1.102362204724405714 ) ) ;
#31555 = EDGE_CURVE ( 'NONE', #27703, #49324, #26030, .T. ) ;
#31556 = ORIENTED_EDGE ( 'NONE', *, *, #3887, .T. ) ;
#31557 = DIRECTION ( 'NONE',  ( -0.9998717552508121775, -0.01601477604151182663, 0.000000000000000000 ) ) ;
#31558 = CARTESIAN_POINT ( 'NONE',  ( -0.6529837180168073241, 0.8335264911517249464, -0.6529837180168078792 ) ) ;
#31559 = CARTESIAN_POINT ( 'NONE',  ( 1.953585199828835828, 3.267716535433071279, 0.7874015748031456541 ) ) ;
#31560 = ORIENTED_EDGE ( 'NONE', *, *, #14546, .F. ) ;
#31561 = ORIENTED_EDGE ( 'NONE', *, *, #16826, .T. ) ;
#31562 = ORIENTED_EDGE ( 'NONE', *, *, #184, .T. ) ;
#31563 = LINE ( 'NONE', #35949, #33188 ) ;
#31564 = DIRECTION ( 'NONE',  ( -0.000000000000000000, 1.000000000000000000, -0.000000000000000000 ) ) ;
#31565 = VERTEX_POINT ( 'NONE', #14155 ) ;
#31566 = ORIENTED_EDGE ( 'NONE', *, *, #295, .F. ) ;
#31567 = CARTESIAN_POINT ( 'NONE',  ( 0.000000000000000000, 3.267716535433071279, 0.000000000000000000 ) ) ;
#31568 = CYLINDRICAL_SURFACE ( 'NONE', #12900, 2.165354330708661568 ) ;
#31569 = DIRECTION ( 'NONE',  ( 1.734723475976806848E-16, -0.000000000000000000, 1.000000000000000000 ) ) ;
#31570 = ORIENTED_EDGE ( 'NONE', *, *, #16352, .T. ) ;
#31571 = EDGE_LOOP ( 'NONE', ( #27815, #13518, #37454, #12315 ) ) ;
#31572 = EDGE_CURVE ( 'NONE', #24144, #25794, #48685, .T. ) ;
#31573 = CARTESIAN_POINT ( 'NONE',  ( -1.636583440222564301, 3.346456692913386100, -0.3149606299212592275 ) ) ;
#31574 = CARTESIAN_POINT ( 'NONE',  ( 0.3958187006869922642, 1.717958654416033681, 2.456753799658804915 ) ) ;
#31575 = LINE ( 'NONE', #32097, #26987 ) ;
#31576 = ORIENTED_EDGE ( 'NONE', *, *, #12384, .F. ) ;
#31577 = DIRECTION ( 'NONE',  ( 0.5508969814520945363, -1.160734090543304660E-16, 0.8345732537213079727 ) ) ;
#31578 = VECTOR ( 'NONE', #29802, 39.37007874015748143 ) ;
#31579 = CARTESIAN_POINT ( 'NONE',  ( -1.091055626815042645, 3.232777166330607521, 2.204724409448808764 ) ) ;
#31580 = ORIENTED_EDGE ( 'NONE', *, *, #36162, .F. ) ;
#31581 = EDGE_CURVE ( 'NONE', #18573, #12446, #22165, .T. ) ;
#31582 = FACE_OUTER_BOUND ( 'NONE', #17460, .T. ) ;
#31583 = EDGE_LOOP ( 'NONE', ( #18513, #30721, #20048 ) ) ;
#31584 = ORIENTED_EDGE ( 'NONE', *, *, #11557, .T. ) ;
#31585 = CARTESIAN_POINT ( 'NONE',  ( 0.000000000000000000, 3.267716535433071279, -1.771653543307081025 ) ) ;
#31586 = DIRECTION ( 'NONE',  ( 1.000000000000000000, 0.000000000000000000, -0.000000000000000000 ) ) ;
#31587 = VECTOR ( 'NONE', #47729, 39.37007874015748143 ) ;
#31588 = VECTOR ( 'NONE', #29701, 39.37007874015748143 ) ;
#31589 = CARTESIAN_POINT ( 'NONE',  ( -0.4460728916448887249, 1.700757277111965449, 2.182451250484750638 ) ) ;
#31590 = B_SPLINE_CURVE_WITH_KNOTS ( 'NONE', 3,
 ( #2565, #13174, #25802, #41808 ),
 .UNSPECIFIED., .F., .F.,
 ( 4, 4 ),
 ( 0.001265363855408508167, 0.003765594348430528499 ),
 .UNSPECIFIED. ) ;
#31591 = LINE ( 'NONE', #43951, #18731 ) ;
#31592 = DIRECTION ( 'NONE',  ( -0.01601477604151182663, 0.9998717552508123996, -0.000000000000000000 ) ) ;
#31593 = ORIENTED_EDGE ( 'NONE', *, *, #1893, .F. ) ;
#31594 = ORIENTED_EDGE ( 'NONE', *, *, #4703, .F. ) ;
#31595 = AXIS2_PLACEMENT_3D ( 'NONE', #26265, #42015, #38154 ) ;
#31596 = EDGE_LOOP ( 'NONE', ( #48274, #27185, #7794, #27065 ) ) ;
#31597 = DIRECTION ( 'NONE',  ( -0.000000000000000000, 1.000000000000000000, -0.000000000000000000 ) ) ;
#31598 = DIRECTION ( 'NONE',  ( -0.9998717552508121775, -0.01601477604151182316, 0.000000000000000000 ) ) ;
#31599 = DIRECTION ( 'NONE',  ( -0.000000000000000000, 0.000000000000000000, 1.000000000000000000 ) ) ;
#31600 = CARTESIAN_POINT ( 'NONE',  ( 2.378961647330872786, 3.346456692913386100, -0.3149606299212596716 ) ) ;
#31601 = ORIENTED_EDGE ( 'NONE', *, *, #13043, .T. ) ;
#31602 = CARTESIAN_POINT ( 'NONE',  ( 0.000000000000000000, 3.267716535433071279, 0.000000000000000000 ) ) ;
#31603 = DIRECTION ( 'NONE',  ( 1.000000000000000000, -0.000000000000000000, 0.000000000000000000 ) ) ;
#31604 = ORIENTED_EDGE ( 'NONE', *, *, #47852, .F. ) ;
#31605 = DIRECTION ( 'NONE',  ( -1.000000000000000000, 0.000000000000000000, 0.000000000000000000 ) ) ;
#31606 = CARTESIAN_POINT ( 'NONE',  ( -0.8987785766980536106, 1.205361022782829114E-17, 1.600251783270283390 ) ) ;
#31607 = CARTESIAN_POINT ( 'NONE',  ( 0.000000000000000000, 6.692913385826772199, 0.000000000000000000 ) ) ;
#31608 = VERTEX_POINT ( 'NONE', #38419 ) ;
#31609 = LINE ( 'NONE', #16379, #22639 ) ;
#31610 = CARTESIAN_POINT ( 'NONE',  ( 1.091055626815042423, 0.000000000000000000, -1.889763779527552368 ) ) ;
#31611 = DIRECTION ( 'NONE',  ( 0.000000000000000000, -1.000000000000000000, 0.000000000000000000 ) ) ;
#31612 = ADVANCED_FACE ( 'NONE', ( #3044 ), #14918, .T. ) ;
#31613 = EDGE_CURVE ( 'NONE', #3678, #14290, #16191, .T. ) ;
#31614 = VERTEX_POINT ( 'NONE', #27793 ) ;
#31615 = VECTOR ( 'NONE', #1708, 39.37007874015748143 ) ;
#31616 = FACE_OUTER_BOUND ( 'NONE', #28006, .T. ) ;
#31617 = ORIENTED_EDGE ( 'NONE', *, *, #38433, .T. ) ;
#31618 = LINE ( 'NONE', #47320, #8908 ) ;
#31619 = ADVANCED_FACE ( 'NONE', ( #7174 ), #35553, .F. ) ;
#31620 = AXIS2_PLACEMENT_3D ( 'NONE', #46167, #7214, #31211 ) ;
#31621 = AXIS2_PLACEMENT_3D ( 'NONE', #43703, #8358, #38898 ) ;
#31622 = CARTESIAN_POINT ( 'NONE',  ( -1.133754555558240673, 0.009760511380980992774, 1.372484652545675532 ) ) ;
#31623 = FACE_OUTER_BOUND ( 'NONE', #27561, .T. ) ;
#31624 = CARTESIAN_POINT ( 'NONE',  ( -2.454875160333845674, 3.346456692913386100, 0.1574803149606286423 ) ) ;
#31625 = ORIENTED_EDGE ( 'NONE', *, *, #29275, .T. ) ;
#31626 = EDGE_LOOP ( 'NONE', ( #38979, #32971, #41622, #7317 ) ) ;
#31627 = CARTESIAN_POINT ( 'NONE',  ( -0.5756566573089003658, 1.611847391933241669, 2.896516654582634853 ) ) ;
#31628 = AXIS2_PLACEMENT_3D ( 'NONE', #50161, #50406, #23091 ) ;
#31629 = CARTESIAN_POINT ( 'NONE',  ( 2.106197740627111514, 3.346456692913386100, -0.7874015748031473194 ) ) ;
#31630 = ORIENTED_EDGE ( 'NONE', *, *, #24815, .T. ) ;
#31631 = CARTESIAN_POINT ( 'NONE',  ( 0.2727639067037604947, 3.267716535433071279, -0.1574803149606298636 ) ) ;
#31632 = CARTESIAN_POINT ( 'NONE',  ( 1.735586374879370952, 0.000000000000000000, -2.388829707800026458 ) ) ;
#31633 = CARTESIAN_POINT ( 'NONE',  ( -1.091055626815042645, 0.000000000000000000, -2.086614173228339641 ) ) ;
#31634 = LINE ( 'NONE', #27746, #14931 ) ;
#31635 = EDGE_LOOP ( 'NONE', ( #27309, #41347, #29839, #40502 ) ) ;
#31636 = ORIENTED_EDGE ( 'NONE', *, *, #21195, .T. ) ;
#31637 = ADVANCED_FACE ( 'NONE', ( #7426 ), #23161, .T. ) ;
#31638 = ORIENTED_EDGE ( 'NONE', *, *, #24447, .F. ) ;
#31639 = CARTESIAN_POINT ( 'NONE',  ( -0.3486774197067339376, 3.346456692913386100, -0.9448818897637762948 ) ) ;
#31640 = DIRECTION ( 'NONE',  ( -1.000000000000000000, 0.000000000000000000, 1.734723475976806848E-16 ) ) ;
#31641 = LINE ( 'NONE', #47340, #17465 ) ;
#31642 = ORIENTED_EDGE ( 'NONE', *, *, #31225, .T. ) ;
#31643 = EDGE_CURVE ( 'NONE', #1464, #1640, #23475, .T. ) ;
#31644 = LINE ( 'NONE', #11762, #9252 ) ;
#31645 = ORIENTED_EDGE ( 'NONE', *, *, #16214, .T. ) ;
#31646 = VERTEX_POINT ( 'NONE', #43283 ) ;
#31647 = CARTESIAN_POINT ( 'NONE',  ( 0.000000000000000000, 0.000000000000000000, -1.220472440944881942 ) ) ;
#31648 = ORIENTED_EDGE ( 'NONE', *, *, #23845, .F. ) ;
#31649 = ORIENTED_EDGE ( 'NONE', *, *, #38723, .F. ) ;
#31650 = DIRECTION ( 'NONE',  ( 1.000000000000000000, 0.000000000000000000, 0.000000000000000000 ) ) ;
#31651 = ORIENTED_EDGE ( 'NONE', *, *, #17402, .T. ) ;
#31652 = AXIS2_PLACEMENT_3D ( 'NONE', #7642, #39135, #27761 ) ;
#31653 = VECTOR ( 'NONE', #29171, 39.37007874015748854 ) ;
#31654 = AXIS2_PLACEMENT_3D ( 'NONE', #495, #3608, #50535 ) ;
#31655 = PLANE ( 'NONE',  #38633 ) ;
#31656 = EDGE_CURVE ( 'NONE', #11744, #643, #7486, .T. ) ;
#31657 = CARTESIAN_POINT ( 'NONE',  ( -0.2727639067037608278, 3.267716535433071279, -0.6692913385826758654 ) ) ;
#31658 = DIRECTION ( 'NONE',  ( -0.000000000000000000, -1.000000000000000000, 0.000000000000000000 ) ) ;
#31659 = VECTOR ( 'NONE', #26653, 39.37007874015748143 ) ;
#31660 = ADVANCED_BREP_SHAPE_REPRESENTATION ( '', ( #24040, #26741 ), #13567 ) ;
#31661 = VECTOR ( 'NONE', #2342, 39.37007874015748143 ) ;
#31662 = LINE ( 'NONE', #16429, #1691 ) ;
#31663 = CARTESIAN_POINT ( 'NONE',  ( 1.091055626815042645, 0.000000000000000000, 0.7480314960629872445 ) ) ;
#31664 = CARTESIAN_POINT ( 'NONE',  ( 0.3820226255272446414, 0.03403845698394380309, 1.829505193364920679 ) ) ;
#31665 = VECTOR ( 'NONE', #553, 39.37007874015748143 ) ;
#31666 = ORIENTED_EDGE ( 'NONE', *, *, #2496, .F. ) ;
#31667 = FACE_OUTER_BOUND ( 'NONE', #21175, .T. ) ;
#31668 = CARTESIAN_POINT ( 'NONE',  ( 0.8660835963268131987, 1.007957364116236709, 2.447728759293120504 ) ) ;
#31669 = CARTESIAN_POINT ( 'NONE',  ( 1.287906020515829919, 3.267716535433071279, -1.574803149606294417 ) ) ;
#31670 = VERTEX_POINT ( 'NONE', #20042 ) ;
#31671 = DIRECTION ( 'NONE',  ( -0.000000000000000000, 1.000000000000000000, -0.000000000000000000 ) ) ;
#31672 = DIRECTION ( 'NONE',  ( -3.469446951953613696E-16, 0.000000000000000000, -1.000000000000000000 ) ) ;
#31673 = EDGE_LOOP ( 'NONE', ( #45633, #6804, #35137, #4145 ) ) ;
#31674 = DIRECTION ( 'NONE',  ( -0.9195277725514489076, 0.000000000000000000, -0.3930250316539278255 ) ) ;
#31675 = DIRECTION ( 'NONE',  ( 1.000000000000000000, 0.000000000000000000, 0.000000000000000000 ) ) ;
#31676 = DIRECTION ( 'NONE',  ( 0.000000000000000000, -1.000000000000000000, 0.000000000000000000 ) ) ;
#31677 = CARTESIAN_POINT ( 'NONE',  ( -0.04921259842519689481, 2.794703227806734062E-17, 1.924024829198930364 ) ) ;
#31678 = ORIENTED_EDGE ( 'NONE', *, *, #3000, .T. ) ;
#31679 = CARTESIAN_POINT ( 'NONE',  ( -0.7874015748031497619, 6.389997247649651107E-17, -0.7480314960629921295 ) ) ;
#31680 = EDGE_CURVE ( 'NONE', #40996, #7498, #15925, .T. ) ;
#31681 = FACE_OUTER_BOUND ( 'NONE', #48220, .T. ) ;
#31682 = DIRECTION ( 'NONE',  ( -0.000000000000000000, 1.000000000000000000, -0.000000000000000000 ) ) ;
#31684 = ADVANCED_FACE ( 'NONE', ( #12317 ), #37461, .T. ) ;
#31683 = DIRECTION ( 'NONE',  ( -1.000000000000000000, 0.000000000000000000, 1.734723475976806848E-16 ) ) ;
#31685 = ORIENTED_EDGE ( 'NONE', *, *, #44921, .T. ) ;
#31686 = ADVANCED_FACE ( 'NONE', ( #31681 ), #20931, .T. ) ;
#31687 = ORIENTED_EDGE ( 'NONE', *, *, #24911, .F. ) ;
#31688 = ORIENTED_EDGE ( 'NONE', *, *, #27685, .T. ) ;
#31689 = VECTOR ( 'NONE', #11471, 39.37007874015748143 ) ;
#31690 = CARTESIAN_POINT ( 'NONE',  ( 1.887300604142603921, 1.205361022782829114E-17, 0.9597141752041703500 ) ) ;
#31691 = ORIENTED_EDGE ( 'NONE', *, *, #26473, .F. ) ;
#31692 = CARTESIAN_POINT ( 'NONE',  ( 1.621795816027391979, 0.000000000000000000, -0.6396693727619211511 ) ) ;
#31693 = VECTOR ( 'NONE', #14100, 39.37007874015748854 ) ;
#31694 = DIRECTION ( 'NONE',  ( -0.9998717552508122886, -0.01601477604151182316, 0.000000000000000000 ) ) ;
#31695 = ORIENTED_EDGE ( 'NONE', *, *, #31167, .F. ) ;
#31696 = AXIS2_PLACEMENT_3D ( 'NONE', #23164, #34797, #15672 ) ;
#31697 = AXIS2_PLACEMENT_3D ( 'NONE', #34037, #22657, #25512 ) ;
#31698 = CARTESIAN_POINT ( 'NONE',  ( -0.8182917201112819283, 0.000000000000000000, -1.417322834645664331 ) ) ;
#31699 = EDGE_CURVE ( 'NONE', #24770, #22865, #11796, .T. ) ;
#31700 = ORIENTED_EDGE ( 'NONE', *, *, #5112, .F. ) ;
#31701 = CARTESIAN_POINT ( 'NONE',  ( -1.080407128511521764, 1.049866565877817237, 1.712347114401022274 ) ) ;
#31702 = CARTESIAN_POINT ( 'NONE',  ( 1.015142113812069313, 3.346456692913386100, -0.4724409448818889246 ) ) ;
#31703 = CIRCLE ( 'NONE', #30896, 2.106299212598425008 ) ;
#31704 = VERTEX_POINT ( 'NONE', #19033 ) ;
#31705 = ORIENTED_EDGE ( 'NONE', *, *, #4478, .T. ) ;
#31706 = DIRECTION ( 'NONE',  ( -0.01601477604151182663, 0.9998717552508123996, -0.000000000000000000 ) ) ;
#31707 = ORIENTED_EDGE ( 'NONE', *, *, #46492, .F. ) ;
#31708 = CARTESIAN_POINT ( 'NONE',  ( 1.426808618753927282, 0.05077261674489902399, -1.296082183384024811 ) ) ;
#31709 =( BOUNDED_CURVE ( )  B_SPLINE_CURVE ( 3, ( #48865, #9676, #37306, #33692 ),
 .UNSPECIFIED., .F., .F. ) 
 B_SPLINE_CURVE_WITH_KNOTS ( ( 4, 4 ),
 ( 3.141592653589793116, 3.207290069758609974 ),
 .UNSPECIFIED. ) 
 CURVE ( )  GEOMETRIC_REPRESENTATION_ITEM ( )  RATIONAL_B_SPLINE_CURVE ( ( 1.000000000000000000, 0.9996403531335149584, 0.9996403531335149584, 1.000000000000000000 ) ) 
 REPRESENTATION_ITEM ( '' )  );
#31710 = ADVANCED_FACE ( 'NONE', ( #34794 ), #49739, .F. ) ;
#31711 = ORIENTED_EDGE ( 'NONE', *, *, #8204, .T. ) ;
#31712 = ORIENTED_EDGE ( 'NONE', *, *, #6132, .F. ) ;
#31713 = LINE ( 'NONE', #2457, #50341 ) ;
#31714 = CARTESIAN_POINT ( 'NONE',  ( 4.268512490100411402E-16, 3.267716535433071279, 1.574803149606291974 ) ) ;
#31715 = EDGE_LOOP ( 'NONE', ( #32498, #20060, #26305, #46862 ) ) ;
#31716 = FACE_OUTER_BOUND ( 'NONE', #45032, .T. ) ;
#31717 = EDGE_CURVE ( 'NONE', #25302, #41810, #11850, .T. ) ;
#31718 = ORIENTED_EDGE ( 'NONE', *, *, #7267, .T. ) ;
#31719 = DIRECTION ( 'NONE',  ( 1.734723475976806848E-16, -0.000000000000000000, 1.000000000000000000 ) ) ;
#31720 = CARTESIAN_POINT ( 'NONE',  ( 2.168245791271197209, 1.654581109258766558, -2.004968704497248400 ) ) ;
#31721 = LINE ( 'NONE', #44088, #9091 ) ;
#31722 = EDGE_LOOP ( 'NONE', ( #47547, #42650, #20728, #30764, #21887, #27372, #17546, #44040 ) ) ;
#31723 = ORIENTED_EDGE ( 'NONE', *, *, #20331, .T. ) ;
#31724 = CARTESIAN_POINT ( 'NONE',  ( -0.5455278134075208785, 3.267716535433071279, 0.7480314960629874665 ) ) ;
#31725 = DIRECTION ( 'NONE',  ( -3.469446951953613696E-16, 0.000000000000000000, -1.000000000000000000 ) ) ;
#31726 = AXIS2_PLACEMENT_3D ( 'NONE', #42321, #45927, #30206 ) ;
#31727 = CARTESIAN_POINT ( 'NONE',  ( 0.002207914879453961969, 5.905511811023623991, 0.04916304461325442243 ) ) ;
#31728 = EDGE_CURVE ( 'NONE', #2530, #17636, #31175, .T. ) ;
#31729 = VECTOR ( 'NONE', #24031, 39.37007874015748143 ) ;
#31730 = CARTESIAN_POINT ( 'NONE',  ( 0.2727639067037604947, 0.000000000000000000, -1.417322834645664331 ) ) ;
#31731 = VECTOR ( 'NONE', #10159, 39.37007874015748143 ) ;
#31732 = EDGE_CURVE ( 'NONE', #26914, #38732, #46630, .T. ) ;
#31733 = DIRECTION ( 'NONE',  ( 0.2660368455666688448, 0.000000000000000000, 0.9639628606958550172 ) ) ;
#31734 = DIRECTION ( 'NONE',  ( -3.469446951953613696E-16, 0.000000000000000000, -1.000000000000000000 ) ) ;
#31735 = ORIENTED_EDGE ( 'NONE', *, *, #19596, .T. ) ;
#31736 = CARTESIAN_POINT ( 'NONE',  ( -0.2727639067037605503, 3.267716535433071279, 4.731699523581609125E-17 ) ) ;
#31737 = B_SPLINE_CURVE_WITH_KNOTS ( 'NONE', 3,
 ( #46263, #7054, #19163, #14548 ),
 .UNSPECIFIED., .F., .F.,
 ( 4, 4 ),
 ( 2.220059671770691363E-07, 0.002500468339801800461 ),
 .UNSPECIFIED. ) ;
#31738 = VECTOR ( 'NONE', #46634, 39.37007874015748143 ) ;
#31739 = ORIENTED_EDGE ( 'NONE', *, *, #31508, .T. ) ;
#31740 = LINE ( 'NONE', #47437, #11899 ) ;
#31741 = EDGE_LOOP ( 'NONE', ( #14391, #22528, #32066, #26320 ) ) ;
#31742 = EDGE_CURVE ( 'NONE', #44911, #18980, #23670, .T. ) ;
#31743 = DIRECTION ( 'NONE',  ( -0.9998717552508121775, -0.01601477604151182316, 0.000000000000000000 ) ) ;
#31744 = DIRECTION ( 'NONE',  ( -0.000000000000000000, 1.000000000000000000, -0.000000000000000000 ) ) ;
#31745 = CARTESIAN_POINT ( 'NONE',  ( 1.735586374879370952, 0.000000000000000000, -2.388829707800026458 ) ) ;
#31746 = EDGE_LOOP ( 'NONE', ( #37980, #9531, #8142, #17429 ) ) ;
#31747 = ADVANCED_FACE ( 'NONE', ( #39168 ), #6966, .T. ) ;
#31748 = ADVANCED_FACE ( 'NONE', ( #35302 ), #50983, .F. ) ;
#31749 = FACE_OUTER_BOUND ( 'NONE', #38615, .T. ) ;
#31750 = EDGE_CURVE ( 'NONE', #26744, #26405, #24710, .T. ) ;
#31751 = ORIENTED_EDGE ( 'NONE', *, *, #17818, .T. ) ;
#31752 = DIRECTION ( 'NONE',  ( 0.000000000000000000, 0.000000000000000000, 1.000000000000000000 ) ) ;
#31753 = ORIENTED_EDGE ( 'NONE', *, *, #19497, .T. ) ;
#31754 = LINE ( 'NONE', #31248, #44978 ) ;
#31755 = LINE ( 'NONE', #40008, #9927 ) ;
#31756 = ORIENTED_EDGE ( 'NONE', *, *, #29273, .F. ) ;
#31757 = CARTESIAN_POINT ( 'NONE',  ( 0.08139965876239094178, 1.610780518492231694, 0.000000000000000000 ) ) ;
#31758 = CONICAL_SURFACE ( 'NONE', #31726, 3.483074324928249421, 1.244861948955335196 ) ;
#31759 = ORIENTED_EDGE ( 'NONE', *, *, #1440, .F. ) ;
#31760 = ORIENTED_EDGE ( 'NONE', *, *, #7664, .T. ) ;
#31761 = AXIS2_PLACEMENT_3D ( 'NONE', #6499, #50066, #3626 ) ;
#31762 = AXIS2_PLACEMENT_3D ( 'NONE', #16753, #43331, #8742 ) ;
#31763 = DIRECTION ( 'NONE',  ( 0.000000000000000000, -1.000000000000000000, 0.000000000000000000 ) ) ;
#31764 = CARTESIAN_POINT ( 'NONE',  ( -0.5455278134075214336, 0.000000000000000000, -0.1968503937007883287 ) ) ;
#31765 = CARTESIAN_POINT ( 'NONE',  ( 0.1450362469327832748, 6.692913385826772199, -2.160491579385212191 ) ) ;
#31766 = VECTOR ( 'NONE', #49299, 39.37007874015748143 ) ;
#31767 = VERTEX_POINT ( 'NONE', #16709 ) ;
#31768 = FACE_OUTER_BOUND ( 'NONE', #14344, .T. ) ;
#31769 = FACE_OUTER_BOUND ( 'NONE', #3216, .T. ) ;
#31770 = ADVANCED_FACE ( 'NONE', ( #4830 ), #1714, .F. ) ;
#31771 = ORIENTED_EDGE ( 'NONE', *, *, #47549, .T. ) ;
#31772 = CARTESIAN_POINT ( 'NONE',  ( -2.607957063749950066, 1.580174266876329670, 1.384773081374161663 ) ) ;
#31773 = VECTOR ( 'NONE', #42725, 39.37007874015748143 ) ;
#31774 = VERTEX_POINT ( 'NONE', #32463 ) ;
#31775 = VERTEX_POINT ( 'NONE', #48155 ) ;
#31776 = SHAPE_DEFINITION_REPRESENTATION ( #20731, #50787 ) ;
#31777 = EDGE_CURVE ( 'NONE', #12815, #28950, #949, .T. ) ;
#31778 = ORIENTED_EDGE ( 'NONE', *, *, #13202, .T. ) ;
#31779 = CARTESIAN_POINT ( 'NONE',  ( 0.3381173457103284763, 6.692913385826772199, 2.138793126519850318 ) ) ;
#31780 = FACE_OUTER_BOUND ( 'NONE', #5103, .T. ) ;
#31781 = ADVANCED_FACE ( 'NONE', ( #48402 ), #40461, .F. ) ;
#31782 = EDGE_CURVE ( 'NONE', #49534, #216, #21342, .T. ) ;
#31783 = DIRECTION ( 'NONE',  ( 0.000000000000000000, 0.000000000000000000, -1.000000000000000000 ) ) ;
#31784 = DIRECTION ( 'NONE',  ( -0.000000000000000000, 1.000000000000000000, -0.000000000000000000 ) ) ;
#31785 = ORIENTED_EDGE ( 'NONE', *, *, #9125, .F. ) ;
#31786 = ORIENTED_EDGE ( 'NONE', *, *, #49279, .F. ) ;
#31787 = CARTESIAN_POINT ( 'NONE',  ( 1.688048600224988149, 0.000000000000000000, -0.4357642695449466252 ) ) ;
#31788 = LINE ( 'NONE', #23020, #4533 ) ;
#31789 = EDGE_LOOP ( 'NONE', ( #45860, #22435, #34857, #41679 ) ) ;
#31790 = DIRECTION ( 'NONE',  ( 1.000000000000000000, 0.000000000000000000, 0.000000000000000000 ) ) ;
#31791 = DIRECTION ( 'NONE',  ( -9.701723960855733411E-17, 1.000000000000000000, -8.476140964546406840E-17 ) ) ;
#31792 = ADVANCED_FACE ( 'NONE', ( #9208 ), #20965, .T. ) ;
#31794 = B_SPLINE_CURVE_WITH_KNOTS ( 'NONE', 3,
 ( #13510, #13003, #8867, #48067 ),
 .UNSPECIFIED., .F., .F.,
 ( 4, 4 ),
 ( 2.018271350767252085E-07, 0.002500207285796618092 ),
 .UNSPECIFIED. ) ;
#31793 = LINE ( 'NONE', #43899, #14300 ) ;
#31795 = DIRECTION ( 'NONE',  ( -0.000000000000000000, 1.000000000000000000, -0.000000000000000000 ) ) ;
#31796 = VERTEX_POINT ( 'NONE', #44814 ) ;
#31797 = LINE ( 'NONE', #4169, #20939 ) ;
#31798 = LINE ( 'NONE', #4938, #34317 ) ;
#31799 = VECTOR ( 'NONE', #9460, 39.37007874015748143 ) ;
#31800 = VERTEX_POINT ( 'NONE', #5333 ) ;
#31801 = VECTOR ( 'NONE', #14362, 39.37007874015748143 ) ;
#31803 = EDGE_LOOP ( 'NONE', ( #27634, #7456, #2942, #42029 ) ) ;
#31802 = ADVANCED_FACE ( 'NONE', ( #20575 ), #28566, .F. ) ;
#31804 = CARTESIAN_POINT ( 'NONE',  ( 0.000000000000000000, 1.574803149606302854, 0.000000000000000000 ) ) ;
#31805 = FACE_OUTER_BOUND ( 'NONE', #37117, .T. ) ;
#31806 = FACE_OUTER_BOUND ( 'NONE', #2493, .T. ) ;
#31807 = CIRCLE ( 'NONE', #33490, 1.743387098533651480 ) ;
#31808 = ORIENTED_EDGE ( 'NONE', *, *, #24627, .F. ) ;
#31809 = ADVANCED_FACE ( 'NONE', ( #13340 ), #32980, .F. ) ;
#31810 = EDGE_CURVE ( 'NONE', #17939, #33261, #16016, .T. ) ;
#31811 = AXIS2_PLACEMENT_3D ( 'NONE', #46757, #46264, #42905 ) ;
#31812 = EDGE_CURVE ( 'NONE', #33606, #37376, #48656, .T. ) ;
#31813 = ORIENTED_EDGE ( 'NONE', *, *, #5243, .T. ) ;
#31814 = DIRECTION ( 'NONE',  ( 1.000000000000000000, 0.000000000000000000, -3.469446951953613696E-16 ) ) ;
#31815 = B_SPLINE_CURVE_WITH_KNOTS ( 'NONE', 3,
 ( #36465, #32863, #16072, #36210 ),
 .UNSPECIFIED., .F., .F.,
 ( 4, 4 ),
 ( 6.088918481998526345E-07, 0.0008127897595450017231 ),
 .UNSPECIFIED. ) ;
#31816 = ORIENTED_EDGE ( 'NONE', *, *, #30175, .F. ) ;
#31817 = DIRECTION ( 'NONE',  ( 0.000000000000000000, 0.000000000000000000, 1.000000000000000000 ) ) ;
#31818 = ORIENTED_EDGE ( 'NONE', *, *, #23046, .F. ) ;
#31819 = DIRECTION ( 'NONE',  ( -1.000000000000000000, 0.000000000000000000, -0.000000000000000000 ) ) ;
#31820 = LINE ( 'NONE', #32332, #4129 ) ;
#31821 = PLANE ( 'NONE',  #27659 ) ;
#31822 = ORIENTED_EDGE ( 'NONE', *, *, #49246, .F. ) ;
#31823 = ORIENTED_EDGE ( 'NONE', *, *, #22853, .T. ) ;
#31824 = ORIENTED_EDGE ( 'NONE', *, *, #28262, .F. ) ;
#31825 = PLANE ( 'NONE',  #43832 ) ;
#31826 = CARTESIAN_POINT ( 'NONE',  ( 0.000000000000000000, 7.874015748031496287, 0.000000000000000000 ) ) ;
#31827 = ORIENTED_EDGE ( 'NONE', *, *, #1766, .T. ) ;
#31828 = VERTEX_POINT ( 'NONE', #36584 ) ;
#31829 = CARTESIAN_POINT ( 'NONE',  ( -1.295944566667802889, 1.542179613706447849, -2.653217792976843015 ) ) ;
#31830 = DIRECTION ( 'NONE',  ( 0.000000000000000000, 0.000000000000000000, 1.000000000000000000 ) ) ;
#31831 = DIRECTION ( 'NONE',  ( 1.734723475976806848E-16, 0.000000000000000000, 1.000000000000000000 ) ) ;
#31832 = ORIENTED_EDGE ( 'NONE', *, *, #27616, .F. ) ;
#31833 = ORIENTED_EDGE ( 'NONE', *, *, #27994, .F. ) ;
#31834 = DIRECTION ( 'NONE',  ( 0.000000000000000000, 0.000000000000000000, -1.000000000000000000 ) ) ;
#31835 = CARTESIAN_POINT ( 'NONE',  ( -1.091055626815042645, 3.346456692913386100, -1.456692913385822186 ) ) ;
#31836 = CARTESIAN_POINT ( 'NONE',  ( -1.236813753895213086, 1.699986652445209634, -2.681693691597581974 ) ) ;
#31837 = VECTOR ( 'NONE', #39597, 39.37007874015748143 ) ;
#31838 = VERTEX_POINT ( 'NONE', #29074 ) ;
#31839 = CARTESIAN_POINT ( 'NONE',  ( 0.000000000000000000, 6.692913385826772199, 0.000000000000000000 ) ) ;
#31840 = LINE ( 'NONE', #23313, #4643 ) ;
#31841 = VECTOR ( 'NONE', #12817, 39.37007874015748854 ) ;
#31842 = ORIENTED_EDGE ( 'NONE', *, *, #9479, .F. ) ;
#31843 = VECTOR ( 'NONE', #42247, 39.37007874015748143 ) ;
#31844 = DIRECTION ( 'NONE',  ( -0.000000000000000000, 1.000000000000000000, -0.000000000000000000 ) ) ;
#31845 = ORIENTED_EDGE ( 'NONE', *, *, #41324, .T. ) ;
#31846 = ORIENTED_EDGE ( 'NONE', *, *, #42791, .T. ) ;
#31847 = DIRECTION ( 'NONE',  ( 0.000000000000000000, -1.000000000000000000, 0.000000000000000000 ) ) ;
#31848 = PLANE ( 'NONE',  #21822 ) ;
#31849 = AXIS2_PLACEMENT_3D ( 'NONE', #48796, #13477, #28956 ) ;
#31850 = CARTESIAN_POINT ( 'NONE',  ( 0.1067246931122726866, 0.02962905676920215767, 0.000000000000000000 ) ) ;
#31851 = ADVANCED_FACE ( 'NONE', ( #9465 ), #354, .T. ) ;
#31852 = VECTOR ( 'NONE', #35964, 39.37007874015748143 ) ;
#31853 = PLANE ( 'NONE',  #17074 ) ;
#31854 = CARTESIAN_POINT ( 'NONE',  ( 0.5455278134075208785, 3.346456692913386100, -2.086614173228340086 ) ) ;
#31855 = EDGE_LOOP ( 'NONE', ( #33882, #32472, #27921, #45010, #48397, #215 ) ) ;
#31857 = EDGE_CURVE ( 'NONE', #39762, #38725, #32753, .T. ) ;
#31856 = ORIENTED_EDGE ( 'NONE', *, *, #8465, .F. ) ;
#31858 = VECTOR ( 'NONE', #19993, 39.37007874015748143 ) ;
#31859 = ORIENTED_EDGE ( 'NONE', *, *, #15139, .F. ) ;
#31860 = FACE_OUTER_BOUND ( 'NONE', #27563, .T. ) ;
#31861 = CARTESIAN_POINT ( 'NONE',  ( -1.439733046521776361, 0.000000000000000000, 0.7480314960629874665 ) ) ;
#31862 = B_SPLINE_CURVE_WITH_KNOTS ( 'NONE', 3,
 ( #50684, #19496, #42235, #18997 ),
 .UNSPECIFIED., .F., .F.,
 ( 4, 4 ),
 ( 2.175066794692088623E-07, 0.002500264396982808911 ),
 .UNSPECIFIED. ) ;
#31863 = DIRECTION ( 'NONE',  ( -0.9989930665413144784, 0.000000000000000000, -0.04486483035051863633 ) ) ;
#31864 = DIRECTION ( 'NONE',  ( -3.469446951953613696E-16, 0.000000000000000000, -1.000000000000000000 ) ) ;
#31865 = VERTEX_POINT ( 'NONE', #12570 ) ;
#31866 = LINE ( 'NONE', #19715, #33303 ) ;
#31867 = EDGE_CURVE ( 'NONE', #18498, #49569, #40970, .T. ) ;
#31868 = CARTESIAN_POINT ( 'NONE',  ( 1.785842763811721357, 0.03714046191358289645, 0.9051173831972618711 ) ) ;
#31869 = VERTEX_POINT ( 'NONE', #44051 ) ;
#31870 = CARTESIAN_POINT ( 'NONE',  ( -1.915752150681443222, 1.685393533398291233, -1.899733137568783814 ) ) ;
#31871 = EDGE_CURVE ( 'NONE', #2736, #14380, #8445, .T. ) ;
#31872 = LINE ( 'NONE', #43715, #45918 ) ;
#31873 = CARTESIAN_POINT ( 'NONE',  ( 0.2727639067037604392, 3.346456692913386100, -1.614173228346451605 ) ) ;
#31874 = ORIENTED_EDGE ( 'NONE', *, *, #32751, .T. ) ;
#31875 = AXIS2_PLACEMENT_3D ( 'NONE', #45609, #22156, #18272 ) ;
#31876 = FACE_OUTER_BOUND ( 'NONE', #20462, .T. ) ;
#31877 = CARTESIAN_POINT ( 'NONE',  ( 0.002207914879453961969, 6.692913385826772199, 0.04916304461325451958 ) ) ;
#31878 = EDGE_CURVE ( 'NONE', #2160, #12958, #49924, .T. ) ;
#31879 = DIRECTION ( 'NONE',  ( 1.734723475976806848E-16, 0.000000000000000000, 1.000000000000000000 ) ) ;
#31880 = AXIS2_PLACEMENT_3D ( 'NONE', #29711, #36956, #1577 ) ;
#31881 = AXIS2_PLACEMENT_3D ( 'NONE', #87, #23844, #43193 ) ;
#31882 = EDGE_CURVE ( 'NONE', #22897, #37873, #26227, .T. ) ;
#31883 = ORIENTED_EDGE ( 'NONE', *, *, #35558, .T. ) ;
#31884 = FACE_BOUND ( 'NONE', #41550, .T. ) ;
#31885 = CARTESIAN_POINT ( 'NONE',  ( 2.192594616722325807, 1.677403568648509813, 0.7641623650280537916 ) ) ;
#31886 = ORIENTED_EDGE ( 'NONE', *, *, #6096, .F. ) ;
#31887 = EDGE_CURVE ( 'NONE', #8556, #10297, #13850, .T. ) ;
#31888 = CARTESIAN_POINT ( 'NONE',  ( -1.181102362204724310, 0.000000000000000000, -1.062992125984252079 ) ) ;
#31889 = DIRECTION ( 'NONE',  ( 1.000000000000000000, 0.000000000000000000, -3.469446951953613696E-16 ) ) ;
#31890 = DIRECTION ( 'NONE',  ( -3.469446951953613696E-16, 0.000000000000000000, -1.000000000000000000 ) ) ;
#31891 = CARTESIAN_POINT ( 'NONE',  ( -0.07591351300297333182, 0.000000000000000000, -1.417322834645664331 ) ) ;
#31892 = AXIS2_PLACEMENT_3D ( 'NONE', #42034, #17780, #46381 ) ;
#31893 = AXIS2_PLACEMENT_3D ( 'NONE', #32344, #9090, #27938 ) ;
#31894 = ORIENTED_EDGE ( 'NONE', *, *, #24549, .T. ) ;
#31895 = ORIENTED_EDGE ( 'NONE', *, *, #42839, .T. ) ;
#31896 = CARTESIAN_POINT ( 'NONE',  ( 1.443330927545150910, 3.267716535433071279, -1.614173228346452715 ) ) ;
#31897 = CARTESIAN_POINT ( 'NONE',  ( -1.636583440222564301, 0.000000000000000000, -1.141732283464563791 ) ) ;
#31898 = VERTEX_POINT ( 'NONE', #6615 ) ;
#31899 = DIRECTION ( 'NONE',  ( 1.734723475976806848E-16, -0.000000000000000000, 1.000000000000000000 ) ) ;
#31900 = DIRECTION ( 'NONE',  ( 1.734723475976806848E-16, -0.000000000000000000, 1.000000000000000000 ) ) ;
#31901 = DIRECTION ( 'NONE',  ( -0.000000000000000000, 1.000000000000000000, -0.000000000000000000 ) ) ;
#31902 = CARTESIAN_POINT ( 'NONE',  ( 1.560669927219590747, 3.267716535433071279, -5.414661521997677271E-16 ) ) ;
#31903 = VERTEX_POINT ( 'NONE', #17972 ) ;
#31904 = ORIENTED_EDGE ( 'NONE', *, *, #3295, .F. ) ;
#31905 = CARTESIAN_POINT ( 'NONE',  ( -0.5455278134075214336, 3.346456692913386100, -0.6299212598425175669 ) ) ;
#31906 = CARTESIAN_POINT ( 'NONE',  ( 0.000000000000000000, 3.267716535433071279, -0.7874015748031473194 ) ) ;
#31907 = CARTESIAN_POINT ( 'NONE',  ( -0.8329809839909436686, 1.533199950842965453, -2.833254665166566877 ) ) ;
#31908 = CARTESIAN_POINT ( 'NONE',  ( 1.015142113812069979, 3.346456692913386100, 1.732283464566921172 ) ) ;
#31909 = FACE_BOUND ( 'NONE', #26539, .T. ) ;
#31910 = VERTEX_POINT ( 'NONE', #33740 ) ;
#31911 = CARTESIAN_POINT ( 'NONE',  ( 0.1155636338427008941, -0.5222242541845523167, 0.000000000000000000 ) ) ;
#31912 = ORIENTED_EDGE ( 'NONE', *, *, #12254, .T. ) ;
#31913 = ORIENTED_EDGE ( 'NONE', *, *, #14312, .T. ) ;
#31914 = PLANE ( 'NONE',  #35779 ) ;
#31915 = AXIS2_PLACEMENT_3D ( 'NONE', #30785, #2914, #3161 ) ;
#31916 = EDGE_LOOP ( 'NONE', ( #44948, #25428, #30026, #33917 ) ) ;
#31917 = ORIENTED_EDGE ( 'NONE', *, *, #29700, .T. ) ;
#31918 = CARTESIAN_POINT ( 'NONE',  ( -0.04921259842519708216, 1.620047916482694861, 2.952755905511811108 ) ) ;
#31919 = ORIENTED_EDGE ( 'NONE', *, *, #17562, .F. ) ;
#31920 = EDGE_CURVE ( 'NONE', #18819, #27935, #22107, .T. ) ;
#31921 = CONICAL_SURFACE ( 'NONE', #42587, 1.850107469027523210, 0.6386652850508578450 ) ;
#31922 = EDGE_CURVE ( 'NONE', #46790, #5893, #45820, .T. ) ;
#31923 = DIRECTION ( 'NONE',  ( -1.000000000000000000, 0.000000000000000000, 1.734723475976806848E-16 ) ) ;
#31924 = PLANE ( 'NONE',  #5448 ) ;
#31925 = ADVANCED_FACE ( 'NONE', ( #17721 ), #25094, .T. ) ;
#31926 = DIRECTION ( 'NONE',  ( 0.04486483035051863633, 0.000000000000000000, -0.9989930665413144784 ) ) ;
#31927 = VECTOR ( 'NONE', #42124, 39.37007874015748143 ) ;
#31928 = FACE_OUTER_BOUND ( 'NONE', #39320, .T. ) ;
#31929 = CARTESIAN_POINT ( 'NONE',  ( 0.1968503937007878568, 0.000000000000000000, 1.574803149606291974 ) ) ;
#31930 = LINE ( 'NONE', #20809, #45130 ) ;
#31931 = EDGE_LOOP ( 'NONE', ( #34049, #36935, #12386, #23182 ) ) ;
#31932 = DIRECTION ( 'NONE',  ( 0.000000000000000000, 1.000000000000000000, 0.000000000000000000 ) ) ;
#31933 = CARTESIAN_POINT ( 'NONE',  ( 1.775400203342704986, 1.746929418358725172, -2.359903268218703332 ) ) ;
#31934 = CARTESIAN_POINT ( 'NONE',  ( -0.8942052331142552601, 0.000000000000000000, -1.889763779527552146 ) ) ;
#31935 = ORIENTED_EDGE ( 'NONE', *, *, #4337, .T. ) ;
#31936 = DIRECTION ( 'NONE',  ( -0.000000000000000000, 1.000000000000000000, -0.000000000000000000 ) ) ;
#31937 = EDGE_CURVE ( 'NONE', #44082, #48833, #49424, .T. ) ;
#31938 = CARTESIAN_POINT ( 'NONE',  ( -1.734129965298919718, 4.960977165729326543E-05, 0.1852418127046455421 ) ) ;
#31939 = ORIENTED_EDGE ( 'NONE', *, *, #29128, .F. ) ;
#31940 = CARTESIAN_POINT ( 'NONE',  ( 1.091055626815043311, 0.000000000000000000, 1.889763779527550369 ) ) ;
#31941 = PLANE ( 'NONE',  #6971 ) ;
#31942 = CARTESIAN_POINT ( 'NONE',  ( 1.909347346926324684, 3.267716535433071279, -0.03937007874015936021 ) ) ;
#31943 = EDGE_CURVE ( 'NONE', #39739, #45623, #1973, .T. ) ;
#31944 = LINE ( 'NONE', #32459, #43026 ) ;
#31945 = ORIENTED_EDGE ( 'NONE', *, *, #41580, .F. ) ;
#31946 = DIRECTION ( 'NONE',  ( -0.6427876096865403621, 0.7660444431189770143, -7.432978702377923406E-17 ) ) ;
#31947 = CARTESIAN_POINT ( 'NONE',  ( 1.628466770324754176, 1.733984826446373750, -1.625060189682509870 ) ) ;
#31948 = LINE ( 'NONE', #36586, #35015 ) ;
#31949 = CARTESIAN_POINT ( 'NONE',  ( 1.544727076124027931, 0.5249316475426858419, -1.078632795641746966 ) ) ;
#31950 = VECTOR ( 'NONE', #17361, 39.37007874015748143 ) ;
#31951 = VECTOR ( 'NONE', #31296, 39.37007874015748143 ) ;
#31952 = CONICAL_SURFACE ( 'NONE', #42653, 3.483074324928249421, 1.244861948955335196 ) ;
#31953 = VERTEX_POINT ( 'NONE', #25974 ) ;
#31954 = ORIENTED_EDGE ( 'NONE', *, *, #36738, .T. ) ;
#31955 = CARTESIAN_POINT ( 'NONE',  ( -0.2727639067037611609, 3.267716535433071279, 4.731699523581620218E-17 ) ) ;
#31956 = EDGE_LOOP ( 'NONE', ( #9520, #7643, #12470, #8176 ) ) ;
#31957 = CARTESIAN_POINT ( 'NONE',  ( -0.5756566573089004768, 1.527738838675063882, 2.896516654582634853 ) ) ;
#31958 = EDGE_CURVE ( 'NONE', #2318, #7103, #18227, .T. ) ;
#31959 = ORIENTED_EDGE ( 'NONE', *, *, #18872, .F. ) ;
#31960 = DIRECTION ( 'NONE',  ( 1.000000000000000000, 0.000000000000000000, 1.734839586111147642E-16 ) ) ;
#31961 = ORIENTED_EDGE ( 'NONE', *, *, #4999, .F. ) ;
#31962 = DIRECTION ( 'NONE',  ( 0.000000000000000000, -1.000000000000000000, 0.000000000000000000 ) ) ;
#31963 = LINE ( 'NONE', #24209, #32248 ) ;
#31964 = VERTEX_POINT ( 'NONE', #6361 ) ;
#31965 = DIRECTION ( 'NONE',  ( 0.000000000000000000, 0.000000000000000000, -1.000000000000000000 ) ) ;
#31966 = ORIENTED_EDGE ( 'NONE', *, *, #31398, .T. ) ;
#31967 = AXIS2_PLACEMENT_3D ( 'NONE', #5062, #32962, #17704 ) ;
#31968 = DIRECTION ( 'NONE',  ( 0.000000000000000000, 0.000000000000000000, 1.000000000000000000 ) ) ;
#31969 = VERTEX_POINT ( 'NONE', #29597 ) ;
#31970 = ORIENTED_EDGE ( 'NONE', *, *, #50176, .T. ) ;
#31971 = DIRECTION ( 'NONE',  ( -1.000000000000000000, 0.000000000000000000, 0.000000000000000000 ) ) ;
#31972 = B_SPLINE_CURVE_WITH_KNOTS ( 'NONE', 3,
 ( #3339, #14203, #25823, #21960 ),
 .UNSPECIFIED., .F., .F.,
 ( 4, 4 ),
 ( 0.02763470841684000437, 0.02815926868579550144 ),
 .UNSPECIFIED. ) ;
#31973 = ADVANCED_FACE ( 'NONE', ( #13598 ), #48966, .F. ) ;
#31974 = CARTESIAN_POINT ( 'NONE',  ( 0.4696143004045476577, 0.000000000000000000, -1.732283464566922726 ) ) ;
#31975 = ORIENTED_EDGE ( 'NONE', *, *, #12544, .F. ) ;
#31976 = LINE ( 'NONE', #40742, #15547 ) ;
#31977 = ORIENTED_EDGE ( 'NONE', *, *, #13124, .T. ) ;
#31978 = CARTESIAN_POINT ( 'NONE',  ( 2.623503965249849301, 1.661669217907264740, 1.355882097269874187 ) ) ;
#31979 = ADVANCED_FACE ( 'NONE', ( #41469 ), #11091, .T. ) ;
#31980 = DIRECTION ( 'NONE',  ( -1.000000000000000000, 0.000000000000000000, 0.000000000000000000 ) ) ;
#31981 = ADVANCED_FACE ( 'NONE', ( #25717 ), #6097, .F. ) ;
#31982 = VECTOR ( 'NONE', #4181, 39.37007874015748143 ) ;
#31983 = VECTOR ( 'NONE', #4884, 39.37007874015748143 ) ;
#31984 = EDGE_CURVE ( 'NONE', #44346, #29618, #30102, .T. ) ;
#31985 = CARTESIAN_POINT ( 'NONE',  ( 0.4696143004045478797, 0.000000000000000000, -0.6692913385826760875 ) ) ;
#31986 = VERTEX_POINT ( 'NONE', #49670 ) ;
#31987 = ORIENTED_EDGE ( 'NONE', *, *, #32469, .F. ) ;
#31988 = DIRECTION ( 'NONE',  ( -1.000000000000000000, -0.000000000000000000, -0.000000000000000000 ) ) ;
#31989 = CYLINDRICAL_SURFACE ( 'NONE', #8969, 2.165354330708661568 ) ;
#31990 = LINE ( 'NONE', #4870, #18394 ) ;
#31991 = VECTOR ( 'NONE', #3631, 39.37007874015748143 ) ;
#31992 = CARTESIAN_POINT ( 'NONE',  ( 1.087963734054938625, 1.205361022782829114E-17, 1.724994741719410918 ) ) ;
#31993 = CARTESIAN_POINT ( 'NONE',  ( -0.8942052331142547050, 3.267716535433071279, 3.102397620449221495E-16 ) ) ;
#31994 = DIRECTION ( 'NONE',  ( -0.000000000000000000, -1.000000000000000000, -0.000000000000000000 ) ) ;
#31995 = ADVANCED_FACE ( 'NONE', ( #18484 ), #9723, .T. ) ;
#31996 = ORIENTED_EDGE ( 'NONE', *, *, #45682, .F. ) ;
#31997 = CARTESIAN_POINT ( 'NONE',  ( 0.1968503937007877735, 3.346456692913386100, 1.692913385826762873 ) ) ;
#31998 = VERTEX_POINT ( 'NONE', #44974 ) ;
#31999 = DIRECTION ( 'NONE',  ( -1.000000000000000000, 0.000000000000000000, 0.000000000000000000 ) ) ;
#32000 = EDGE_CURVE ( 'NONE', #49676, #26927, #48819, .T. ) ;
#32001 = VECTOR ( 'NONE', #46737, 39.37007874015748143 ) ;
#32002 = ORIENTED_EDGE ( 'NONE', *, *, #27754, .T. ) ;
#32003 = CARTESIAN_POINT ( 'NONE',  ( 0.4696143004045476577, 3.346456692913386100, -1.732283464566922726 ) ) ;
#32004 = CARTESIAN_POINT ( 'NONE',  ( -1.312248418042854858, 1.574803149606302854, -1.722429524498108711 ) ) ;
#32005 = LINE ( 'NONE', #47697, #49780 ) ;
#32006 = VERTEX_POINT ( 'NONE', #40369 ) ;
#32007 = EDGE_CURVE ( 'NONE', #12716, #41514, #40617, .T. ) ;
#32008 = DIRECTION ( 'NONE',  ( -3.469446951953613696E-16, 0.000000000000000000, -1.000000000000000000 ) ) ;
#32009 = CARTESIAN_POINT ( 'NONE',  ( 0.08139965876239094178, 1.610780518492231694, 0.000000000000000000 ) ) ;
#32010 = VERTEX_POINT ( 'NONE', #5239 ) ;
#32011 = CARTESIAN_POINT ( 'NONE',  ( -0.9146000759343694275, 1.693252956796532871, -2.012610095043610769 ) ) ;
#32012 = ADVANCED_FACE ( 'NONE', ( #29241 ), #6120, .F. ) ;
#32013 = ORIENTED_EDGE ( 'NONE', *, *, #35600, .T. ) ;
#32014 = PLANE ( 'NONE',  #41724 ) ;
#32015 = CARTESIAN_POINT ( 'NONE',  ( 2.217727732172433353, 0.5219239147199549178, -0.5566600749325844033 ) ) ;
#32016 =( BOUNDED_CURVE ( )  B_SPLINE_CURVE ( 3, ( #38862, #7869, #26727, #42474 ),
 .UNSPECIFIED., .F., .F. ) 
 B_SPLINE_CURVE_WITH_KNOTS ( ( 4, 4 ),
 ( 2.384712079142225161, 2.847747046894732126 ),
 .UNSPECIFIED. ) 
 CURVE ( )  GEOMETRIC_REPRESENTATION_ITEM ( )  RATIONAL_B_SPLINE_CURVE ( ( 1.000000000000000000, 0.9822128812423629451, 0.9822128812423629451, 1.000000000000000000 ) ) 
 REPRESENTATION_ITEM ( '' )  );
#32017 = VECTOR ( 'NONE', #39432, 39.37007874015748143 ) ;
#32018 = CARTESIAN_POINT ( 'NONE',  ( -0.5455278134075208785, 3.267716535433071279, 1.259842519685033357 ) ) ;
#32019 = VERTEX_POINT ( 'NONE', #44716 ) ;
#32020 = ORIENTED_EDGE ( 'NONE', *, *, #14852, .T. ) ;
#32021 = EDGE_CURVE ( 'NONE', #36731, #15952, #9631, .T. ) ;
#32022 = CARTESIAN_POINT ( 'NONE',  ( -2.168245791271168343, 1.685466330048090322, -2.004968704497279930 ) ) ;
#32023 = LINE ( 'NONE', #19613, #38845 ) ;
#32024 = FACE_BOUND ( 'NONE', #8904, .T. ) ;
#32025 = VECTOR ( 'NONE', #43304, 39.37007874015748143 ) ;
#32026 = ADVANCED_FACE ( 'NONE', ( #28469 ), #41128, .F. ) ;
#32027 = AXIS2_PLACEMENT_3D ( 'NONE', #30311, #22058, #33439 ) ;
#32028 = AXIS2_PLACEMENT_3D ( 'NONE', #28427, #23288, #39038 ) ;
#32029 = DIRECTION ( 'NONE',  ( -1.000000000000000000, 0.000000000000000000, -0.000000000000000000 ) ) ;
#32030 = DIRECTION ( 'NONE',  ( -3.469446951953613696E-16, 0.000000000000000000, -1.000000000000000000 ) ) ;
#32031 = ORIENTED_EDGE ( 'NONE', *, *, #25551, .T. ) ;
#32032 = VECTOR ( 'NONE', #32432, 39.37007874015748143 ) ;
#32033 = CARTESIAN_POINT ( 'NONE',  ( 0.000000000000000000, 3.267716535433071279, 1.417322834645662777 ) ) ;
#32034 = ORIENTED_EDGE ( 'NONE', *, *, #26222, .F. ) ;
#32035 = ORIENTED_EDGE ( 'NONE', *, *, #21898, .T. ) ;
#32036 = SHAPE_DEFINITION_REPRESENTATION ( #7091, #5020 ) ;
#32037 = VECTOR ( 'NONE', #3285, 39.37007874015748143 ) ;
#32038 = EDGE_LOOP ( 'NONE', ( #26352, #29145, #41811, #14227 ) ) ;
#32039 = CARTESIAN_POINT ( 'NONE',  ( 0.1968503937007874405, 3.346456692913386100, 0.000000000000000000 ) ) ;
#32040 = EDGE_CURVE ( 'NONE', #49693, #30403, #24611, .T. ) ;
#32041 = DIRECTION ( 'NONE',  ( -0.8268442224656336048, -0.000000000000000000, -0.5624310017906212211 ) ) ;
#32042 = CARTESIAN_POINT ( 'NONE',  ( -2.182111253630085290, 3.346456692913386100, -0.5118110236220464460 ) ) ;
#32043 = EDGE_CURVE ( 'NONE', #22349, #12025, #9373, .T. ) ;
#32044 = DIRECTION ( 'NONE',  ( -0.000000000000000000, 1.000000000000000000, -0.000000000000000000 ) ) ;
#32045 = VERTEX_POINT ( 'NONE', #4987 ) ;
#32046 = ORIENTED_EDGE ( 'NONE', *, *, #39861, .T. ) ;
#32047 = DIRECTION ( 'NONE',  ( -0.000000000000000000, -1.000000000000000000, -0.000000000000000000 ) ) ;
#32048 = DIRECTION ( 'NONE',  ( -0.000000000000000000, -1.000000000000000000, -0.000000000000000000 ) ) ;
#32049 = CARTESIAN_POINT ( 'NONE',  ( -0.7874015748031498729, 0.000000000000000000, -1.138269997360109921E-16 ) ) ;
#32050 = VERTEX_POINT ( 'NONE', #17375 ) ;
#32051 = CARTESIAN_POINT ( 'NONE',  ( 0.1067246931122726866, 0.02962905676920215767, 0.000000000000000000 ) ) ;
#32052 = LINE ( 'NONE', #44415, #19004 ) ;
#32053 = CARTESIAN_POINT ( 'NONE',  ( 0.000000000000000000, 1.574803149606302854, 0.000000000000000000 ) ) ;
#32054 = AXIS2_PLACEMENT_3D ( 'NONE', #43997, #36018, #642 ) ;
#32055 = CARTESIAN_POINT ( 'NONE',  ( 1.514466370292996578, 5.905511811023623991, 2.534789744887420149 ) ) ;
#32056 = DIRECTION ( 'NONE',  ( -3.469446951953613696E-16, 0.000000000000000000, -1.000000000000000000 ) ) ;
#32057 = ORIENTED_EDGE ( 'NONE', *, *, #45356, .T. ) ;
#32058 = DIRECTION ( 'NONE',  ( 1.734723475976806848E-16, 0.000000000000000000, 1.000000000000000000 ) ) ;
#32059 = DIRECTION ( 'NONE',  ( -0.000000000000000000, 1.000000000000000000, -0.000000000000000000 ) ) ;
#32060 = ORIENTED_EDGE ( 'NONE', *, *, #30508, .F. ) ;
#32061 = ORIENTED_EDGE ( 'NONE', *, *, #35762, .T. ) ;
#32063 = CARTESIAN_POINT ( 'NONE',  ( 1.287906020515830363, 3.267716535433071279, -4.468321617281356063E-16 ) ) ;
#32062 = CONICAL_SURFACE ( 'NONE', #30402, 3.033577403570480779, 1.554780866114618743 ) ;
#32064 = CARTESIAN_POINT ( 'NONE',  ( 2.164971648505046975, 5.905511811023623991, -0.04070796836118371897 ) ) ;
#32065 = DIRECTION ( 'NONE',  ( 0.000000000000000000, -1.000000000000000000, 0.000000000000000000 ) ) ;
#32066 = ORIENTED_EDGE ( 'NONE', *, *, #33444, .F. ) ;
#32067 = EDGE_CURVE ( 'NONE', #43799, #11883, #3835, .T. ) ;
#32068 = VECTOR ( 'NONE', #14517, 39.37007874015748143 ) ;
#32069 = EDGE_LOOP ( 'NONE', ( #28790, #24738, #27377, #11240 ) ) ;
#32070 = CARTESIAN_POINT ( 'NONE',  ( 2.755905511811024056, 4.960629921259846142, 1.023622047244094446 ) ) ;
#32071 = VERTEX_POINT ( 'NONE', #28979 ) ;
#32072 = VECTOR ( 'NONE', #15606, 39.37007874015748143 ) ;
#32073 = CARTESIAN_POINT ( 'NONE',  ( 1.769879628650530723, 0.05626752682809384870, -0.8100022834900426627 ) ) ;
#32074 = EDGE_CURVE ( 'NONE', #22430, #18703, #39095, .T. ) ;
#32075 = EDGE_LOOP ( 'NONE', ( #25555, #47035, #42654, #44409 ) ) ;
#32076 = CARTESIAN_POINT ( 'NONE',  ( 1.686111637834603938, 0.05492582915004715072, 0.9632209503012270080 ) ) ;
#32077 = LINE ( 'NONE', #31558, #48610 ) ;
#32078 = LINE ( 'NONE', #19916, #40879 ) ;
#32079 = EDGE_CURVE ( 'NONE', #27812, #29397, #16613, .T. ) ;
#32080 = ADVANCED_FACE ( 'NONE', ( #8604 ), #29502, .F. ) ;
#32081 = ORIENTED_EDGE ( 'NONE', *, *, #23439, .T. ) ;
#32082 = DIMENSIONAL_EXPONENTS ( 1.000000000000000000, 0.000000000000000000, 0.000000000000000000, 0.000000000000000000, 0.000000000000000000, 0.000000000000000000, 0.000000000000000000 ) ;
#32083 = ORIENTED_EDGE ( 'NONE', *, *, #3269, .F. ) ;
#32084 = ORIENTED_EDGE ( 'NONE', *, *, #27102, .F. ) ;
#32085 = DIRECTION ( 'NONE',  ( -0.01601477604151182663, 0.9998717552508123996, -0.000000000000000000 ) ) ;
#32086 = ORIENTED_EDGE ( 'NONE', *, *, #36243, .F. ) ;
#32087 = ORIENTED_EDGE ( 'NONE', *, *, #24167, .F. ) ;
#32088 = EDGE_CURVE ( 'NONE', #12444, #8496, #4735, .T. ) ;
#32089 = CARTESIAN_POINT ( 'NONE',  ( -0.3486774197067339376, 0.000000000000000000, -1.259842519685035134 ) ) ;
#32090 = DIRECTION ( 'NONE',  ( -0.000000000000000000, 1.000000000000000000, -0.000000000000000000 ) ) ;
#32091 = LINE ( 'NONE', #24590, #3025 ) ;
#32092 = EDGE_CURVE ( 'NONE', #31670, #48175, #34170, .T. ) ;
#32093 = ORIENTED_EDGE ( 'NONE', *, *, #46206, .F. ) ;
#32094 = LINE ( 'NONE', #20710, #35372 ) ;
#32095 = PLANE ( 'NONE',  #28286 ) ;
#32096 = VECTOR ( 'NONE', #37230, 39.37007874015748143 ) ;
#32097 = CARTESIAN_POINT ( 'NONE',  ( -1.439733046521776139, 3.346456692913386100, 0.9448818897637749625 ) ) ;
#32098 = VERTEX_POINT ( 'NONE', #8861 ) ;
#32099 = CARTESIAN_POINT ( 'NONE',  ( -0.2727639067037607723, 3.346456692913386100, -1.417322834645664331 ) ) ;
#32100 = ORIENTED_EDGE ( 'NONE', *, *, #46689, .F. ) ;
#32101 = CARTESIAN_POINT ( 'NONE',  ( -2.378234070510009790, 1.575584252498931193, -0.4923382150760590159 ) ) ;
#32102 = ORIENTED_EDGE ( 'NONE', *, *, #6917, .T. ) ;
#32103 = ORIENTED_EDGE ( 'NONE', *, *, #40056, .T. ) ;
#32104 = DIRECTION ( 'NONE',  ( -1.000000000000000000, -0.000000000000000000, -0.000000000000000000 ) ) ;
#32105 = CARTESIAN_POINT ( 'NONE',  ( -0.3937007874015748254, 3.248031496062991685, -2.362204724409448620 ) ) ;
#32106 = EDGE_CURVE ( 'NONE', #24532, #40028, #14898, .T. ) ;
#32107 = VECTOR ( 'NONE', #3714, 39.37007874015748143 ) ;
#32108 = CARTESIAN_POINT ( 'NONE',  ( -1.439733046521776583, 0.000000000000000000, -1.574803149606293307 ) ) ;
#32109 = CARTESIAN_POINT ( 'NONE',  ( -2.165460538733998241, 1.205361022782829114E-17, 0.04798874274652762534 ) ) ;
#32110 = EDGE_CURVE ( 'NONE', #23592, #21262, #1368, .T. ) ;
#32112 = AXIS2_PLACEMENT_3D ( 'NONE', #21082, #40704, #36839 ) ;
#32111 = LINE ( 'NONE', #16092, #12304 ) ;
#32113 = VERTEX_POINT ( 'NONE', #12997 ) ;
#32114 = EDGE_LOOP ( 'NONE', ( #39241, #48078, #1657, #39591 ) ) ;
#32115 = EDGE_CURVE ( 'NONE', #3395, #21117, #14255, .T. ) ;
#32116 = CIRCLE ( 'NONE', #27148, 2.165354330708661568 ) ;
#32117 = ORIENTED_EDGE ( 'NONE', *, *, #16564, .F. ) ;
#32118 = DIRECTION ( 'NONE',  ( 1.000000000000000000, 0.000000000000000000, -3.469446951953613696E-16 ) ) ;
#32119 = DIRECTION ( 'NONE',  ( -0.000000000000000000, -1.000000000000000000, -0.000000000000000000 ) ) ;
#32120 = CARTESIAN_POINT ( 'NONE',  ( 0.1968503937007869686, 3.346456692913386100, -2.086614173228339641 ) ) ;
#32121 = CARTESIAN_POINT ( 'NONE',  ( 2.923830774217214934, 1.764811239170032131, 0.4126137884981752602 ) ) ;
#32122 = CARTESIAN_POINT ( 'NONE',  ( 1.560669927219590303, 0.000000000000000000, -1.929133858267710666 ) ) ;
#32123 = ORIENTED_EDGE ( 'NONE', *, *, #16295, .F. ) ;
#32124 = CARTESIAN_POINT ( 'NONE',  ( 0.2727639067037610499, 3.267716535433071279, 1.102362204724404160 ) ) ;
#32125 = DIRECTION ( 'NONE',  ( 1.734723475976806848E-16, -0.000000000000000000, 1.000000000000000000 ) ) ;
#32126 = ORIENTED_EDGE ( 'NONE', *, *, #48394, .F. ) ;
#32127 = LINE ( 'NONE', #16631, #34795 ) ;
#32128 = CARTESIAN_POINT ( 'NONE',  ( 0.000000000000000000, 1.574803149606302854, 0.000000000000000000 ) ) ;
#32129 = CARTESIAN_POINT ( 'NONE',  ( 2.295325967725798222, 1.744665796922353351, 0.3605850800666594580 ) ) ;
#32130 = VECTOR ( 'NONE', #29924, 39.37007874015748143 ) ;
#32131 = VERTEX_POINT ( 'NONE', #9882 ) ;
#32132 = CARTESIAN_POINT ( 'NONE',  ( -1.546216657190577770, 1.038502057849785887, -2.044459178825514645 ) ) ;
#32133 = CARTESIAN_POINT ( 'NONE',  ( -0.8942052331142552601, 3.267716535433071279, -7.512581982576723358E-16 ) ) ;
#32134 = LINE ( 'NONE', #36260, #30849 ) ;
#32135 = ORIENTED_EDGE ( 'NONE', *, *, #35014, .T. ) ;
#32136 = LINE ( 'NONE', #24638, #41183 ) ;
#32137 = DIRECTION ( 'NONE',  ( 1.734723475976806848E-16, -0.000000000000000000, 1.000000000000000000 ) ) ;
#32138 = ORIENTED_EDGE ( 'NONE', *, *, #39968, .F. ) ;
#32139 = CARTESIAN_POINT ( 'NONE',  ( 0.2727639067037604392, 3.346456692913386100, 0.5905511811023579360 ) ) ;
#32140 = AXIS2_PLACEMENT_3D ( 'NONE', #13950, #48758, #45660 ) ;
#32141 = CARTESIAN_POINT ( 'NONE',  ( 0.000000000000000000, 3.267716535433071279, 0.000000000000000000 ) ) ;
#32142 = CARTESIAN_POINT ( 'NONE',  ( 0.2727639067037602172, 3.267716535433071279, -2.088563196121306476 ) ) ;
#32143 = CARTESIAN_POINT ( 'NONE',  ( -1.091055626815042645, 3.346456692913386100, 2.204724409448808764 ) ) ;
#32144 = EDGE_CURVE ( 'NONE', #37337, #4877, #25882, .T. ) ;
#32145 = EDGE_CURVE ( 'NONE', #40985, #42971, #41630, .T. ) ;
#32146 = EDGE_CURVE ( 'NONE', #4115, #23868, #18895, .T. ) ;
#32147 = VERTEX_POINT ( 'NONE', #3145 ) ;
#32148 = ORIENTED_EDGE ( 'NONE', *, *, #9180, .T. ) ;
#32149 = CARTESIAN_POINT ( 'NONE',  ( -2.813308242715026886, 1.572884882776984794, 0.8968463675966862336 ) ) ;
#32150 = FACE_OUTER_BOUND ( 'NONE', #18663, .T. ) ;
#32151 = ORIENTED_EDGE ( 'NONE', *, *, #26951, .F. ) ;
#32152 = DIRECTION ( 'NONE',  ( -1.000000000000000000, -0.000000000000000000, -0.000000000000000000 ) ) ;
#32153 = DIRECTION ( 'NONE',  ( 1.000000000000000000, 0.000000000000000000, -3.469446951953613696E-16 ) ) ;
#32154 = VECTOR ( 'NONE', #10358, 39.37007874015748143 ) ;
#32155 = DIRECTION ( 'NONE',  ( 1.558091277195102803E-17, -1.000000000000000000, 1.150229170499808965E-16 ) ) ;
#32156 = DIRECTION ( 'NONE',  ( 0.000000000000000000, -1.000000000000000000, 0.000000000000000000 ) ) ;
#32157 = ORIENTED_EDGE ( 'NONE', *, *, #29945, .T. ) ;
#32158 = EDGE_LOOP ( 'NONE', ( #43717, #50251, #40222, #21044 ) ) ;
#32159 = CARTESIAN_POINT ( 'NONE',  ( -1.091055626815042645, 0.000000000000000000, -1.259842519685034690 ) ) ;
#32160 = DIRECTION ( 'NONE',  ( -0.01601477604151182663, 0.9998717552508123996, -0.000000000000000000 ) ) ;
#32161 = LINE ( 'NONE', #18814, #23051 ) ;
#32162 = PLANE ( 'NONE',  #47895 ) ;
#32163 = FACE_BOUND ( 'NONE', #47772, .T. ) ;
#32164 = ORIENTED_EDGE ( 'NONE', *, *, #15068, .F. ) ;
#32165 = DIRECTION ( 'NONE',  ( -1.000000000000000000, 0.000000000000000000, 0.000000000000000000 ) ) ;
#32166 = ORIENTED_EDGE ( 'NONE', *, *, #11346, .F. ) ;
#32167 = ORIENTED_EDGE ( 'NONE', *, *, #10921, .T. ) ;
#32168 = EDGE_CURVE ( 'NONE', #351, #44517, #25949, .T. ) ;
#32169 = FACE_OUTER_BOUND ( 'NONE', #21052, .T. ) ;
#32170 = EDGE_CURVE ( 'NONE', #23287, #31073, #45685, .T. ) ;
#32171 = VECTOR ( 'NONE', #44769, 39.37007874015748143 ) ;
#32172 = VERTEX_POINT ( 'NONE', #49832 ) ;
#32173 = ORIENTED_EDGE ( 'NONE', *, *, #24037, .T. ) ;
#32174 = DIRECTION ( 'NONE',  ( -3.469446951953613696E-16, 0.000000000000000000, -1.000000000000000000 ) ) ;
#32175 = EDGE_CURVE ( 'NONE', #39052, #23451, #10646, .T. ) ;
#32176 = ORIENTED_EDGE ( 'NONE', *, *, #50307, .F. ) ;
#32177 = EDGE_CURVE ( 'NONE', #38883, #49063, #38525, .T. ) ;
#32178 = LINE ( 'NONE', #32696, #3979 ) ;
#32179 = DIRECTION ( 'NONE',  ( -0.000000000000000000, 1.000000000000000000, -0.000000000000000000 ) ) ;
#32180 = CARTESIAN_POINT ( 'NONE',  ( -2.138597145901436125, 1.574803149606302854, 0.3393547186366939750 ) ) ;
#32181 = VECTOR ( 'NONE', #45348, 39.37007874015748143 ) ;
#32182 = AXIS2_PLACEMENT_3D ( 'NONE', #20208, #599, #20468 ) ;
#32183 = CARTESIAN_POINT ( 'NONE',  ( 0.000000000000000000, 0.000000000000000000, 0.000000000000000000 ) ) ;
#32184 = DIRECTION ( 'NONE',  ( -0.000000000000000000, 1.000000000000000000, -0.000000000000000000 ) ) ;
#32185 = CARTESIAN_POINT ( 'NONE',  ( 1.909347346926324684, 3.267716535433071279, -3.312189666507128175E-16 ) ) ;
#32186 = ORIENTED_EDGE ( 'NONE', *, *, #7617, .T. ) ;
#32187 = DIRECTION ( 'NONE',  ( 1.509903313490212895E-14, 0.000000000000000000, 1.000000000000000000 ) ) ;
#32188 = VECTOR ( 'NONE', #31494, 39.37007874015748143 ) ;
#32189 = DIRECTION ( 'NONE',  ( 0.000000000000000000, 0.000000000000000000, -1.000000000000000000 ) ) ;
#32190 = CARTESIAN_POINT ( 'NONE',  ( 1.672606463373375485, 0.000000000000000000, 0.4917175957957914401 ) ) ;
#32191 = ORIENTED_EDGE ( 'NONE', *, *, #32007, .T. ) ;
#32192 = DIRECTION ( 'NONE',  ( 0.1785568947986229116, 0.000000000000000000, 0.9839295885986321100 ) ) ;
#32193 = FACE_OUTER_BOUND ( 'NONE', #33345, .T. ) ;
#32194 = ORIENTED_EDGE ( 'NONE', *, *, #24391, .T. ) ;
#32195 = CARTESIAN_POINT ( 'NONE',  ( 2.695799277629594037, 1.205361022782829114E-17, -1.205759334241453651 ) ) ;
#32196 = CARTESIAN_POINT ( 'NONE',  ( -1.363819533518803473, 0.000000000000000000, -1.102362204724405270 ) ) ;
#32197 = DIRECTION ( 'NONE',  ( 0.000000000000000000, 0.000000000000000000, 1.000000000000000000 ) ) ;
#32198 = ORIENTED_EDGE ( 'NONE', *, *, #10527, .T. ) ;
#32199 = CARTESIAN_POINT ( 'NONE',  ( 0.000000000000000000, 3.267716535433071279, -0.1574803149606297248 ) ) ;
#32200 = ORIENTED_EDGE ( 'NONE', *, *, #2967, .T. ) ;
#32201 = FACE_OUTER_BOUND ( 'NONE', #40328, .T. ) ;
#32202 = DIRECTION ( 'NONE',  ( 0.9998717552508121775, 0.01601477604151182663, 0.000000000000000000 ) ) ;
#32203 = LINE ( 'NONE', #13093, #38306 ) ;
#32204 = DIRECTION ( 'NONE',  ( -3.469446951953613696E-16, 0.000000000000000000, -1.000000000000000000 ) ) ;
#32205 = EDGE_CURVE ( 'NONE', #40819, #21432, #24777, .T. ) ;
#32206 = ORIENTED_EDGE ( 'NONE', *, *, #42239, .F. ) ;
#32207 = EDGE_LOOP ( 'NONE', ( #3601, #44225, #24120, #9112 ) ) ;
#32208 = EDGE_CURVE ( 'NONE', #2168, #27199, #41884, .T. ) ;
#32209 = CARTESIAN_POINT ( 'NONE',  ( 0.000000000000000000, 6.692913385826772199, 0.000000000000000000 ) ) ;
#32210 = VERTEX_POINT ( 'NONE', #45219 ) ;
#32211 = CARTESIAN_POINT ( 'NONE',  ( -1.909347346926324462, 3.346456692913386100, 0.5905511811023582691 ) ) ;
#32212 = ORIENTED_EDGE ( 'NONE', *, *, #19340, .F. ) ;
#32213 = EDGE_CURVE ( 'NONE', #6661, #35582, #34399, .T. ) ;
#32214 = AXIS2_PLACEMENT_3D ( 'NONE', #40685, #33465, #5060 ) ;
#32215 = LINE ( 'NONE', #40214, #22343 ) ;
#32216 = VECTOR ( 'NONE', #12058, 39.37007874015748143 ) ;
#32217 = ORIENTED_EDGE ( 'NONE', *, *, #36248, .T. ) ;
#32218 = CARTESIAN_POINT ( 'NONE',  ( -2.168245791271168343, 1.685466330048090322, -2.004968704497279930 ) ) ;
#32219 = FACE_OUTER_BOUND ( 'NONE', #9308, .T. ) ;
#32220 = ORIENTED_EDGE ( 'NONE', *, *, #532, .T. ) ;
#32221 = DIRECTION ( 'NONE',  ( 0.000000000000000000, 0.000000000000000000, 1.000000000000000000 ) ) ;
#32222 = ORIENTED_EDGE ( 'NONE', *, *, #23994, .F. ) ;
#32223 = AXIS2_PLACEMENT_3D ( 'NONE', #3004, #2499, #14623 ) ;
#32224 = CARTESIAN_POINT ( 'NONE',  ( -2.813306909019601232, 1.675400517285150270, 0.8968504722891414982 ) ) ;
#32225 = EDGE_CURVE ( 'NONE', #31431, #36611, #40144, .T. ) ;
#32226 = ORIENTED_EDGE ( 'NONE', *, *, #6118, .F. ) ;
#32227 = ORIENTED_EDGE ( 'NONE', *, *, #17244, .T. ) ;
#32228 = CARTESIAN_POINT ( 'NONE',  ( 0.1968503937007876625, 3.267716535433071279, -6.829619984160665442E-17 ) ) ;
#32229 = LINE ( 'NONE', #47924, #23724 ) ;
#32230 = EDGE_CURVE ( 'NONE', #7280, #13250, #50598, .T. ) ;
#32231 = ORIENTED_EDGE ( 'NONE', *, *, #9901, .F. ) ;
#32232 = CARTESIAN_POINT ( 'NONE',  ( -0.3928349003157404762, 1.705466165868896988, 2.440311704409034554 ) ) ;
#32233 = EDGE_CURVE ( 'NONE', #16438, #9349, #6768, .T. ) ;
#32234 = ORIENTED_EDGE ( 'NONE', *, *, #20471, .T. ) ;
#32235 = CARTESIAN_POINT ( 'NONE',  ( 1.909347346926324684, 3.346456692913386100, 0.4724409448818868706 ) ) ;
#32236 = FACE_OUTER_BOUND ( 'NONE', #29997, .T. ) ;
#32237 = LINE ( 'NONE', #16227, #31354 ) ;
#32238 = ORIENTED_EDGE ( 'NONE', *, *, #25838, .F. ) ;
#32239 = ORIENTED_EDGE ( 'NONE', *, *, #26364, .T. ) ;
#32240 = LINE ( 'NONE', #47936, #5522 ) ;
#32241 = CARTESIAN_POINT ( 'NONE',  ( -1.983277435230861085, 1.585901007090198878, -1.828120848347478455 ) ) ;
#32242 = CARTESIAN_POINT ( 'NONE',  ( 0.4696143004045484903, 0.000000000000000000, 2.362204724409437961 ) ) ;
#32243 = CARTESIAN_POINT ( 'NONE',  ( -1.721723715434402058, 0.0002321930594665579301, 0.2828853756254362528 ) ) ;
#32244 = B_SPLINE_CURVE_WITH_KNOTS ( 'NONE', 3,
 ( #13688, #29429, #13942, #25810 ),
 .UNSPECIFIED., .F., .F.,
 ( 4, 4 ),
 ( 0.001790699833465591011, 0.004290724276823231105 ),
 .UNSPECIFIED. ) ;
#32245 = CARTESIAN_POINT ( 'NONE',  ( -0.9845150457423005319, 0.000000000000000000, -1.438794182654565601 ) ) ;
#32246 = CARTESIAN_POINT ( 'NONE',  ( 1.091055626815042645, 3.346456692913386100, -0.6299212598425181220 ) ) ;
#32247 = CIRCLE ( 'NONE', #38837, 2.165354330708661568 ) ;
#32248 = VECTOR ( 'NONE', #22493, 39.37007874015748143 ) ;
#32249 = CARTESIAN_POINT ( 'NONE',  ( 1.530693736245519521, 6.692913385826772199, -1.531579597454042707 ) ) ;
#32250 = EDGE_LOOP ( 'NONE', ( #14128, #4082, #48790, #3973 ) ) ;
#32251 = DIRECTION ( 'NONE',  ( 2.753352829315774182E-14, 0.000000000000000000, 1.000000000000000000 ) ) ;
#32252 = ORIENTED_EDGE ( 'NONE', *, *, #44685, .F. ) ;
#32253 = LINE ( 'NONE', #35360, #36648 ) ;
#32254 = AXIS2_PLACEMENT_3D ( 'NONE', #4651, #16526, #19861 ) ;
#32255 = ORIENTED_EDGE ( 'NONE', *, *, #35114, .T. ) ;
#32256 = PLANE ( 'NONE',  #317 ) ;
#32257 = VECTOR ( 'NONE', #31412, 39.37007874015748143 ) ;
#32258 = CARTESIAN_POINT ( 'NONE',  ( -1.350373579275921276, 0.006290961278228680842, 1.139832270491418553 ) ) ;
#32259 = DIRECTION ( 'NONE',  ( 1.000000000000000000, 0.000000000000000000, -3.469446951953613696E-16 ) ) ;
#32260 = DIRECTION ( 'NONE',  ( 1.000000000000000000, -0.000000000000000000, 0.000000000000000000 ) ) ;
#32261 = ORIENTED_EDGE ( 'NONE', *, *, #41371, .F. ) ;
#32262 = DIRECTION ( 'NONE',  ( 0.000000000000000000, 0.000000000000000000, 1.000000000000000000 ) ) ;
#32263 = ADVANCED_FACE ( 'NONE', ( #22016 ), #38276, .F. ) ;
#32264 = CARTESIAN_POINT ( 'NONE',  ( -2.497042144641281602, 1.050182909770654982, -0.5194553827013835834 ) ) ;
#32265 = EDGE_CURVE ( 'NONE', #50554, #17626, #10827, .T. ) ;
#32266 = B_SPLINE_CURVE_WITH_KNOTS ( 'NONE', 3,
 ( #10956, #3207, #34704, #3459 ),
 .UNSPECIFIED., .F., .F.,
 ( 4, 4 ),
 ( 3.361685337281771228E-07, 0.04732126538906464980 ),
 .UNSPECIFIED. ) ;
#32267 = ORIENTED_EDGE ( 'NONE', *, *, #23495, .F. ) ;
#32268 = CARTESIAN_POINT ( 'NONE',  ( -1.636583440222564301, 3.267716535433071279, 1.574803149606291530 ) ) ;
#32269 = ORIENTED_EDGE ( 'NONE', *, *, #49803, .F. ) ;
#32270 = EDGE_CURVE ( 'NONE', #25764, #15688, #45727, .T. ) ;
#32271 = LINE ( 'NONE', #12128, #29334 ) ;
#32272 = CARTESIAN_POINT ( 'NONE',  ( 0.2727639067037604947, 0.000000000000000000, -0.1574803149606298636 ) ) ;
#32273 = EDGE_CURVE ( 'NONE', #28312, #23622, #26633, .T. ) ;
#32274 = LINE ( 'NONE', #13165, #50199 ) ;
#32275 = ORIENTED_EDGE ( 'NONE', *, *, #13763, .T. ) ;
#32276 = ORIENTED_EDGE ( 'NONE', *, *, #26274, .F. ) ;
#32277 = CARTESIAN_POINT ( 'NONE',  ( 0.2727639067037610499, 3.346456692913386100, 1.102362204724404160 ) ) ;
#32278 = DIRECTION ( 'NONE',  ( 1.000000000000000000, 0.000000000000000000, 0.000000000000000000 ) ) ;
#32279 = FACE_BOUND ( 'NONE', #31486, .T. ) ;
#32280 = VECTOR ( 'NONE', #42710, 39.37007874015748143 ) ;
#32281 = VECTOR ( 'NONE', #27497, 39.37007874015748143 ) ;
#32282 = DIRECTION ( 'NONE',  ( 0.6427876096865403621, -0.7660444431189770143, 1.858431260983764056E-16 ) ) ;
#32283 = EDGE_CURVE ( 'NONE', #7558, #42367, #23776, .T. ) ;
#32284 = CARTESIAN_POINT ( 'NONE',  ( 1.834323595590318323, 0.000000000000000000, 1.151859023884926891 ) ) ;
#32285 = VERTEX_POINT ( 'NONE', #11901 ) ;
#32286 = LINE ( 'NONE', #47980, #27384 ) ;
#32287 = AXIS2_PLACEMENT_3D ( 'NONE', #34304, #38425, #21656 ) ;
#32288 = EDGE_CURVE ( 'NONE', #22473, #27704, #34212, .T. ) ;
#32289 = ORIENTED_EDGE ( 'NONE', *, *, #17240, .F. ) ;
#32290 = ORIENTED_EDGE ( 'NONE', *, *, #43894, .F. ) ;
#32291 = AXIS2_PLACEMENT_3D ( 'NONE', #22495, #34120, #1667 ) ;
#32292 = APPLICATION_PROTOCOL_DEFINITION ( 'draft international standard', 'automotive_design', 1998, #39127 ) ;
#32293 = EDGE_LOOP ( 'NONE', ( #49290, #45404, #7069, #2090 ) ) ;
#32294 = DIRECTION ( 'NONE',  ( -3.469446951953613696E-16, 0.000000000000000000, -1.000000000000000000 ) ) ;
#32295 = VECTOR ( 'NONE', #1895, 39.37007874015748143 ) ;
#32296 = CARTESIAN_POINT ( 'NONE',  ( 0.7697289541891751963, 1.731250765710271811, -2.850711116208678675 ) ) ;
#32297 = EDGE_CURVE ( 'NONE', #24184, #4725, #31528, .T. ) ;
#32298 = LINE ( 'NONE', #17063, #40761 ) ;
#32299 = DIRECTION ( 'NONE',  ( -3.469446951953613696E-16, 0.000000000000000000, -1.000000000000000000 ) ) ;
#32300 = ORIENTED_EDGE ( 'NONE', *, *, #15999, .T. ) ;
#32301 = ORIENTED_EDGE ( 'NONE', *, *, #30839, .T. ) ;
#32302 = FACE_OUTER_BOUND ( 'NONE', #2545, .T. ) ;
#32303 = FILL_AREA_STYLE ('',( #36685 ) ) ;
#32304 = CARTESIAN_POINT ( 'NONE',  ( -1.735586374879336535, 0.000000000000000000, -2.388829707800051327 ) ) ;
#32305 = EDGE_CURVE ( 'NONE', #36336, #15273, #11146, .T. ) ;
#32306 = DIRECTION ( 'NONE',  ( -3.469446951953613696E-16, 0.000000000000000000, -1.000000000000000000 ) ) ;
#32307 = PLANE ( 'NONE',  #14077 ) ;
#32308 = PLANE ( 'NONE',  #29251 ) ;
#32309 = CARTESIAN_POINT ( 'NONE',  ( 1.999177773822438553, 1.049866565877818125, 0.3204690814889624151 ) ) ;
#32310 = CARTESIAN_POINT ( 'NONE',  ( 1.687984952120845428, 3.346456692913386100, 1.259842519685033135 ) ) ;
#32311 = ORIENTED_EDGE ( 'NONE', *, *, #25347, .T. ) ;
#32312 = CARTESIAN_POINT ( 'NONE',  ( 2.182111253630085290, 3.346456692913386100, 0.1181102362204698858 ) ) ;
#32313 = CARTESIAN_POINT ( 'NONE',  ( -1.062992125984251413, 0.5905511811023621549, -1.181102362204724754 ) ) ;
#32314 = ORIENTED_EDGE ( 'NONE', *, *, #11737, .T. ) ;
#32315 = CIRCLE ( 'NONE', #10057, 2.164630168518208109 ) ;
#32316 = ORIENTED_EDGE ( 'NONE', *, *, #33540, .T. ) ;
#32317 = DIRECTION ( 'NONE',  ( -0.6579387259397027066, 0.000000000000000000, -0.7530714660036196273 ) ) ;
#32318 = VECTOR ( 'NONE', #30252, 39.37007874015748143 ) ;
#32319 = DIRECTION ( 'NONE',  ( 1.734723475976806848E-16, -0.000000000000000000, 1.000000000000000000 ) ) ;
#32320 = PLANE ( 'NONE',  #9035 ) ;
#32321 = ORIENTED_EDGE ( 'NONE', *, *, #7824, .T. ) ;
#32322 = AXIS2_PLACEMENT_3D ( 'NONE', #30939, #7940, #191 ) ;
#32323 = ORIENTED_EDGE ( 'NONE', *, *, #37245, .T. ) ;
#32324 = CARTESIAN_POINT ( 'NONE',  ( -0.6214413264104939882, 0.000000000000000000, 0.7874015748031456541 ) ) ;
#32325 = AXIS2_PLACEMENT_3D ( 'NONE', #38694, #45643, #46400 ) ;
#32326 = ORIENTED_EDGE ( 'NONE', *, *, #49425, .F. ) ;
#32327 = DIRECTION ( 'NONE',  ( 1.000000000000000000, 0.000000000000000000, 0.000000000000000000 ) ) ;
#32328 = ORIENTED_EDGE ( 'NONE', *, *, #42141, .T. ) ;
#32329 = ADVANCED_FACE ( 'NONE', ( #39015 ), #22, .F. ) ;
#32330 = AXIS2_PLACEMENT_3D ( 'NONE', #12566, #24449, #36581 ) ;
#32331 = DIRECTION ( 'NONE',  ( 0.000000000000000000, 0.000000000000000000, -1.000000000000000000 ) ) ;
#32332 = CARTESIAN_POINT ( 'NONE',  ( -0.5455278134075214336, 3.346456692913386100, -0.9448818897637762948 ) ) ;
#32333 = CARTESIAN_POINT ( 'NONE',  ( -1.636583440222564301, 3.267716535433071279, -1.141732283464563791 ) ) ;
#32334 = ADVANCED_FACE ( 'NONE', ( #35403 ), #43385, .F. ) ;
#32335 = EDGE_CURVE ( 'NONE', #36271, #40209, #38338, .T. ) ;
#32336 = EDGE_LOOP ( 'NONE', ( #35265, #22068, #20144, #41825 ) ) ;
#32337 = ORIENTED_EDGE ( 'NONE', *, *, #14793, .F. ) ;
#32338 = ORIENTED_EDGE ( 'NONE', *, *, #49471, .T. ) ;
#32339 = DIRECTION ( 'NONE',  ( -0.000000000000000000, 1.000000000000000000, -0.000000000000000000 ) ) ;
#32340 = VERTEX_POINT ( 'NONE', #19380 ) ;
#32341 = ORIENTED_EDGE ( 'NONE', *, *, #44032, .F. ) ;
#32342 = LINE ( 'NONE', #834, #37155 ) ;
#32343 = CARTESIAN_POINT ( 'NONE',  ( -1.377952755905510918, 0.000000000000000000, -4.133858267716536083 ) ) ;
#32344 = CARTESIAN_POINT ( 'NONE',  ( 0.5455278134075217666, 0.000000000000000000, 2.204724409448808764 ) ) ;
#32345 = ORIENTED_EDGE ( 'NONE', *, *, #30230, .F. ) ;
#32346 = DIRECTION ( 'NONE',  ( -0.000000000000000000, -1.000000000000000000, 0.000000000000000000 ) ) ;
#32347 = DIRECTION ( 'NONE',  ( 0.000000000000000000, -1.000000000000000000, 0.000000000000000000 ) ) ;
#32348 = CARTESIAN_POINT ( 'NONE',  ( 0.1067246931122726866, 0.02962905676920215767, 0.000000000000000000 ) ) ;
#32349 = ORIENTED_EDGE ( 'NONE', *, *, #16629, .F. ) ;
#32350 = CARTESIAN_POINT ( 'NONE',  ( 0.8912126068892033404, 0.000000000000000000, -1.812984823346281749 ) ) ;
#32351 = PLANE ( 'NONE',  #9585 ) ;
#32352 = ORIENTED_EDGE ( 'NONE', *, *, #25123, .F. ) ;
#32353 = DIRECTION ( 'NONE',  ( 1.000000000000000000, -0.000000000000000000, 0.000000000000000000 ) ) ;
#32354 = ORIENTED_EDGE ( 'NONE', *, *, #29718, .T. ) ;
#32355 = ORIENTED_EDGE ( 'NONE', *, *, #24140, .F. ) ;
#32356 = DIRECTION ( 'NONE',  ( 0.000000000000000000, 0.000000000000000000, -1.000000000000000000 ) ) ;
#32357 = CARTESIAN_POINT ( 'NONE',  ( 0.000000000000000000, 3.267716535433071279, 1.062992125984245639 ) ) ;
#32359 = AXIS2_PLACEMENT_3D ( 'NONE', #19063, #43051, #50756 ) ;
#32358 = DIRECTION ( 'NONE',  ( -3.469446951953613696E-16, 0.000000000000000000, -1.000000000000000000 ) ) ;
#32360 = EDGE_CURVE ( 'NONE', #31903, #35616, #23263, .T. ) ;
#32361 = CARTESIAN_POINT ( 'NONE',  ( -0.5455278134075214336, 3.346456692913386100, -0.6299212598425175669 ) ) ;
#32362 = DIRECTION ( 'NONE',  ( -0.01601477604151182663, 0.9998717552508123996, -0.000000000000000000 ) ) ;
#32363 = VERTEX_POINT ( 'NONE', #43638 ) ;
#32364 = ORIENTED_EDGE ( 'NONE', *, *, #5871, .T. ) ;
#32365 = AXIS2_PLACEMENT_3D ( 'NONE', #35005, #49940, #30376 ) ;
#32366 = DIRECTION ( 'NONE',  ( -1.000000000000000000, 0.000000000000000000, 0.000000000000000000 ) ) ;
#32367 = VECTOR ( 'NONE', #41936, 39.37007874015748143 ) ;
#32368 = ORIENTED_EDGE ( 'NONE', *, *, #4680, .T. ) ;
#32369 = CARTESIAN_POINT ( 'NONE',  ( 1.735113842587030497, 0.05571068913886997875, 0.8778189866238004235 ) ) ;
#32370 = EDGE_CURVE ( 'NONE', #38936, #3690, #31788, .T. ) ;
#32371 = DIRECTION ( 'NONE',  ( 1.734723475976806848E-16, 0.000000000000000000, 1.000000000000000000 ) ) ;
#32372 = AXIS2_PLACEMENT_3D ( 'NONE', #5176, #1304, #16285 ) ;
#32373 = EDGE_CURVE ( 'NONE', #30180, #24438, #19135, .T. ) ;
#32374 = CARTESIAN_POINT ( 'NONE',  ( -0.2865598533144464444, 0.007820411976265893850, 1.854687926664660758 ) ) ;
#32375 = FACE_OUTER_BOUND ( 'NONE', #50563, .T. ) ;
#32376 = CARTESIAN_POINT ( 'NONE',  ( -1.536664496436148184E-16, 0.000000000000000000, -0.8267716535433052849 ) ) ;
#32377 = ORIENTED_EDGE ( 'NONE', *, *, #37582, .T. ) ;
#32378 = CARTESIAN_POINT ( 'NONE',  ( -1.363819533518803029, 3.346456692913386100, 1.102362204724404160 ) ) ;
#32379 = EDGE_CURVE ( 'NONE', #14806, #48863, #10766, .T. ) ;
#32380 = CARTESIAN_POINT ( 'NONE',  ( -2.695799277629577162, 1.578813927010291218, -1.205759334241492731 ) ) ;
#32381 = EDGE_CURVE ( 'NONE', #20129, #33855, #34895, .T. ) ;
#32382 = ORIENTED_EDGE ( 'NONE', *, *, #31140, .F. ) ;
#32383 = DIRECTION ( 'NONE',  ( 0.000000000000000000, -1.000000000000000000, 0.000000000000000000 ) ) ;
#32384 = PLANE ( 'NONE',  #36038 ) ;
#32385 = LINE ( 'NONE', #40122, #16417 ) ;
#32386 = EDGE_LOOP ( 'NONE', ( #24115, #44325, #41998, #13144, #16075, #38366, #32799, #46119, #14585, #40845, #23469 ) ) ;
#32387 = DIRECTION ( 'NONE',  ( 1.000000000000000000, 0.000000000000000000, -3.469446951953613696E-16 ) ) ;
#32388 = CARTESIAN_POINT ( 'NONE',  ( -0.6214413264104939882, 3.267716535433071279, 1.220472440944875281 ) ) ;
#32389 = CARTESIAN_POINT ( 'NONE',  ( -0.1943412135031128696, 1.613985720517193245, -2.708314625670412035 ) ) ;
#32390 = ORIENTED_EDGE ( 'NONE', *, *, #9558, .F. ) ;
#32391 = PLANE ( 'NONE',  #43610 ) ;
#32392 = CARTESIAN_POINT ( 'NONE',  ( 0.000000000000000000, 3.267716535433071279, -0.3543307086614173040 ) ) ;
#32393 = ORIENTED_EDGE ( 'NONE', *, *, #32828, .T. ) ;
#32394 = CARTESIAN_POINT ( 'NONE',  ( -0.3486774197067334380, 0.000000000000000000, 1.889763779527550369 ) ) ;
#32395 = EDGE_CURVE ( 'NONE', #42, #16195, #47222, .T. ) ;
#32396 = CARTESIAN_POINT ( 'NONE',  ( -1.712496953225537188, 3.346456692913386100, -0.3543307086614171930 ) ) ;
#32397 = CARTESIAN_POINT ( 'NONE',  ( -2.277873973731453727, 1.683757167080951245, 1.879489153247634992 ) ) ;
#32398 = DIRECTION ( 'NONE',  ( -3.469446951953613696E-16, 0.000000000000000000, -1.000000000000000000 ) ) ;
#32399 = EDGE_CURVE ( 'NONE', #27803, #30813, #50577, .T. ) ;
#32400 = ADVANCED_FACE ( 'NONE', ( #31021 ), #44902, .T. ) ;
#32401 = VECTOR ( 'NONE', #38068, 39.37007874015748143 ) ;
#32402 = ORIENTED_EDGE ( 'NONE', *, *, #40714, .F. ) ;
#32403 = VERTEX_POINT ( 'NONE', #42877 ) ;
#32404 = DIRECTION ( 'NONE',  ( -9.390536051998861478E-17, -1.000000000000000000, 6.822623802544654332E-17 ) ) ;
#32405 = FACE_OUTER_BOUND ( 'NONE', #23599, .T. ) ;
#32406 = ORIENTED_EDGE ( 'NONE', *, *, #44627, .F. ) ;
#32407 = VECTOR ( 'NONE', #13153, 39.37007874015748143 ) ;
#32408 = CARTESIAN_POINT ( 'NONE',  ( 1.435629050127790629, 1.734437112858062235, -2.059699342362053542 ) ) ;
#32409 = CARTESIAN_POINT ( 'NONE',  ( 0.5455278134075211005, 0.000000000000000000, -1.456692913385822630 ) ) ;
#32410 = DIRECTION ( 'NONE',  ( 0.9959742939952397345, -1.160734090543304660E-16, -0.08963930890342654279 ) ) ;
#32411 = VECTOR ( 'NONE', #7777, 39.37007874015748143 ) ;
#32412 = CARTESIAN_POINT ( 'NONE',  ( 0.2727639067037604392, 3.346456692913386100, -1.299212598425193210 ) ) ;
#32413 = VECTOR ( 'NONE', #35094, 39.37007874015748143 ) ;
#32414 = ORIENTED_EDGE ( 'NONE', *, *, #27252, .T. ) ;
#32415 = ORIENTED_EDGE ( 'NONE', *, *, #16544, .T. ) ;
#32416 = DIRECTION ( 'NONE',  ( -0.000000000000000000, 1.000000000000000000, -0.000000000000000000 ) ) ;
#32417 = DIRECTION ( 'NONE',  ( 1.000000000000000000, 0.000000000000000000, 0.000000000000000000 ) ) ;
#32418 = CARTESIAN_POINT ( 'NONE',  ( 0.000000000000000000, 1.574803149606302854, 0.000000000000000000 ) ) ;
#32419 = LINE ( 'NONE', #17423, #33953 ) ;
#32420 = FACE_BOUND ( 'NONE', #48251, .T. ) ;
#32421 = VECTOR ( 'NONE', #22646, 39.37007874015748143 ) ;
#32422 = ORIENTED_EDGE ( 'NONE', *, *, #44835, .F. ) ;
#32423 = DIRECTION ( 'NONE',  ( -0.000000000000000000, -1.000000000000000000, -0.000000000000000000 ) ) ;
#32424 = VERTEX_POINT ( 'NONE', #50826 ) ;
#32425 = ORIENTED_EDGE ( 'NONE', *, *, #13450, .T. ) ;
#32426 = CARTESIAN_POINT ( 'NONE',  ( 0.7855418668307559971, 5.905511811023623991, -2.846347029613733870 ) ) ;
#32427 = ORIENTED_EDGE ( 'NONE', *, *, #39146, .T. ) ;
#32429 = VERTEX_POINT ( 'NONE', #46973 ) ;
#32428 = EDGE_CURVE ( 'NONE', #49749, #36594, #1538, .T. ) ;
#32430 = CARTESIAN_POINT ( 'NONE',  ( 1.363819533518803251, 3.346456692913386100, 1.220472440944875281 ) ) ;
#32431 = ORIENTED_EDGE ( 'NONE', *, *, #34363, .T. ) ;
#32432 = DIRECTION ( 'NONE',  ( 0.000000000000000000, -1.000000000000000000, 0.000000000000000000 ) ) ;
#32433 = DIRECTION ( 'NONE',  ( 4.884978838366539963E-14, 0.000000000000000000, 1.000000000000000000 ) ) ;
#32434 = ADVANCED_FACE ( 'NONE', ( #3906 ), #19635, .F. ) ;
#32435 = CARTESIAN_POINT ( 'NONE',  ( -1.439733046521776583, 3.267716535433071279, 4.995077429881868843E-16 ) ) ;
#32436 = EDGE_CURVE ( 'NONE', #38137, #2677, #4676, .T. ) ;
#32437 = EDGE_CURVE ( 'NONE', #34370, #33474, #39785, .T. ) ;
#32438 = PLANE ( 'NONE',  #44536 ) ;
#32439 = AXIS2_PLACEMENT_3D ( 'NONE', #13175, #9551, #17550 ) ;
#32440 = DIRECTION ( 'NONE',  ( -1.000000000000000000, 0.000000000000000000, -0.000000000000000000 ) ) ;
#32441 = LINE ( 'NONE', #28543, #18766 ) ;
#32442 = VERTEX_POINT ( 'NONE', #8289 ) ;
#32443 = DIRECTION ( 'NONE',  ( -3.469446951953613696E-16, 0.000000000000000000, -1.000000000000000000 ) ) ;
#32444 = AXIS2_PLACEMENT_3D ( 'NONE', #40126, #36259, #8879 ) ;
#32445 = PRESENTATION_STYLE_ASSIGNMENT (( #4554 ) ) ;
#32446 = CARTESIAN_POINT ( 'NONE',  ( 0.1067246931122726866, 0.02962905676920215767, 0.000000000000000000 ) ) ;
#32447 = CIRCLE ( 'NONE', #17582, 2.246510896728926010 ) ;
#32448 = VECTOR ( 'NONE', #43963, 39.37007874015748143 ) ;
#32449 = VERTEX_POINT ( 'NONE', #36176 ) ;
#32450 = CARTESIAN_POINT ( 'NONE',  ( -0.7303501086101935602, 5.905511811023623991, 2.086068174627930816 ) ) ;
#32451 = DIRECTION ( 'NONE',  ( -0.000000000000000000, 1.000000000000000000, -0.000000000000000000 ) ) ;
#32452 = ORIENTED_EDGE ( 'NONE', *, *, #47909, .F. ) ;
#32453 = CARTESIAN_POINT ( 'NONE',  ( 1.909347346926324684, 3.346456692913386100, 1.102362204724403938 ) ) ;
#32454 = EDGE_CURVE ( 'NONE', #2274, #5130, #5182, .T. ) ;
#32455 = CARTESIAN_POINT ( 'NONE',  ( 0.8182917201112824834, 0.000000000000000000, 1.220472440944875281 ) ) ;
#32456 = DIRECTION ( 'NONE',  ( -1.000000000000000000, 0.000000000000000000, 0.000000000000000000 ) ) ;
#32457 = VECTOR ( 'NONE', #13261, 39.37007874015748143 ) ;
#32458 = EDGE_LOOP ( 'NONE', ( #27501, #8531, #26134, #11319 ) ) ;
#32459 = CARTESIAN_POINT ( 'NONE',  ( -1.363819533518803695, 3.267716535433071279, 2.365849761790806473E-16 ) ) ;
#32460 = EDGE_CURVE ( 'NONE', #19826, #18320, #803, .T. ) ;
#32461 = ORIENTED_EDGE ( 'NONE', *, *, #35407, .F. ) ;
#32462 = FACE_BOUND ( 'NONE', #20822, .T. ) ;
#32463 = CARTESIAN_POINT ( 'NONE',  ( -0.2156685157583833057, 1.520013147563287648, -2.945280361644576850 ) ) ;
#32464 = DIRECTION ( 'NONE',  ( -1.000000000000000000, 0.000000000000000000, 0.000000000000000000 ) ) ;
#32465 = CARTESIAN_POINT ( 'NONE',  ( 0.5905511811023621549, 0.000000000000000000, -4.133858267716536083 ) ) ;
#32466 = EDGE_CURVE ( 'NONE', #41982, #30636, #1052, .T. ) ;
#32467 = EDGE_LOOP ( 'NONE', ( #2986, #13709, #40541, #8630 ) ) ;
#32468 = ORIENTED_EDGE ( 'NONE', *, *, #8498, .T. ) ;
#32469 = EDGE_CURVE ( 'NONE', #37445, #28425, #44956, .T. ) ;
#32470 = CARTESIAN_POINT ( 'NONE',  ( -0.6214413264104939882, 3.346456692913386100, 1.220472440944875281 ) ) ;
#32471 = EDGE_CURVE ( 'NONE', #13914, #43507, #1218, .T. ) ;
#32472 = ORIENTED_EDGE ( 'NONE', *, *, #3298, .F. ) ;
#32473 = B_SPLINE_CURVE_WITH_KNOTS ( 'NONE', 3,
 ( #16450, #43789, #15425, #20040 ),
 .UNSPECIFIED., .F., .F.,
 ( 4, 4 ),
 ( 2.008297004145147925E-07, 0.01822228745053504351 ),
 .UNSPECIFIED. ) ;
#32474 = CARTESIAN_POINT ( 'NONE',  ( 1.909347346926324684, 0.000000000000000000, 0.1574803149606280872 ) ) ;
#32475 = ORIENTED_EDGE ( 'NONE', *, *, #9758, .F. ) ;
#32476 = CARTESIAN_POINT ( 'NONE',  ( 1.015142113812069091, 3.346456692913386100, -1.732283464566923614 ) ) ;
#32477 = ORIENTED_EDGE ( 'NONE', *, *, #15002, .T. ) ;
#32478 = CARTESIAN_POINT ( 'NONE',  ( -1.712496953225537188, 0.000000000000000000, 0.4724409448818871482 ) ) ;
#32479 = VECTOR ( 'NONE', #22829, 39.37007874015748143 ) ;
#32480 = CARTESIAN_POINT ( 'NONE',  ( -2.160407304981126320, 1.673304745347873324, -0.1462862061266896330 ) ) ;
#32481 = VERTEX_POINT ( 'NONE', #47997 ) ;
#32482 = DIRECTION ( 'NONE',  ( 1.000000000000000000, 0.000000000000000000, 0.000000000000000000 ) ) ;
#32483 = ORIENTED_EDGE ( 'NONE', *, *, #16695, .F. ) ;
#32484 = VECTOR ( 'NONE', #8731, 39.37007874015748143 ) ;
#32485 = VECTOR ( 'NONE', #17760, 39.37007874015748143 ) ;
#32486 = CARTESIAN_POINT ( 'NONE',  ( -2.793030215715272213, 1.675725205278408403, 0.9592557174602281966 ) ) ;
#32487 = ORIENTED_EDGE ( 'NONE', *, *, #42585, .T. ) ;
#32488 = ORIENTED_EDGE ( 'NONE', *, *, #32170, .T. ) ;
#32489 = DIRECTION ( 'NONE',  ( -1.000000000000000000, -0.000000000000000000, -0.000000000000000000 ) ) ;
#32490 = VECTOR ( 'NONE', #31999, 39.37007874015748143 ) ;
#32491 = ORIENTED_EDGE ( 'NONE', *, *, #17695, .T. ) ;
#32492 = LINE ( 'NONE', #36358, #7297 ) ;
#32493 = ORIENTED_EDGE ( 'NONE', *, *, #19937, .F. ) ;
#32494 = CARTESIAN_POINT ( 'NONE',  ( 0.1155636338427008941, -0.5222242541845523167, 0.000000000000000000 ) ) ;
#32495 = DIRECTION ( 'NONE',  ( -3.986037398843765983E-20, -1.000000000000000000, -1.160734090543304660E-16 ) ) ;
#32496 = ADVANCED_FACE ( 'NONE', ( #43644 ), #14406, .T. ) ;
#32497 = DIRECTION ( 'NONE',  ( 5.063291518729136385E-17, 1.000000000000000000, -1.184615939703115601E-16 ) ) ;
#32498 = ORIENTED_EDGE ( 'NONE', *, *, #18761, .T. ) ;
#32499 = EDGE_CURVE ( 'NONE', #6449, #9844, #1311, .T. ) ;
#32500 = DIRECTION ( 'NONE',  ( -3.469446951953613696E-16, 0.000000000000000000, -1.000000000000000000 ) ) ;
#32501 = LINE ( 'NONE', #33015, #28744 ) ;
#32502 = EDGE_CURVE ( 'NONE', #39048, #36296, #43897, .T. ) ;
#32503 = CARTESIAN_POINT ( 'NONE',  ( -1.439733046521776139, 3.346456692913386100, -4.780733988912460139E-16 ) ) ;
#32504 = DIRECTION ( 'NONE',  ( 0.000000000000000000, 0.000000000000000000, -1.000000000000000000 ) ) ;
#32505 = FACE_OUTER_BOUND ( 'NONE', #18829, .T. ) ;
#32506 = CARTESIAN_POINT ( 'NONE',  ( 1.163887619842433718, 0.04656145577143805392, -1.518228404148327160 ) ) ;
#32507 = LINE ( 'NONE', #49216, #47379 ) ;
#32508 = ORIENTED_EDGE ( 'NONE', *, *, #12757, .T. ) ;
#32509 = CARTESIAN_POINT ( 'NONE',  ( -1.181102362204724310, 0.5905511811023621549, -1.181102362204724754 ) ) ;
#32510 = DIRECTION ( 'NONE',  ( -0.000000000000000000, 1.000000000000000000, -0.000000000000000000 ) ) ;
#32511 = AXIS2_PLACEMENT_3D ( 'NONE', #26866, #35138, #22260 ) ;
#32512 = ORIENTED_EDGE ( 'NONE', *, *, #1688, .F. ) ;
#32513 = PLANE ( 'NONE',  #25110 ) ;
#32514 = AXIS2_PLACEMENT_3D ( 'NONE', #3524, #19259, #45411 ) ;
#32515 = VECTOR ( 'NONE', #1624, 39.37007874015748143 ) ;
#32516 = ADVANCED_FACE ( 'NONE', ( #24810 ), #32834, .F. ) ;
#32517 = ORIENTED_EDGE ( 'NONE', *, *, #40974, .F. ) ;
#32518 = CARTESIAN_POINT ( 'NONE',  ( -1.712496953225537633, 0.000000000000000000, -0.4724409448818884805 ) ) ;
#32519 = VECTOR ( 'NONE', #44758, 39.37007874015748143 ) ;
#32521 = VECTOR ( 'NONE', #7782, 39.37007874015748854 ) ;
#32520 = CARTESIAN_POINT ( 'NONE',  ( -2.875073865522039807, 1.674437446067899682, -0.6730429437227067879 ) ) ;
#32522 = LINE ( 'NONE', #33035, #7248 ) ;
#32523 = ADVANCED_FACE ( 'NONE', ( #16556 ), #32308, .F. ) ;
#32524 = CARTESIAN_POINT ( 'NONE',  ( -0.06966273521059175577, -0.6299212598425202314, 0.3674709282358789575 ) ) ;
#32525 = DIRECTION ( 'NONE',  ( 5.782411586589357392E-17, 0.000000000000000000, 1.000000000000000000 ) ) ;
#32526 = ORIENTED_EDGE ( 'NONE', *, *, #24584, .T. ) ;
#32527 = CARTESIAN_POINT ( 'NONE',  ( 1.363819533518803251, 3.346456692913386100, -0.03937007874015908959 ) ) ;
#32528 = AXIS2_PLACEMENT_3D ( 'NONE', #27982, #20500, #36511 ) ;
#32529 = FACE_BOUND ( 'NONE', #4630, .T. ) ;
#32530 = EDGE_CURVE ( 'NONE', #42995, #45311, #48512, .T. ) ;
#32531 = EDGE_LOOP ( 'NONE', ( #29719, #25308, #11514, #48990, #49070 ) ) ;
#32532 = CARTESIAN_POINT ( 'NONE',  ( 0.1067246931122726866, 0.02962905676920215767, 0.000000000000000000 ) ) ;
#32533 = ORIENTED_EDGE ( 'NONE', *, *, #30695, .F. ) ;
#32534 = DIRECTION ( 'NONE',  ( -0.000000000000000000, 1.000000000000000000, -0.000000000000000000 ) ) ;
#32535 = DIRECTION ( 'NONE',  ( 0.000000000000000000, 0.000000000000000000, -1.000000000000000000 ) ) ;
#32536 = DIRECTION ( 'NONE',  ( -1.000000000000000000, 0.000000000000000000, -2.891205793294678326E-16 ) ) ;
#32537 = ORIENTED_EDGE ( 'NONE', *, *, #6096, .T. ) ;
#32538 = VERTEX_POINT ( 'NONE', #8802 ) ;
#32539 = CARTESIAN_POINT ( 'NONE',  ( 1.064142702668988694, 0.000000000000000000, -1.380941303491905359 ) ) ;
#32540 = CARTESIAN_POINT ( 'NONE',  ( 1.560669927219590747, 3.267716535433071279, -5.414661521997677271E-16 ) ) ;
#32541 = FACE_BOUND ( 'NONE', #7330, .T. ) ;
#32542 = PLANE ( 'NONE',  #39391 ) ;
#32543 = DIRECTION ( 'NONE',  ( -0.000000000000000000, 1.000000000000000000, -0.000000000000000000 ) ) ;
#32544 = ORIENTED_EDGE ( 'NONE', *, *, #32454, .T. ) ;
#32545 = B_SPLINE_CURVE_WITH_KNOTS ( 'NONE', 3,
 ( #26031, #6161, #45619, #3045 ),
 .UNSPECIFIED., .F., .F.,
 ( 4, 4 ),
 ( 2.329854597834415671E-07, 0.01900427930416172251 ),
 .UNSPECIFIED. ) ;
#32546 = DIRECTION ( 'NONE',  ( 0.000000000000000000, 0.000000000000000000, 1.000000000000000000 ) ) ;
#32547 = VECTOR ( 'NONE', #30585, 39.37007874015748854 ) ;
#32548 = VERTEX_POINT ( 'NONE', #24550 ) ;
#32549 = VECTOR ( 'NONE', #5704, 39.37007874015748143 ) ;
#32550 = VERTEX_POINT ( 'NONE', #40306 ) ;
#32551 = VECTOR ( 'NONE', #19036, 39.37007874015748143 ) ;
#32552 = ORIENTED_EDGE ( 'NONE', *, *, #11007, .T. ) ;
#32553 = CARTESIAN_POINT ( 'NONE',  ( -1.905671854841497259, 1.205361022782829114E-17, 2.256015092822653667 ) ) ;
#32554 = AXIS2_PLACEMENT_3D ( 'NONE', #23665, #40453, #28046 ) ;
#32555 = DIRECTION ( 'NONE',  ( -0.9998717552508121775, -0.01601477604151182663, 0.000000000000000000 ) ) ;
#32556 = DIRECTION ( 'NONE',  ( -3.469446951953613696E-16, 0.000000000000000000, -1.000000000000000000 ) ) ;
#32557 = LINE ( 'NONE', #9051, #32967 ) ;
#32558 = VERTEX_POINT ( 'NONE', #48258 ) ;
#32559 = ORIENTED_EDGE ( 'NONE', *, *, #1623, .F. ) ;
#32560 = EDGE_CURVE ( 'NONE', #21618, #20329, #28929, .T. ) ;
#32561 = AXIS2_PLACEMENT_3D ( 'NONE', #43285, #19792, #27031 ) ;
#32562 = CARTESIAN_POINT ( 'NONE',  ( 1.472697644137372697, 1.731489898814932316, 1.760436233057293354 ) ) ;
#32563 = DIRECTION ( 'NONE',  ( 0.000000000000000000, -1.000000000000000000, 0.000000000000000000 ) ) ;
#32564 = EDGE_CURVE ( 'NONE', #9285, #35070, #3471, .T. ) ;
#32565 = DIRECTION ( 'NONE',  ( -0.000000000000000000, -1.000000000000000000, -0.000000000000000000 ) ) ;
#32566 = LINE ( 'NONE', #24807, #21858 ) ;
#32567 = EDGE_CURVE ( 'NONE', #47504, #42496, #50647, .T. ) ;
#32568 = DIRECTION ( 'NONE',  ( -1.000000000000000000, 0.000000000000000000, 1.734723475976806848E-16 ) ) ;
#32569 = CARTESIAN_POINT ( 'NONE',  ( 1.909347346926324462, 0.000000000000000000, -0.7874015748031473194 ) ) ;
#32570 = EDGE_CURVE ( 'NONE', #24648, #34110, #10339, .T. ) ;
#32571 = DIRECTION ( 'NONE',  ( -1.000000000000000000, 0.000000000000000000, -0.000000000000000000 ) ) ;
#32572 = DIRECTION ( 'NONE',  ( 0.000000000000000000, 1.000000000000000000, 0.000000000000000000 ) ) ;
#32573 = ORIENTED_EDGE ( 'NONE', *, *, #27977, .F. ) ;
#32574 = CARTESIAN_POINT ( 'NONE',  ( 1.549689501921142964, 1.667106268065684738, 1.698964208316597446 ) ) ;
#32575 = CARTESIAN_POINT ( 'NONE',  ( 1.636583440222563857, 3.346456692913386100, 0.7480314960629872445 ) ) ;
#32576 = ORIENTED_EDGE ( 'NONE', *, *, #13200, .T. ) ;
#32577 = ORIENTED_EDGE ( 'NONE', *, *, #40903, .T. ) ;
#32578 = LINE ( 'NONE', #36960, #48786 ) ;
#32579 = CARTESIAN_POINT ( 'NONE',  ( 3.927031490892378253E-16, 0.000000000000000000, 1.062992125984246083 ) ) ;
#32580 = EDGE_CURVE ( 'NONE', #19845, #43301, #45673, .T. ) ;
#32581 = CARTESIAN_POINT ( 'NONE',  ( -0.2727639067037602172, 0.000000000000000000, 1.102362204724404160 ) ) ;
#32582 = ORIENTED_EDGE ( 'NONE', *, *, #24506, .F. ) ;
#32583 = VECTOR ( 'NONE', #26079, 39.37007874015748143 ) ;
#32584 = AXIS2_PLACEMENT_3D ( 'NONE', #8945, #16445, #24187 ) ;
#32585 = EDGE_CURVE ( 'NONE', #13057, #24863, #41834, .T. ) ;
#32586 = ORIENTED_EDGE ( 'NONE', *, *, #17274, .F. ) ;
#32587 = AXIS2_PLACEMENT_3D ( 'NONE', #38964, #31227, #42583 ) ;
#32588 = DIRECTION ( 'NONE',  ( -1.000000000000000000, 0.000000000000000000, 1.734723475976806848E-16 ) ) ;
#32589 = ORIENTED_EDGE ( 'NONE', *, *, #32067, .T. ) ;
#32590 = VECTOR ( 'NONE', #15859, 39.37007874015748143 ) ;
#32591 = ORIENTED_EDGE ( 'NONE', *, *, #43544, .T. ) ;
#32592 = DIRECTION ( 'NONE',  ( -0.000000000000000000, 1.000000000000000000, -0.000000000000000000 ) ) ;
#32593 = DIRECTION ( 'NONE',  ( -0.000000000000000000, 1.000000000000000000, -0.000000000000000000 ) ) ;
#32594 = CARTESIAN_POINT ( 'NONE',  ( 0.1968503937007878568, 3.346456692913386100, 0.9448818897637749625 ) ) ;
#32595 = ORIENTED_EDGE ( 'NONE', *, *, #9303, .F. ) ;
#32596 = ORIENTED_EDGE ( 'NONE', *, *, #50163, .T. ) ;
#32597 = ORIENTED_EDGE ( 'NONE', *, *, #43360, .T. ) ;
#32598 = VECTOR ( 'NONE', #36073, 39.37007874015748143 ) ;
#32599 = FACE_OUTER_BOUND ( 'NONE', #31673, .T. ) ;
#32600 = ORIENTED_EDGE ( 'NONE', *, *, #29046, .T. ) ;
#32601 = ORIENTED_EDGE ( 'NONE', *, *, #48014, .T. ) ;
#32602 = CARTESIAN_POINT ( 'NONE',  ( 0.1968503937007877735, 3.346456692913386100, 1.062992125984246083 ) ) ;
#32603 = CARTESIAN_POINT ( 'NONE',  ( -0.2727639067037607723, 0.000000000000000000, -0.7874015748031470974 ) ) ;
#32604 = CARTESIAN_POINT ( 'NONE',  ( 2.725796967338451449, 1.659824354563097737, 0.3195722353185223019 ) ) ;
#32605 = ADVANCED_FACE ( 'NONE', ( #36952 ), #13958, .T. ) ;
#32606 = EDGE_LOOP ( 'NONE', ( #39179, #18909, #32945, #8084 ) ) ;
#32607 = DIRECTION ( 'NONE',  ( -1.000000000000000000, 0.000000000000000000, 1.734723475976806848E-16 ) ) ;
#32608 = CARTESIAN_POINT ( 'NONE',  ( 0.1968503937007872462, 0.000000000000000000, -0.8267716535433052849 ) ) ;
#32609 = CARTESIAN_POINT ( 'NONE',  ( -1.672606463373382590, 0.000000000000000000, 0.4917175957957677923 ) ) ;
#32610 = ORIENTED_EDGE ( 'NONE', *, *, #7985, .F. ) ;
#32611 = LINE ( 'NONE', #40856, #24909 ) ;
#32612 = CARTESIAN_POINT ( 'NONE',  ( 0.000000000000000000, 1.574803149606302854, 0.000000000000000000 ) ) ;
#32613 = CARTESIAN_POINT ( 'NONE',  ( -0.8182917201112819283, 0.000000000000000000, -0.03937007874015895081 ) ) ;
#32614 = ORIENTED_EDGE ( 'NONE', *, *, #40571, .T. ) ;
#32615 = VERTEX_POINT ( 'NONE', #2084 ) ;
#32616 = LINE ( 'NONE', #48562, #17211 ) ;
#32617 = CARTESIAN_POINT ( 'NONE',  ( -2.454875160333845674, 0.000000000000000000, 0.1574803149606286423 ) ) ;
#32618 = CARTESIAN_POINT ( 'NONE',  ( -0.8182917201112819283, 3.346456692913386100, 2.047244094488179567 ) ) ;
#32619 = PLANE ( 'NONE',  #28774 ) ;
#32620 = VERTEX_POINT ( 'NONE', #14206 ) ;
#32621 = EDGE_LOOP ( 'NONE', ( #34264, #16801, #23363, #32267 ) ) ;
#32622 = VECTOR ( 'NONE', #27584, 39.37007874015748143 ) ;
#32623 = B_SPLINE_CURVE_WITH_KNOTS ( 'NONE', 3,
 ( #30906, #7657, #19522, #35286 ),
 .UNSPECIFIED., .F., .F.,
 ( 4, 4 ),
 ( 2.102925093913365354E-07, 0.01991504288061870728 ),
 .UNSPECIFIED. ) ;
#32624 = ADVANCED_FACE ( 'NONE', ( #21452 ), #34092, .F. ) ;
#32625 = VECTOR ( 'NONE', #167, 39.37007874015748143 ) ;
#32626 = CARTESIAN_POINT ( 'NONE',  ( -0.04921259842519758176, 5.905511811023623991, -2.165433070866141119 ) ) ;
#32627 = ORIENTED_EDGE ( 'NONE', *, *, #21494, .T. ) ;
#32628 = CARTESIAN_POINT ( 'NONE',  ( 0.4350747367505080065, 5.905511811023623991, -2.121846421795414717 ) ) ;
#32629 = LINE ( 'NONE', #48321, #2838 ) ;
#32630 = AXIS2_PLACEMENT_3D ( 'NONE', #19409, #23542, #39806 ) ;
#32631 = EDGE_CURVE ( 'NONE', #31986, #29362, #48768, .T. ) ;
#32632 = EDGE_CURVE ( 'NONE', #46669, #50716, #29707, .T. ) ;
#32633 = VECTOR ( 'NONE', #47975, 39.37007874015748143 ) ;
#32634 = EDGE_CURVE ( 'NONE', #44754, #814, #21197, .T. ) ;
#32635 = CARTESIAN_POINT ( 'NONE',  ( -1.531732224425391253, 1.205361022782829114E-17, 0.8801458454442117052 ) ) ;
#32636 = CARTESIAN_POINT ( 'NONE',  ( 0.000000000000000000, 2.755905511811024056, 0.000000000000000000 ) ) ;
#32637 = CARTESIAN_POINT ( 'NONE',  ( -1.636583440222564301, 0.000000000000000000, -1.574803149606293307 ) ) ;
#32638 = VECTOR ( 'NONE', #25657, 39.37007874015748143 ) ;
#32639 = ORIENTED_EDGE ( 'NONE', *, *, #12047, .F. ) ;
#32640 = LINE ( 'NONE', #32378, #1933 ) ;
#32641 = DIRECTION ( 'NONE',  ( -1.000000000000000000, 0.000000000000000000, -0.000000000000000000 ) ) ;
#32642 = EDGE_LOOP ( 'NONE', ( #32526, #19477, #2950, #12281 ) ) ;
#32643 = DIRECTION ( 'NONE',  ( -3.469446951953613696E-16, 0.000000000000000000, -1.000000000000000000 ) ) ;
#32644 = CARTESIAN_POINT ( 'NONE',  ( 0.2727639067037609943, 0.000000000000000000, 1.220472440944875281 ) ) ;
#32645 = EDGE_CURVE ( 'NONE', #1280, #39907, #21824, .T. ) ;
#32646 = DIRECTION ( 'NONE',  ( -3.469446951953613696E-16, 0.000000000000000000, -1.000000000000000000 ) ) ;
#32647 = ORIENTED_EDGE ( 'NONE', *, *, #18132, .F. ) ;
#32648 = FACE_OUTER_BOUND ( 'NONE', #27399, .T. ) ;
#32649 = B_SPLINE_CURVE_WITH_KNOTS ( 'NONE', 3,
 ( #9170, #12795, #24670, #44013 ),
 .UNSPECIFIED., .F., .F.,
 ( 4, 4 ),
 ( 0.0009436092406449438433, 0.04779288783656267248 ),
 .UNSPECIFIED. ) ;
#32650 = CARTESIAN_POINT ( 'NONE',  ( 0.08139965876239094178, 1.610780518492231694, 0.000000000000000000 ) ) ;
#32651 = EDGE_CURVE ( 'NONE', #21491, #47610, #13448, .T. ) ;
#32652 = ORIENTED_EDGE ( 'NONE', *, *, #29104, .T. ) ;
#32653 = CARTESIAN_POINT ( 'NONE',  ( -1.166969139818015755, 3.267716535433071279, 0.5905511811023582691 ) ) ;
#32654 = CARTESIAN_POINT ( 'NONE',  ( -1.985260859929298016, 0.000000000000000000, -0.9448818897637762948 ) ) ;
#32655 = ORIENTED_EDGE ( 'NONE', *, *, #32672, .T. ) ;
#32656 = DIRECTION ( 'NONE',  ( -0.000000000000000000, 1.000000000000000000, -0.000000000000000000 ) ) ;
#32657 = LINE ( 'NONE', #11739, #16056 ) ;
#32658 = FACE_OUTER_BOUND ( 'NONE', #9757, .T. ) ;
#32659 = CARTESIAN_POINT ( 'NONE',  ( -1.363819533518803473, 0.000000000000000000, -1.102362204724405270 ) ) ;
#32660 = ADVANCED_FACE ( 'NONE', ( #25314 ), #45423, .T. ) ;
#32661 = CARTESIAN_POINT ( 'NONE',  ( -0.07591351300297340121, 3.346456692913386100, -0.9842519685039344823 ) ) ;
#32662 = ORIENTED_EDGE ( 'NONE', *, *, #46193, .T. ) ;
#32663 = ORIENTED_EDGE ( 'NONE', *, *, #11799, .F. ) ;
#32664 = CARTESIAN_POINT ( 'NONE',  ( 0.5756566573088583993, 1.629780628454260194, 2.896516654582643291 ) ) ;
#32665 = VECTOR ( 'NONE', #33, 39.37007874015748143 ) ;
#32666 = DIRECTION ( 'NONE',  ( -3.469446951953613696E-16, 0.000000000000000000, -1.000000000000000000 ) ) ;
#32667 = VECTOR ( 'NONE', #38460, 39.37007874015748143 ) ;
#32668 = ORIENTED_EDGE ( 'NONE', *, *, #44695, .F. ) ;
#32669 = CARTESIAN_POINT ( 'NONE',  ( 1.091055626815042423, 0.000000000000000000, -2.086614173228339641 ) ) ;
#32670 = PLANE ( 'NONE',  #35112 ) ;
#32671 = CARTESIAN_POINT ( 'NONE',  ( -2.946551303128973842, 1.574890269766889617, -0.1815919737934194866 ) ) ;
#32672 = EDGE_CURVE ( 'NONE', #22025, #20718, #17730, .T. ) ;
#32673 = AXIS2_PLACEMENT_3D ( 'NONE', #7378, #39119, #4013 ) ;
#32674 = DIRECTION ( 'NONE',  ( -3.469446951953613696E-16, 0.000000000000000000, -1.000000000000000000 ) ) ;
#32675 = ORIENTED_EDGE ( 'NONE', *, *, #48182, .T. ) ;
#32676 = ORIENTED_EDGE ( 'NONE', *, *, #2268, .F. ) ;
#32677 = CARTESIAN_POINT ( 'NONE',  ( -0.8942052331142552601, 3.267716535433071279, -0.8267716535433052849 ) ) ;
#32678 = LINE ( 'NONE', #40664, #7651 ) ;
#32679 = AXIS2_PLACEMENT_3D ( 'NONE', #19934, #35704, #15321 ) ;
#32680 = DIRECTION ( 'NONE',  ( -0.000000000000000000, 1.000000000000000000, -0.000000000000000000 ) ) ;
#32681 = ORIENTED_EDGE ( 'NONE', *, *, #5836, .F. ) ;
#32682 = DIRECTION ( 'NONE',  ( 0.01601477604151182663, -0.9998717552508123996, 0.000000000000000000 ) ) ;
#32684 = VECTOR ( 'NONE', #28060, 39.37007874015748143 ) ;
#32683 = FACE_BOUND ( 'NONE', #23641, .T. ) ;
#32685 = ORIENTED_EDGE ( 'NONE', *, *, #36596, .F. ) ;
#32686 = EDGE_CURVE ( 'NONE', #23722, #39604, #6481, .T. ) ;
#32687 = CARTESIAN_POINT ( 'NONE',  ( 3.937007874015748143, 2.755905511811027164, 1.181102362204724088 ) ) ;
#32688 = VERTEX_POINT ( 'NONE', #41079 ) ;
#32689 = ORIENTED_EDGE ( 'NONE', *, *, #29471, .T. ) ;
#32690 = DIRECTION ( 'NONE',  ( -0.000000000000000000, -1.000000000000000000, -0.000000000000000000 ) ) ;
#32691 = EDGE_CURVE ( 'NONE', #12432, #4560, #17575, .T. ) ;
#32692 = ORIENTED_EDGE ( 'NONE', *, *, #45281, .T. ) ;
#32693 = ORIENTED_EDGE ( 'NONE', *, *, #44666, .F. ) ;
#32694 = DIRECTION ( 'NONE',  ( -0.000000000000000000, 1.000000000000000000, -0.000000000000000000 ) ) ;
#32695 = ORIENTED_EDGE ( 'NONE', *, *, #32796, .F. ) ;
#32696 = CARTESIAN_POINT ( 'NONE',  ( 1.636583440222563635, 3.267716535433071279, -2.839019714148966584E-16 ) ) ;
#32697 = LINE ( 'NONE', #1945, #4671 ) ;
#32698 = CARTESIAN_POINT ( 'NONE',  ( -1.613153987106138443, 1.649255939716216091, -1.474246598108883699 ) ) ;
#32699 = EDGE_CURVE ( 'NONE', #30287, #22389, #49021, .T. ) ;
#32700 = VECTOR ( 'NONE', #27969, 39.37007874015748143 ) ;
#32701 = FACE_OUTER_BOUND ( 'NONE', #41432, .T. ) ;
#32702 = ADVANCED_FACE ( 'NONE', ( #2339 ), #9832, .F. ) ;
#32703 = CARTESIAN_POINT ( 'NONE',  ( 0.08119777152254364916, 1.623385212329073957, 0.000000000000000000 ) ) ;
#32704 = LINE ( 'NONE', #21068, #3098 ) ;
#32705 = VECTOR ( 'NONE', #14127, 39.37007874015748143 ) ;
#32706 = VERTEX_POINT ( 'NONE', #33595 ) ;
#32707 = DIRECTION ( 'NONE',  ( 0.000000000000000000, 0.000000000000000000, 1.000000000000000000 ) ) ;
#32708 = AXIS2_PLACEMENT_3D ( 'NONE', #39657, #11772, #32433 ) ;
#32709 = CIRCLE ( 'NONE', #40013, 0.8858267716535433989 ) ;
#32710 = LINE ( 'NONE', #33725, #2605 ) ;
#32711 = ORIENTED_EDGE ( 'NONE', *, *, #35989, .T. ) ;
#32712 = LINE ( 'NONE', #5832, #46261 ) ;
#32713 = LINE ( 'NONE', #43527, #3014 ) ;
#32714 = ORIENTED_EDGE ( 'NONE', *, *, #1693, .F. ) ;
#32715 = CARTESIAN_POINT ( 'NONE',  ( 0.000000000000000000, 3.267716535433071279, 0.000000000000000000 ) ) ;
#32716 = AXIS2_PLACEMENT_3D ( 'NONE', #49230, #3048, #38177 ) ;
#32717 = CARTESIAN_POINT ( 'NONE',  ( -2.808237744966007643, 0.000000000000000000, 0.9124517550441282321 ) ) ;
#32718 = LINE ( 'NONE', #48396, #11158 ) ;
#32719 = VECTOR ( 'NONE', #43678, 39.37007874015748143 ) ;
#32720 = ORIENTED_EDGE ( 'NONE', *, *, #24202, .F. ) ;
#32721 = DIRECTION ( 'NONE',  ( 1.000000000000000000, 0.000000000000000000, 0.000000000000000000 ) ) ;
#32722 = VERTEX_POINT ( 'NONE', #49282 ) ;
#32723 = FACE_BOUND ( 'NONE', #26339, .T. ) ;
#32724 = DIRECTION ( 'NONE',  ( 1.000000000000000000, 0.000000000000000000, -3.469446951953613696E-16 ) ) ;
#32725 = DIRECTION ( 'NONE',  ( 1.000000000000000000, -0.000000000000000000, 0.000000000000000000 ) ) ;
#32726 = CARTESIAN_POINT ( 'NONE',  ( 0.8182917201112817063, 3.346456692913386100, -1.732283464566923614 ) ) ;
#32727 = EDGE_CURVE ( 'NONE', #38070, #33610, #24361, .T. ) ;
#32728 = B_SPLINE_CURVE_WITH_KNOTS ( 'NONE', 3,
 ( #14158, #2543, #29907, #45621 ),
 .UNSPECIFIED., .F., .F.,
 ( 4, 4 ),
 ( 0.01073245408401574987, 0.03073581594907834336 ),
 .UNSPECIFIED. ) ;
#32729 = ORIENTED_EDGE ( 'NONE', *, *, #36893, .T. ) ;
#32730 = ORIENTED_EDGE ( 'NONE', *, *, #39385, .T. ) ;
#32731 = DIRECTION ( 'NONE',  ( -1.000000000000000000, 0.000000000000000000, 1.734723475976806848E-16 ) ) ;
#32732 = VERTEX_POINT ( 'NONE', #49529 ) ;
#32733 = DIRECTION ( 'NONE',  ( -1.000000000000000000, -0.000000000000000000, -0.000000000000000000 ) ) ;
#32734 = ORIENTED_EDGE ( 'NONE', *, *, #30471, .F. ) ;
#32735 = EDGE_CURVE ( 'NONE', #39288, #16952, #39216, .T. ) ;
#32736 = DIRECTION ( 'NONE',  ( -4.561975526775602830E-17, -1.000000000000000000, -1.067327232801823148E-16 ) ) ;
#32737 = EDGE_CURVE ( 'NONE', #5208, #46569, #40375, .T. ) ;
#32738 = ORIENTED_EDGE ( 'NONE', *, *, #1306, .F. ) ;
#32739 = DIRECTION ( 'NONE',  ( 0.6579387259397138088, 0.000000000000000000, -0.7530714660036099684 ) ) ;
#32740 = EDGE_CURVE ( 'NONE', #27093, #42728, #33450, .T. ) ;
#32741 = AXIS2_PLACEMENT_3D ( 'NONE', #43015, #27528, #43270 ) ;
#32742 = PLANE ( 'NONE',  #13310 ) ;
#32743 = CIRCLE ( 'NONE', #36002, 2.165354330708661568 ) ;
#32744 = ORIENTED_EDGE ( 'NONE', *, *, #10934, .T. ) ;
#32745 = CARTESIAN_POINT ( 'NONE',  ( -0.04921259842519708216, 1.620047916482694861, 2.952755905511811108 ) ) ;
#32746 = ORIENTED_EDGE ( 'NONE', *, *, #32761, .F. ) ;
#32747 = ORIENTED_EDGE ( 'NONE', *, *, #47162, .F. ) ;
#32748 = CONICAL_SURFACE ( 'NONE', #30259, 3.483074324928249421, 1.244861948955335196 ) ;
#32749 = ORIENTED_EDGE ( 'NONE', *, *, #47684, .T. ) ;
#32750 = ORIENTED_EDGE ( 'NONE', *, *, #49416, .F. ) ;
#32751 = EDGE_CURVE ( 'NONE', #35748, #41115, #40830, .T. ) ;
#32752 = CARTESIAN_POINT ( 'NONE',  ( -2.695799277629577162, 0.000000000000000000, -1.205759334241492509 ) ) ;
#32753 = B_SPLINE_CURVE_WITH_KNOTS ( 'NONE', 3,
 ( #37096, #36327, #47892, #17463 ),
 .UNSPECIFIED., .F., .F.,
 ( 4, 4 ),
 ( 4.200322152323451851E-07, 0.04489399771681849144 ),
 .UNSPECIFIED. ) ;
#32754 = VECTOR ( 'NONE', #25350, 39.37007874015748143 ) ;
#32755 = VERTEX_POINT ( 'NONE', #34595 ) ;
#32756 = CARTESIAN_POINT ( 'NONE',  ( 0.3136974817028392315, 0.000000000000000000, -2.936457595020219635 ) ) ;
#32757 = ORIENTED_EDGE ( 'NONE', *, *, #6109, .T. ) ;
#32758 = LINE ( 'NONE', #28600, #28547 ) ;
#32759 = ADVANCED_FACE ( 'NONE', ( #19582 ), #10840, .T. ) ;
#32760 = LINE ( 'NONE', #48439, #15652 ) ;
#32761 = EDGE_CURVE ( 'NONE', #46834, #528, #40965, .T. ) ;
#32762 = VERTEX_POINT ( 'NONE', #26831 ) ;
#32763 = CARTESIAN_POINT ( 'NONE',  ( -0.4358998810510941180, 1.610193826879650514, 2.677619307824346873 ) ) ;
#32764 = LINE ( 'NONE', #36621, #27082 ) ;
#32765 = PLANE ( 'NONE',  #24141 ) ;
#32766 = CARTESIAN_POINT ( 'NONE',  ( -1.722047146480845337, 0.0001160965347763901303, 0.2829291873374986666 ) ) ;
#32767 = CARTESIAN_POINT ( 'NONE',  ( 0.000000000000000000, 3.346456692913386100, 0.000000000000000000 ) ) ;
#32768 = DIRECTION ( 'NONE',  ( 1.734723475976806848E-16, -0.000000000000000000, 1.000000000000000000 ) ) ;
#32769 = LINE ( 'NONE', #20089, #13639 ) ;
#32770 = ORIENTED_EDGE ( 'NONE', *, *, #31572, .F. ) ;
#32771 = DIRECTION ( 'NONE',  ( -0.000000000000000000, 1.000000000000000000, -0.000000000000000000 ) ) ;
#32772 = AXIS2_PLACEMENT_3D ( 'NONE', #32348, #48041, #12719 ) ;
#32773 = VECTOR ( 'NONE', #7606, 39.37007874015748143 ) ;
#32775 = ADVANCED_FACE ( 'NONE', ( #43073 ), #46678, .T. ) ;
#32774 = CARTESIAN_POINT ( 'NONE',  ( 0.8182917201112817063, 3.267716535433071279, -2.047244094488181343 ) ) ;
#32776 = ORIENTED_EDGE ( 'NONE', *, *, #6224, .F. ) ;
#32777 = FACE_OUTER_BOUND ( 'NONE', #45676, .T. ) ;
#32778 = ORIENTED_EDGE ( 'NONE', *, *, #22868, .F. ) ;
#32779 = DIRECTION ( 'NONE',  ( 0.000000000000000000, 0.000000000000000000, 1.000000000000000000 ) ) ;
#32780 = PLANE ( 'NONE',  #47266 ) ;
#32781 = CARTESIAN_POINT ( 'NONE',  ( 0.000000000000000000, 3.346456692913386100, 0.000000000000000000 ) ) ;
#32782 = PLANE ( 'NONE',  #6969 ) ;
#32783 = CARTESIAN_POINT ( 'NONE',  ( 2.106197740627111514, 3.245701213390774331, -1.259299084540527192 ) ) ;
#32784 = ORIENTED_EDGE ( 'NONE', *, *, #42347, .T. ) ;
#32785 = FACE_OUTER_BOUND ( 'NONE', #1656, .T. ) ;
#32786 = CARTESIAN_POINT ( 'NONE',  ( 0.7720784846736921114, 1.727602517910236113, -2.612579414938067224 ) ) ;
#32787 = VERTEX_POINT ( 'NONE', #31476 ) ;
#32788 = DIRECTION ( 'NONE',  ( -0.000000000000000000, 1.000000000000000000, -0.000000000000000000 ) ) ;
#32789 = VECTOR ( 'NONE', #8737, 39.37007874015748143 ) ;
#32790 = ORIENTED_EDGE ( 'NONE', *, *, #10338, .T. ) ;
#32791 = CARTESIAN_POINT ( 'NONE',  ( -1.979793062125317471, 1.589971192595758698, 2.191257344206539948 ) ) ;
#32792 = LINE ( 'NONE', #28892, #42089 ) ;
#32793 = ADVANCED_FACE ( 'NONE', ( #51030 ), #11096, .F. ) ;
#32794 = PLANE ( 'NONE',  #37312 ) ;
#32795 = EDGE_CURVE ( 'NONE', #514, #12754, #34249, .T. ) ;
#32796 = EDGE_CURVE ( 'NONE', #22538, #45311, #26335, .T. ) ;
#32797 = DIRECTION ( 'NONE',  ( 0.000000000000000000, 0.000000000000000000, 1.000000000000000000 ) ) ;
#32798 = ORIENTED_EDGE ( 'NONE', *, *, #50032, .T. ) ;
#32799 = ORIENTED_EDGE ( 'NONE', *, *, #25290, .F. ) ;
#32800 = LINE ( 'NONE', #48481, #43276 ) ;
#32801 = DIRECTION ( 'NONE',  ( -1.000000000000000000, 0.000000000000000000, 0.000000000000000000 ) ) ;
#32802 = DIRECTION ( 'NONE',  ( -0.000000000000000000, 1.000000000000000000, -0.000000000000000000 ) ) ;
#32803 = VERTEX_POINT ( 'NONE', #3597 ) ;
#32804 = EDGE_CURVE ( 'NONE', #31365, #16345, #35097, .T. ) ;
#32805 = CARTESIAN_POINT ( 'NONE',  ( 1.039905234370930742, 0.000000000000000000, -0.5599999049406324536 ) ) ;
#32806 = CARTESIAN_POINT ( 'NONE',  ( -2.607960231842429089, 1.568825401333847402, 1.384767194071829577 ) ) ;
#32807 = VECTOR ( 'NONE', #41160, 39.37007874015748143 ) ;
#32808 = VECTOR ( 'NONE', #26839, 39.37007874015748143 ) ;
#32809 = ORIENTED_EDGE ( 'NONE', *, *, #41727, .F. ) ;
#32810 = DIRECTION ( 'NONE',  ( -0.3166081466550566548, 0.000000000000000000, -0.9485564197619718030 ) ) ;
#32811 = LINE ( 'NONE', #41059, #25390 ) ;
#32812 = ORIENTED_EDGE ( 'NONE', *, *, #46211, .T. ) ;
#32813 = VERTEX_POINT ( 'NONE', #42083 ) ;
#32814 = AXIS2_PLACEMENT_3D ( 'NONE', #29682, #25544, #37180 ) ;
#32815 = EDGE_CURVE ( 'NONE', #33586, #18815, #38721, .T. ) ;
#32816 = ORIENTED_EDGE ( 'NONE', *, *, #28262, .T. ) ;
#32817 = CARTESIAN_POINT ( 'NONE',  ( 0.8455406139730251569, 3.346456692913386100, -1.929133858267711110 ) ) ;
#32818 = CARTESIAN_POINT ( 'NONE',  ( -1.014069264286641570, 0.000000000000000000, -1.062992125984252301 ) ) ;
#32819 = ADVANCED_FACE ( 'NONE', ( #15476 ), #23490, .T. ) ;
#32820 = CARTESIAN_POINT ( 'NONE',  ( 0.002207914879453961969, 5.905511811023623991, 0.04916304461325442243 ) ) ;
#32821 = DIRECTION ( 'NONE',  ( 0.000000000000000000, 1.000000000000000000, -0.000000000000000000 ) ) ;
#32822 = EDGE_CURVE ( 'NONE', #25300, #24596, #16944, .T. ) ;
#32823 = VECTOR ( 'NONE', #4340, 39.37007874015748143 ) ;
#32824 = ORIENTED_EDGE ( 'NONE', *, *, #29887, .T. ) ;
#32825 = VERTEX_POINT ( 'NONE', #18597 ) ;
#32826 = CARTESIAN_POINT ( 'NONE',  ( 1.312623452344844566, 0.000000000000000000, 1.722945714930923744 ) ) ;
#32827 = FACE_OUTER_BOUND ( 'NONE', #23134, .T. ) ;
#32828 = EDGE_CURVE ( 'NONE', #11586, #46126, #50524, .T. ) ;
#32829 = PLANE ( 'NONE',  #26599 ) ;
#32830 = VECTOR ( 'NONE', #14333, 39.37007874015748143 ) ;
#32831 = EDGE_CURVE ( 'NONE', #31608, #22729, #9004, .T. ) ;
#32832 = LINE ( 'NONE', #48510, #25173 ) ;
#32833 = DIRECTION ( 'NONE',  ( -3.469446951953613696E-16, 0.000000000000000000, -1.000000000000000000 ) ) ;
#32834 = PLANE ( 'NONE',  #47344 ) ;
#32835 = LINE ( 'NONE', #48514, #48132 ) ;
#32836 = VERTEX_POINT ( 'NONE', #17011 ) ;
#32837 = DIRECTION ( 'NONE',  ( -0.01601477604151182663, 0.9998717552508123996, -0.000000000000000000 ) ) ;
#32838 = DIRECTION ( 'NONE',  ( -0.000000000000000000, 1.000000000000000000, -0.000000000000000000 ) ) ;
#32839 = ORIENTED_EDGE ( 'NONE', *, *, #4963, .T. ) ;
#32840 = EDGE_LOOP ( 'NONE', ( #45182, #31760, #38915, #31138 ) ) ;
#32841 = LINE ( 'NONE', #28937, #24925 ) ;
#32842 = LINE ( 'NONE', #9327, #24531 ) ;
#32843 = VECTOR ( 'NONE', #48663, 39.37007874015748143 ) ;
#32844 = ORIENTED_EDGE ( 'NONE', *, *, #16828, .F. ) ;
#32845 = AXIS2_PLACEMENT_3D ( 'NONE', #18285, #11044, #7175 ) ;
#32846 = EDGE_LOOP ( 'NONE', ( #28717, #26427, #15260, #39687, #30827 ) ) ;
#32847 = LINE ( 'NONE', #9332, #23755 ) ;
#32848 = AXIS2_PLACEMENT_3D ( 'NONE', #13817, #29561, #14316 ) ;
#32849 = VERTEX_POINT ( 'NONE', #47432 ) ;
#32850 = EDGE_LOOP ( 'NONE', ( #41874, #37778, #27617, #2665 ) ) ;
#32851 = AXIS2_PLACEMENT_3D ( 'NONE', #34422, #3423, #30542 ) ;
#32852 = CARTESIAN_POINT ( 'NONE',  ( -0.9664853984138626064, 0.008359359359691105260, 1.521674255078630633 ) ) ;
#32853 = CARTESIAN_POINT ( 'NONE',  ( 0.1324246528213921248, 1.049866565067838486, -2.020365292213844199 ) ) ;
#32854 = VECTOR ( 'NONE', #36300, 39.37007874015748143 ) ;
#32855 = EDGE_LOOP ( 'NONE', ( #11078, #46882, #50642, #16955 ) ) ;
#32856 = EDGE_CURVE ( 'NONE', #5165, #11356, #45739, .T. ) ;
#32857 = EDGE_LOOP ( 'NONE', ( #44206, #5401, #4435, #17346 ) ) ;
#32858 = ORIENTED_EDGE ( 'NONE', *, *, #39734, .T. ) ;
#32859 = DIRECTION ( 'NONE',  ( -0.000000000000000000, -1.000000000000000000, -0.000000000000000000 ) ) ;
#32860 = EDGE_CURVE ( 'NONE', #16575, #13729, #44357, .T. ) ;
#32861 = ORIENTED_EDGE ( 'NONE', *, *, #42637, .F. ) ;
#32862 = VERTEX_POINT ( 'NONE', #12618 ) ;
#32863 = CARTESIAN_POINT ( 'NONE',  ( -1.099260860659351247, 0.003500963706710694470, -1.429277301230134301 ) ) ;
#32864 = DIRECTION ( 'NONE',  ( 0.9839295885986296675, 1.288287287306305530E-16, 0.1785568947986370669 ) ) ;
#32865 = CARTESIAN_POINT ( 'NONE',  ( 2.823445274216730638, 1.763256531483745837, 0.8656477926280683466 ) ) ;
#32866 = AXIS2_PLACEMENT_3D ( 'NONE', #7029, #34654, #18399 ) ;
#32867 = EDGE_CURVE ( 'NONE', #12116, #162, #7035, .T. ) ;
#32868 = ORIENTED_EDGE ( 'NONE', *, *, #4328, .T. ) ;
#32869 = CARTESIAN_POINT ( 'NONE',  ( -1.091055626815042645, 3.346456692913386100, 1.870389530743259199 ) ) ;
#32870 = LINE ( 'NONE', #48550, #15140 ) ;
#32871 = CARTESIAN_POINT ( 'NONE',  ( 1.287906020515830585, 0.000000000000000000, 1.377952755905504256 ) ) ;
#32872 = ORIENTED_EDGE ( 'NONE', *, *, #47386, .T. ) ;
#32873 = DIRECTION ( 'NONE',  ( 1.000000000000000000, 0.000000000000000000, 0.000000000000000000 ) ) ;
#32874 = LINE ( 'NONE', #48556, #35118 ) ;
#32875 = FACE_OUTER_BOUND ( 'NONE', #27882, .T. ) ;
#32876 = EDGE_LOOP ( 'NONE', ( #43696, #2799, #44630, #47712 ) ) ;
#32877 = VERTEX_POINT ( 'NONE', #222 ) ;
#32878 = CARTESIAN_POINT ( 'NONE',  ( -1.166969139818015977, 3.267716535433071279, -1.102362204724405270 ) ) ;
#32879 = LINE ( 'NONE', #1616, #9093 ) ;
#32880 = EDGE_CURVE ( 'NONE', #38641, #46852, #29297, .T. ) ;
#32881 = AXIS2_PLACEMENT_3D ( 'NONE', #30614, #7375, #26478 ) ;
#32882 = DIRECTION ( 'NONE',  ( 1.000000000000000000, 0.000000000000000000, -3.469446951953613696E-16 ) ) ;
#32883 = DIRECTION ( 'NONE',  ( 1.734723475976806848E-16, -0.000000000000000000, 1.000000000000000000 ) ) ;
#32884 = ORIENTED_EDGE ( 'NONE', *, *, #39347, .F. ) ;
#32885 = ORIENTED_EDGE ( 'NONE', *, *, #24652, .F. ) ;
#32886 = ADVANCED_FACE ( 'NONE', ( #8492 ), #43587, .T. ) ;
#32887 = EDGE_CURVE ( 'NONE', #17616, #22523, #1253, .T. ) ;
#32888 = DIRECTION ( 'NONE',  ( 0.000000000000000000, 0.000000000000000000, -1.000000000000000000 ) ) ;
#32889 = VECTOR ( 'NONE', #38734, 39.37007874015748143 ) ;
#32890 = EDGE_LOOP ( 'NONE', ( #8295, #34055, #34849, #48028 ) ) ;
#32891 = CARTESIAN_POINT ( 'NONE',  ( 2.555365368299595323E-16, 6.692913385826772199, 2.086614173228346303 ) ) ;
#32892 = DIRECTION ( 'NONE',  ( 0.000000000000000000, 1.000000000000000000, 0.000000000000000000 ) ) ;
#32893 = VECTOR ( 'NONE', #5287, 39.37007874015748143 ) ;
#32894 = AXIS2_PLACEMENT_3D ( 'NONE', #39434, #19798, #35563 ) ;
#32895 = VECTOR ( 'NONE', #41323, 39.37007874015748143 ) ;
#32896 = LINE ( 'NONE', #12743, #34104 ) ;
#32897 = DIRECTION ( 'NONE',  ( -0.000000000000000000, 1.000000000000000000, -0.000000000000000000 ) ) ;
#32898 = CARTESIAN_POINT ( 'NONE',  ( 0.000000000000000000, 0.000000000000000000, 0.000000000000000000 ) ) ;
#32899 = ORIENTED_EDGE ( 'NONE', *, *, #24811, .T. ) ;
#32900 = LINE ( 'NONE', #48580, #32457 ) ;
#32901 = VECTOR ( 'NONE', #23405, 39.37007874015748143 ) ;
#32902 = CARTESIAN_POINT ( 'NONE',  ( 0.2727639067037609943, 0.000000000000000000, 2.165354330708650910 ) ) ;
#32903 = ORIENTED_EDGE ( 'NONE', *, *, #27819, .T. ) ;
#32904 = DIRECTION ( 'NONE',  ( -3.469446951953613696E-16, 0.000000000000000000, -1.000000000000000000 ) ) ;
#32905 = FACE_OUTER_BOUND ( 'NONE', #31571, .T. ) ;
#32906 = DIRECTION ( 'NONE',  ( -1.000000000000000000, 0.000000000000000000, 0.000000000000000000 ) ) ;
#32907 = ORIENTED_EDGE ( 'NONE', *, *, #33669, .T. ) ;
#32908 = DIRECTION ( 'NONE',  ( -1.000000000000000000, -0.000000000000000000, -0.000000000000000000 ) ) ;
#32909 = DIRECTION ( 'NONE',  ( 1.160734090543304660E-16, -1.000000000000000000, -0.000000000000000000 ) ) ;
#32910 = ORIENTED_EDGE ( 'NONE', *, *, #26826, .T. ) ;
#32911 = CARTESIAN_POINT ( 'NONE',  ( -0.2646829987305902576, 5.905511811023623991, -2.940868978332400463 ) ) ;
#32912 = CARTESIAN_POINT ( 'NONE',  ( 0.7423782071083092626, 3.267716535433071279, 1.574803149606291974 ) ) ;
#32913 = ORIENTED_EDGE ( 'NONE', *, *, #21667, .F. ) ;
#32914 = CARTESIAN_POINT ( 'NONE',  ( 1.833433833923351353, 0.000000000000000000, 0.1181102362204701633 ) ) ;
#32915 = CARTESIAN_POINT ( 'NONE',  ( 0.7381027496705270252, 1.632310643118564997, -2.859439394060913298 ) ) ;
#32916 = CARTESIAN_POINT ( 'NONE',  ( -1.712496953225538077, 3.267716535433071279, 5.941417334598193996E-16 ) ) ;
#32917 = CARTESIAN_POINT ( 'NONE',  ( -2.014567149787738654, 1.675634971041569443, -0.8075478974698888646 ) ) ;
#32918 = VECTOR ( 'NONE', #12445, 39.37007874015748143 ) ;
#32919 = DIRECTION ( 'NONE',  ( -1.000000000000000000, 0.000000000000000000, -0.000000000000000000 ) ) ;
#32920 = EDGE_CURVE ( 'NONE', #13018, #8462, #32769, .T. ) ;
#32921 = EDGE_LOOP ( 'NONE', ( #12655, #26621, #40662, #36340, #50180 ) ) ;
#32922 = VERTEX_POINT ( 'NONE', #747 ) ;
#32923 = CARTESIAN_POINT ( 'NONE',  ( -1.412929913228844203, 0.003568411354370746354, 1.063828730186929805 ) ) ;
#32924 = CARTESIAN_POINT ( 'NONE',  ( -1.712496953225537188, 0.000000000000000000, 0.4724409448818871482 ) ) ;
#32925 = EDGE_CURVE ( 'NONE', #2534, #39129, #35859, .T. ) ;
#32926 = EDGE_LOOP ( 'NONE', ( #7212, #24196, #10294, #41486 ) ) ;
#32927 = PLANE ( 'NONE',  #41537 ) ;
#32928 = CARTESIAN_POINT ( 'NONE',  ( -1.929629134066536134, 1.574803149606302854, 0.9824921284572128988 ) ) ;
#32929 = CARTESIAN_POINT ( 'NONE',  ( 0.5905511811023627100, 0.000000000000000000, 2.165354330708661568 ) ) ;
#32930 = EDGE_CURVE ( 'NONE', #7882, #8114, #24497, .T. ) ;
#32931 = CARTESIAN_POINT ( 'NONE',  ( -1.363819533518803473, 0.000000000000000000, -0.1574803149606300023 ) ) ;
#32932 = AXIS2_PLACEMENT_3D ( 'NONE', #39820, #12454, #9094 ) ;
#32933 = VECTOR ( 'NONE', #34460, 39.37007874015748143 ) ;
#32934 = ORIENTED_EDGE ( 'NONE', *, *, #24467, .T. ) ;
#32935 = EDGE_LOOP ( 'NONE', ( #42501, #39977, #24838, #16154 ) ) ;
#32936 = EDGE_CURVE ( 'NONE', #50505, #41557, #11844, .T. ) ;
#32937 = CARTESIAN_POINT ( 'NONE',  ( -0.8942052331142552601, 3.267716535433071279, -0.5118110236220467790 ) ) ;
#32938 = CARTESIAN_POINT ( 'NONE',  ( -1.733853452330418987, 0.0001488292986583184614, 0.1852043564780690432 ) ) ;
#32939 = PLANE ( 'NONE',  #3296 ) ;
#32940 = EDGE_CURVE ( 'NONE', #13074, #2445, #47688, .T. ) ;
#32941 = EDGE_LOOP ( 'NONE', ( #38858, #3766, #28423, #18079 ) ) ;
#32942 = VECTOR ( 'NONE', #22356, 39.37007874015748143 ) ;
#32943 = CARTESIAN_POINT ( 'NONE',  ( 1.761123562704336232, 3.267716535433071279, -1.259842519685035800 ) ) ;
#32944 = FACE_BOUND ( 'NONE', #15806, .T. ) ;
#32945 = ORIENTED_EDGE ( 'NONE', *, *, #31922, .F. ) ;
#32946 = CARTESIAN_POINT ( 'NONE',  ( 0.000000000000000000, 6.692913385826772199, 0.000000000000000000 ) ) ;
#32947 = ORIENTED_EDGE ( 'NONE', *, *, #15233, .T. ) ;
#32948 = EDGE_LOOP ( 'NONE', ( #16488, #18482, #50164, #15389, #24822, #38325, #25862, #20381, #49863, #41842, #22445, #35557, #4941, #4271, #43803, #34113, #22881, #37734, #33359, #17897 ) ) ;
#32949 = DIRECTION ( 'NONE',  ( 0.000000000000000000, 1.160734090543304660E-16, -1.000000000000000000 ) ) ;
#32950 = EDGE_CURVE ( 'NONE', #10560, #24016, #36626, .T. ) ;
#32951 = ORIENTED_EDGE ( 'NONE', *, *, #49492, .F. ) ;
#32952 = CARTESIAN_POINT ( 'NONE',  ( 2.106197740627112402, 3.267716535433071279, -0.02067487291359444701 ) ) ;
#32953 = VERTEX_POINT ( 'NONE', #28094 ) ;
#32954 = EDGE_CURVE ( 'NONE', #7498, #39188, #16497, .T. ) ;
#32955 = CARTESIAN_POINT ( 'NONE',  ( -0.9237497744857992021, 0.5249316475426863970, 1.642046528476600153 ) ) ;
#32956 = CARTESIAN_POINT ( 'NONE',  ( -0.6214413264104945434, 3.267716535433071279, -0.1574803149606301411 ) ) ;
#32957 = CARTESIAN_POINT ( 'NONE',  ( -1.326676825859837816, 1.205361022782829114E-17, -1.200346386814097999 ) ) ;
#32958 = VECTOR ( 'NONE', #41854, 39.37007874015748143 ) ;
#32959 = EDGE_CURVE ( 'NONE', #36931, #34717, #19837, .T. ) ;
#32960 = CARTESIAN_POINT ( 'NONE',  ( 0.000000000000000000, 3.267716535433071279, -1.614173228346451605 ) ) ;
#32961 = PLANE ( 'NONE',  #24502 ) ;
#32962 = DIRECTION ( 'NONE',  ( 1.000000000000000000, 0.000000000000000000, -3.469446951953613696E-16 ) ) ;
#32963 = ORIENTED_EDGE ( 'NONE', *, *, #6333, .T. ) ;
#32964 = CARTESIAN_POINT ( 'NONE',  ( 1.091055626815042645, 0.000000000000000000, 0.9448818897637746295 ) ) ;
#32965 = EDGE_CURVE ( 'NONE', #23085, #43121, #15973, .T. ) ;
#32966 = CARTESIAN_POINT ( 'NONE',  ( 1.909347346926324684, 3.346456692913386100, -0.6692913385826764205 ) ) ;
#32967 = VECTOR ( 'NONE', #20143, 39.37007874015748143 ) ;
#32968 = VERTEX_POINT ( 'NONE', #12107 ) ;
#32969 = PLANE ( 'NONE',  #24844 ) ;
#32970 = LINE ( 'NONE', #28043, #24466 ) ;
#32971 = ORIENTED_EDGE ( 'NONE', *, *, #24158, .T. ) ;
#32972 = DIRECTION ( 'NONE',  ( 1.000000000000000000, 0.000000000000000000, 0.000000000000000000 ) ) ;
#32973 = LINE ( 'NONE', #24186, #20140 ) ;
#32974 = LINE ( 'NONE', #13085, #40049 ) ;
#32975 = ORIENTED_EDGE ( 'NONE', *, *, #46228, .T. ) ;
#32976 = CARTESIAN_POINT ( 'NONE',  ( 0.7423782071083087075, 3.346456692913386100, 0.6299212598425161236 ) ) ;
#32977 = AXIS2_PLACEMENT_3D ( 'NONE', #4766, #116, #16647 ) ;
#32978 = ORIENTED_EDGE ( 'NONE', *, *, #30336, .T. ) ;
#32979 = FACE_BOUND ( 'NONE', #35224, .T. ) ;
#32980 = PLANE ( 'NONE',  #30031 ) ;
#32981 = CARTESIAN_POINT ( 'NONE',  ( 0.2727639067037604392, 0.000000000000000000, 0.2755905511810994302 ) ) ;
#32982 = DIRECTION ( 'NONE',  ( -1.000000000000000000, -0.000000000000000000, -0.000000000000000000 ) ) ;
#32983 = ORIENTED_EDGE ( 'NONE', *, *, #3887, .F. ) ;
#32984 = VERTEX_POINT ( 'NONE', #20360 ) ;
#32985 = LINE ( 'NONE', #25725, #32843 ) ;
#32986 = ORIENTED_EDGE ( 'NONE', *, *, #8889, .F. ) ;
#32987 = PLANE ( 'NONE',  #19483 ) ;
#32988 = ORIENTED_EDGE ( 'NONE', *, *, #34593, .F. ) ;
#32989 = EDGE_CURVE ( 'NONE', #26292, #22637, #40249, .T. ) ;
#32990 = DIRECTION ( 'NONE',  ( 1.000000000000000000, -0.000000000000000000, 0.000000000000000000 ) ) ;
#32991 = EDGE_CURVE ( 'NONE', #22720, #6064, #32507, .T. ) ;
#32992 = AXIS2_PLACEMENT_3D ( 'NONE', #20641, #9539, #32797 ) ;
#32993 = EDGE_LOOP ( 'NONE', ( #31245, #23887, #39795, #42414 ) ) ;
#32994 = CARTESIAN_POINT ( 'NONE',  ( -0.3486774197067339376, 0.000000000000000000, -0.6299212598425175669 ) ) ;
#32995 = EDGE_CURVE ( 'NONE', #31067, #11355, #37399, .T. ) ;
#32996 = CARTESIAN_POINT ( 'NONE',  ( -1.363819533518803473, 3.267716535433071279, -0.1574803149606300023 ) ) ;
#32997 = ORIENTED_EDGE ( 'NONE', *, *, #48596, .F. ) ;
#32998 = FACE_OUTER_BOUND ( 'NONE', #50745, .T. ) ;
#32999 = ORIENTED_EDGE ( 'NONE', *, *, #6619, .T. ) ;
#33000 = ORIENTED_EDGE ( 'NONE', *, *, #39730, .F. ) ;
#33001 = VECTOR ( 'NONE', #26326, 39.37007874015748143 ) ;
#33002 = ORIENTED_EDGE ( 'NONE', *, *, #15920, .T. ) ;
#33003 = ORIENTED_EDGE ( 'NONE', *, *, #22189, .T. ) ;
#33004 = CARTESIAN_POINT ( 'NONE',  ( 0.8182917201112824834, 0.000000000000000000, 1.220472440944875281 ) ) ;
#33005 = DIRECTION ( 'NONE',  ( -1.000000000000000000, 0.000000000000000000, -0.000000000000000000 ) ) ;
#33006 = ORIENTED_EDGE ( 'NONE', *, *, #12488, .F. ) ;
#33007 = AXIS2_PLACEMENT_3D ( 'NONE', #46512, #18674, #11178 ) ;
#33008 = DIRECTION ( 'NONE',  ( 1.734723475976806848E-16, -0.000000000000000000, 1.000000000000000000 ) ) ;
#33009 = VERTEX_POINT ( 'NONE', #29121 ) ;
#33010 = CARTESIAN_POINT ( 'NONE',  ( 0.002207914879453961969, 5.905511811023623991, 0.04916304461325442243 ) ) ;
#33011 = ADVANCED_FACE ( 'NONE', ( #21897 ), #26813, .T. ) ;
#33012 = CARTESIAN_POINT ( 'NONE',  ( 4.097771990496411591E-16, 3.267716535433071279, 2.106299212598425008 ) ) ;
#33013 = ORIENTED_EDGE ( 'NONE', *, *, #36178, .F. ) ;
#33014 = DIRECTION ( 'NONE',  ( -0.000000000000000000, -1.000000000000000000, -0.000000000000000000 ) ) ;
#33015 = CARTESIAN_POINT ( 'NONE',  ( -1.091055626815042201, 3.267716535433071279, 1.892679809432643896E-16 ) ) ;
#33016 = ORIENTED_EDGE ( 'NONE', *, *, #437, .F. ) ;
#33017 = LINE ( 'NONE', #13379, #20867 ) ;
#33018 = DIRECTION ( 'NONE',  ( -0.7071067811865486830, 0.000000000000000000, -0.7071067811865462405 ) ) ;
#33019 = FACE_OUTER_BOUND ( 'NONE', #15639, .T. ) ;
#33020 = EDGE_CURVE ( 'NONE', #36398, #30647, #14144, .T. ) ;
#33021 = LINE ( 'NONE', #13382, #21512 ) ;
#33022 = CARTESIAN_POINT ( 'NONE',  ( -2.308557526972533136, 0.000000000000000000, 1.841013194464759639 ) ) ;
#33023 = ORIENTED_EDGE ( 'NONE', *, *, #33872, .T. ) ;
#33024 = PLANE ( 'NONE',  #30383 ) ;
#33025 = ADVANCED_FACE ( 'NONE', ( #29897 ), #21391, .F. ) ;
#33026 = DIRECTION ( 'NONE',  ( 0.000000000000000000, 0.000000000000000000, -1.000000000000000000 ) ) ;
#33027 = VERTEX_POINT ( 'NONE', #21135 ) ;
#33028 = CARTESIAN_POINT ( 'NONE',  ( 1.363819533518803251, 3.267716535433071279, 0.2755905511810996522 ) ) ;
#33029 = EDGE_CURVE ( 'NONE', #30636, #23441, #41512, .T. ) ;
#33030 = ORIENTED_EDGE ( 'NONE', *, *, #24749, .T. ) ;
#33031 = LINE ( 'NONE', #32518, #9953 ) ;
#33032 = ADVANCED_FACE ( 'NONE', ( #22155 ), #31442, .T. ) ;
#33033 = PLANE ( 'NONE',  #9395 ) ;
#33034 = AXIS2_PLACEMENT_3D ( 'NONE', #14388, #23142, #46357 ) ;
#33035 = CARTESIAN_POINT ( 'NONE',  ( -1.325491792074585673, 1.205361022782829114E-17, -2.638988599164751481 ) ) ;
#33036 = VECTOR ( 'NONE', #6327, 39.37007874015748143 ) ;
#33037 = CARTESIAN_POINT ( 'NONE',  ( -1.363819533518803473, 0.000000000000000000, 1.732283464566920950 ) ) ;
#33038 = LINE ( 'NONE', #44617, #7920 ) ;
#33039 = ORIENTED_EDGE ( 'NONE', *, *, #2924, .T. ) ;
#33040 = CARTESIAN_POINT ( 'NONE',  ( 0.1968503937007878568, 3.346456692913386100, 2.204724409448808764 ) ) ;
#33041 = FACE_BOUND ( 'NONE', #43371, .T. ) ;
#33042 = VERTEX_POINT ( 'NONE', #45106 ) ;
#33043 = CARTESIAN_POINT ( 'NONE',  ( -1.595649168949286434, 0.0008099078524815457591, -0.7355326111394984157 ) ) ;
#33044 = AXIS2_PLACEMENT_3D ( 'NONE', #26300, #37935, #14683 ) ;
#33045 = ORIENTED_EDGE ( 'NONE', *, *, #29005, .T. ) ;
#33046 = ADVANCED_FACE ( 'NONE', ( #41014 ), #5886, .F. ) ;
#33047 = LINE ( 'NONE', #1784, #13677 ) ;
#33048 = CARTESIAN_POINT ( 'NONE',  ( 0.2727639067037610499, 3.346456692913386100, 1.732283464566921172 ) ) ;
#33049 = CARTESIAN_POINT ( 'NONE',  ( -1.675635838109289288, 1.648255178477637140, 1.399220266318809580 ) ) ;
#33050 = EDGE_CURVE ( 'NONE', #42744, #47368, #20607, .T. ) ;
#33051 = CARTESIAN_POINT ( 'NONE',  ( -1.442444474601640492, 0.004816277389180329341, -1.011116641508509995 ) ) ;
#33052 = EDGE_CURVE ( 'NONE', #6227, #9948, #29784, .T. ) ;
#33053 = VERTEX_POINT ( 'NONE', #2528 ) ;
#33054 = ORIENTED_EDGE ( 'NONE', *, *, #44150, .T. ) ;
#33055 = FACE_OUTER_BOUND ( 'NONE', #31262, .T. ) ;
#33056 = FACE_OUTER_BOUND ( 'NONE', #99, .T. ) ;
#33057 = FACE_BOUND ( 'NONE', #40712, .T. ) ;
#33058 = B_SPLINE_CURVE_WITH_KNOTS ( 'NONE', 3,
 ( #48866, #25670, #2183, #32938 ),
 .UNSPECIFIED., .F., .F.,
 ( 4, 4 ),
 ( 2.623928897500769106E-05, 0.05045977204837132774 ),
 .UNSPECIFIED. ) ;
#33059 = LINE ( 'NONE', #14179, #20436 ) ;
#33060 = CARTESIAN_POINT ( 'NONE',  ( 0.000000000000000000, 3.267716535433071279, 0.6299212598425164567 ) ) ;
#33061 = EDGE_LOOP ( 'NONE', ( #48032, #6682, #32868, #21103 ) ) ;
#33062 = CARTESIAN_POINT ( 'NONE',  ( 1.014069264286641570, 0.4235180831842794702, -1.062992125984252301 ) ) ;
#33063 = CARTESIAN_POINT ( 'NONE',  ( 0.4696143004045484348, 3.346456692913386100, 1.220472440944875281 ) ) ;
#33064 = ORIENTED_EDGE ( 'NONE', *, *, #9372, .T. ) ;
#33065 = ORIENTED_EDGE ( 'NONE', *, *, #32428, .T. ) ;
#33066 = ORIENTED_EDGE ( 'NONE', *, *, #21726, .F. ) ;
#33067 = CARTESIAN_POINT ( 'NONE',  ( -1.195183497228115035E-16, 0.000000000000000000, -0.6299212598425177889 ) ) ;
#33068 = VECTOR ( 'NONE', #38719, 39.37007874015748143 ) ;
#33069 = LINE ( 'NONE', #49513, #20860 ) ;
#33070 = AXIS2_PLACEMENT_3D ( 'NONE', #27677, #23302, #3184 ) ;
#33071 = CARTESIAN_POINT ( 'NONE',  ( -1.909347346926324906, 0.000000000000000000, -0.4724409448818884805 ) ) ;
#33072 = EDGE_CURVE ( 'NONE', #39002, #1491, #41768, .T. ) ;
#33073 = LINE ( 'NONE', #37959, #24731 ) ;
#33074 = ORIENTED_EDGE ( 'NONE', *, *, #5649, .F. ) ;
#33075 = ORIENTED_EDGE ( 'NONE', *, *, #30975, .F. ) ;
#33076 = DIRECTION ( 'NONE',  ( 0.000000000000000000, 0.000000000000000000, -1.000000000000000000 ) ) ;
#33077 = LINE ( 'NONE', #34343, #4022 ) ;
#33078 = CARTESIAN_POINT ( 'NONE',  ( 1.560669927219590525, 3.346456692913386100, -0.3543307086614178592 ) ) ;
#33079 = AXIS2_PLACEMENT_3D ( 'NONE', #38375, #13610, #37879 ) ;
#33080 = DIRECTION ( 'NONE',  ( -1.000000000000000000, 0.000000000000000000, 1.734723475976806848E-16 ) ) ;
#33081 = CARTESIAN_POINT ( 'NONE',  ( 0.000000000000000000, 3.267716535433071279, -2.086614173228340086 ) ) ;
#33082 = ADVANCED_FACE ( 'NONE', ( #25002 ), #18271, .F. ) ;
#33083 = DIRECTION ( 'NONE',  ( 0.000000000000000000, 0.000000000000000000, -1.000000000000000000 ) ) ;
#33084 =( BOUNDED_CURVE ( )  B_SPLINE_CURVE ( 3, ( #33833, #23141, #49515, #27003 ),
 .UNSPECIFIED., .F., .F. ) 
 B_SPLINE_CURVE_WITH_KNOTS ( ( 4, 4 ),
 ( 0.1232251794661485683, 0.1739699573040163205 ),
 .UNSPECIFIED. ) 
 CURVE ( )  GEOMETRIC_REPRESENTATION_ITEM ( )  RATIONAL_B_SPLINE_CURVE ( ( 1.000000000000000000, 0.9997854254717271072, 0.9997854254717271072, 1.000000000000000000 ) ) 
 REPRESENTATION_ITEM ( '' )  );
#33085 = ADVANCED_FACE ( 'NONE', ( #2272 ), #1510, .F. ) ;
#33086 = CARTESIAN_POINT ( 'NONE',  ( -1.711605288297850969, 0.0005051743623580321960, -0.3401845456954783464 ) ) ;
#33087 = EDGE_CURVE ( 'NONE', #38641, #20960, #9769, .T. ) ;
#33088 = ORIENTED_EDGE ( 'NONE', *, *, #8115, .F. ) ;
#33089 = CARTESIAN_POINT ( 'NONE',  ( -1.733526556417524622, 0.000000000000000000, 0.1851600754179555941 ) ) ;
#33090 = CARTESIAN_POINT ( 'NONE',  ( 1.461782879395302048, 1.205361022782829114E-17, -1.598346982901808211 ) ) ;
#33091 = ORIENTED_EDGE ( 'NONE', *, *, #44080, .F. ) ;
#33092 = ORIENTED_EDGE ( 'NONE', *, *, #46890, .T. ) ;
#33093 = CARTESIAN_POINT ( 'NONE',  ( 0.5455278134075212115, 3.346456692913386100, 0.9448818897637746295 ) ) ;
#33094 = CARTESIAN_POINT ( 'NONE',  ( 0.2727639067037610499, 0.000000000000000000, 2.362204724409437961 ) ) ;
#33095 = EDGE_LOOP ( 'NONE', ( #1015, #190, #38512, #20397 ) ) ;
#33096 = VERTEX_POINT ( 'NONE', #25508 ) ;
#33097 = CARTESIAN_POINT ( 'NONE',  ( 1.363819533518803251, 0.000000000000000000, -0.1574803149606304187 ) ) ;
#33098 = EDGE_CURVE ( 'NONE', #37445, #41115, #43354, .T. ) ;
#33099 = AXIS2_PLACEMENT_3D ( 'NONE', #28334, #44336, #20339 ) ;
#33100 = VERTEX_POINT ( 'NONE', #41267 ) ;
#33101 = VECTOR ( 'NONE', #39665, 39.37007874015748143 ) ;
#33102 = DIRECTION ( 'NONE',  ( 1.734723475976806848E-16, -0.000000000000000000, 1.000000000000000000 ) ) ;
#33103 = EDGE_CURVE ( 'NONE', #35993, #42801, #10021, .T. ) ;
#33104 = DIRECTION ( 'NONE',  ( -0.000000000000000000, 0.000000000000000000, 1.000000000000000000 ) ) ;
#33105 = VECTOR ( 'NONE', #4960, 39.37007874015748143 ) ;
#33106 = ADVANCED_FACE ( 'NONE', ( #19274 ), #23152, .F. ) ;
#33107 = EDGE_LOOP ( 'NONE', ( #50495, #20951, #44672, #2378 ) ) ;
#33108 = EDGE_LOOP ( 'NONE', ( #34617, #6721, #23983, #41442 ) ) ;
#33109 = VERTEX_POINT ( 'NONE', #11289 ) ;
#33110 = PLANE ( 'NONE',  #28801 ) ;
#33112 = ORIENTED_EDGE ( 'NONE', *, *, #41761, .F. ) ;
#33111 = ADVANCED_FACE ( 'NONE', ( #22403 ), #23401, .F. ) ;
#33113 = ORIENTED_EDGE ( 'NONE', *, *, #16531, .F. ) ;
#33114 = CARTESIAN_POINT ( 'NONE',  ( 0.4788131938641112528, 1.726726173772622941, 2.914091152102192162 ) ) ;
#33115 = CARTESIAN_POINT ( 'NONE',  ( 1.833433833923351353, 0.000000000000000000, -0.8267716535433055070 ) ) ;
#33116 = VECTOR ( 'NONE', #25539, 39.37007874015748143 ) ;
#33117 = CARTESIAN_POINT ( 'NONE',  ( 1.152568299495707826, 1.574803149606302854, 1.833124570921553120 ) ) ;
#33118 = AXIS2_PLACEMENT_3D ( 'NONE', #3539, #27016, #22903 ) ;
#33119 = ORIENTED_EDGE ( 'NONE', *, *, #47662, .T. ) ;
#33120 = CARTESIAN_POINT ( 'NONE',  ( 1.033334490728470723, 1.724452693827607908, -2.032317711754626277 ) ) ;
#33121 = CARTESIAN_POINT ( 'NONE',  ( 1.429001793727219249, 1.049866565067837820, -1.434352145109974996 ) ) ;
#33122 = LINE ( 'NONE', #5480, #8865 ) ;
#33123 = VERTEX_POINT ( 'NONE', #3034 ) ;
#33124 = PLANE ( 'NONE',  #33988 ) ;
#33125 = CARTESIAN_POINT ( 'NONE',  ( -0.8182917201112815953, 3.267716535433071279, 1.419509857074482553E-16 ) ) ;
#33126 = FACE_OUTER_BOUND ( 'NONE', #27451, .T. ) ;
#33127 = ORIENTED_EDGE ( 'NONE', *, *, #43700, .F. ) ;
#33128 = ORIENTED_EDGE ( 'NONE', *, *, #9181, .T. ) ;
#33129 = DIRECTION ( 'NONE',  ( -1.000000000000000000, 0.000000000000000000, 0.000000000000000000 ) ) ;
#33130 = CARTESIAN_POINT ( 'NONE',  ( 0.2727639067037604392, 0.000000000000000000, -0.9842519685039348154 ) ) ;
#33131 = LINE ( 'NONE', #49329, #27178 ) ;
#33132 = ORIENTED_EDGE ( 'NONE', *, *, #4614, .T. ) ;
#33133 = VERTEX_POINT ( 'NONE', #42770 ) ;
#33134 = DIRECTION ( 'NONE',  ( 0.000000000000000000, 0.000000000000000000, -1.000000000000000000 ) ) ;
#33135 = VERTEX_POINT ( 'NONE', #35038 ) ;
#33136 = LINE ( 'NONE', #4990, #36494 ) ;
#33137 = CARTESIAN_POINT ( 'NONE',  ( -2.867773316779185677, 1.574658946938755522, -0.7050287376752426560 ) ) ;
#33138 = VECTOR ( 'NONE', #32125, 39.37007874015748143 ) ;
#33139 = EDGE_CURVE ( 'NONE', #1125, #16455, #34283, .T. ) ;
#33140 = CARTESIAN_POINT ( 'NONE',  ( 1.363819533518803029, 3.346456692913386100, -1.732283464566923170 ) ) ;
#33141 = EDGE_CURVE ( 'NONE', #39828, #23227, #34535, .T. ) ;
#33142 = PLANE ( 'NONE',  #43376 ) ;
#33144 = FACE_OUTER_BOUND ( 'NONE', #21733, .T. ) ;
#33143 = VECTOR ( 'NONE', #16393, 39.37007874015748143 ) ;
#33145 = EDGE_LOOP ( 'NONE', ( #12980, #3998, #45513, #18211 ) ) ;
#33146 = EDGE_CURVE ( 'NONE', #26629, #4890, #38905, .T. ) ;
#33147 = CARTESIAN_POINT ( 'NONE',  ( 0.2727639067037604392, 0.000000000000000000, -1.614173228346451605 ) ) ;
#33148 = AXIS2_PLACEMENT_3D ( 'NONE', #24212, #31965, #15945 ) ;
#33149 = FACE_OUTER_BOUND ( 'NONE', #3671, .T. ) ;
#33150 = EDGE_CURVE ( 'NONE', #45728, #6369, #30147, .T. ) ;
#33151 = EDGE_LOOP ( 'NONE', ( #1926, #23301, #46302, #50527 ) ) ;
#33152 = AXIS2_PLACEMENT_3D ( 'NONE', #4495, #359, #39605 ) ;
#33153 = CARTESIAN_POINT ( 'NONE',  ( -1.712496953225537188, 3.346456692913386100, -0.1574803149606297248 ) ) ;
#33154 = DIRECTION ( 'NONE',  ( 2.214792131866782686E-16, 0.6427876096865404731, -0.7660444431189771253 ) ) ;
#33155 = DIRECTION ( 'NONE',  ( 0.000000000000000000, 0.000000000000000000, 1.000000000000000000 ) ) ;
#33156 = ORIENTED_EDGE ( 'NONE', *, *, #23913, .T. ) ;
#33157 = CARTESIAN_POINT ( 'NONE',  ( 0.8329809839909849689, 1.496921813388997435, -2.833254665166554442 ) ) ;
#33158 = LINE ( 'NONE', #14279, #45670 ) ;
#33159 = ORIENTED_EDGE ( 'NONE', *, *, #41453, .F. ) ;
#33160 = CARTESIAN_POINT ( 'NONE',  ( -2.158043018693463377, 1.574915981856324310, -0.1812028363557288968 ) ) ;
#33161 = DIRECTION ( 'NONE',  ( -0.000000000000000000, 1.000000000000000000, -0.000000000000000000 ) ) ;
#33163 = ORIENTED_EDGE ( 'NONE', *, *, #17885, .T. ) ;
#33162 = EDGE_CURVE ( 'NONE', #11634, #22597, #6443, .T. ) ;
#33164 = CARTESIAN_POINT ( 'NONE',  ( -1.909347346926324462, 0.000000000000000000, 1.102362204724404160 ) ) ;
#33165 = LINE ( 'NONE', #36773, #25133 ) ;
#33166 = EDGE_CURVE ( 'NONE', #16772, #19508, #49972, .T. ) ;
#33167 = CARTESIAN_POINT ( 'NONE',  ( 0.1968503937007878568, 0.000000000000000000, 0.9448818897637749625 ) ) ;
#33168 = FACE_OUTER_BOUND ( 'NONE', #47482, .T. ) ;
#33169 = CARTESIAN_POINT ( 'NONE',  ( -0.2430652128771645382, 1.574803149606302854, -2.151668812760861194 ) ) ;
#33170 = VERTEX_POINT ( 'NONE', #49718 ) ;
#33171 = EDGE_LOOP ( 'NONE', ( #48793, #5501, #23151, #7672 ) ) ;
#33172 = DIRECTION ( 'NONE',  ( 0.5407162030609374836, -0.6444004775717705469, -0.5407162030609374836 ) ) ;
#33173 = LINE ( 'NONE', #48856, #12255 ) ;
#33174 = EDGE_CURVE ( 'NONE', #46419, #46902, #46120, .T. ) ;
#33175 = ORIENTED_EDGE ( 'NONE', *, *, #15883, .F. ) ;
#33176 = PLANE ( 'NONE',  #25910 ) ;
#33177 = DIRECTION ( 'NONE',  ( 1.000000000000000000, -0.000000000000000000, 0.000000000000000000 ) ) ;
#33178 = CARTESIAN_POINT ( 'NONE',  ( -1.439733046521776139, 3.267716535433071279, 0.3149606299212578953 ) ) ;
#33179 = EDGE_CURVE ( 'NONE', #37754, #45470, #14397, .T. ) ;
#33180 = ORIENTED_EDGE ( 'NONE', *, *, #9595, .T. ) ;
#33181 = CONICAL_SURFACE ( 'NONE', #39750, 2.165354330708661568, 0.2617993877991570129 ) ;
#33182 = ORIENTED_EDGE ( 'NONE', *, *, #31810, .F. ) ;
#33183 = DIRECTION ( 'NONE',  ( -0.6427876096865403621, -0.7660444431189770143, 0.000000000000000000 ) ) ;
#33184 = DIRECTION ( 'NONE',  ( 0.6427876096865403621, -0.7660444431189770143, 1.858431260983764056E-16 ) ) ;
#33185 = CARTESIAN_POINT ( 'NONE',  ( -1.636583440222563635, 3.346456692913386100, 0.9448818897637749625 ) ) ;
#33186 = EDGE_LOOP ( 'NONE', ( #44285, #28765, #37369, #28620, #20621, #25486, #11144, #16326, #18364, #6910, #12993, #19827, #12954 ) ) ;
#33187 = CARTESIAN_POINT ( 'NONE',  ( -1.091055626815042201, 0.000000000000000000, 0.1181102362204705658 ) ) ;
#33188 = VECTOR ( 'NONE', #16066, 39.37007874015748143 ) ;
#33189 = FACE_BOUND ( 'NONE', #29727, .T. ) ;
#33190 = VERTEX_POINT ( 'NONE', #45866 ) ;
#33191 = LINE ( 'NONE', #8657, #22451 ) ;
#33192 = ORIENTED_EDGE ( 'NONE', *, *, #49291, .F. ) ;
#33193 = VECTOR ( 'NONE', #21872, 39.37007874015748143 ) ;
#33194 = ORIENTED_EDGE ( 'NONE', *, *, #16620, .T. ) ;
#33195 = FACE_OUTER_BOUND ( 'NONE', #2363, .T. ) ;
#33196 = VECTOR ( 'NONE', #16963, 39.37007874015748143 ) ;
#33197 = ORIENTED_EDGE ( 'NONE', *, *, #29630, .T. ) ;
#33198 = CARTESIAN_POINT ( 'NONE',  ( -0.8942052331142552601, 3.267716535433071279, 3.102397620449223960E-16 ) ) ;
#33199 = LINE ( 'NONE', #23440, #16321 ) ;
#33200 = EDGE_LOOP ( 'NONE', ( #19681, #1925, #17729, #17717 ) ) ;
#33201 = FACE_OUTER_BOUND ( 'NONE', #39899, .T. ) ;
#33202 = CARTESIAN_POINT ( 'NONE',  ( 2.339241080213586343, 1.205361022782829114E-17, 1.802537235681917815 ) ) ;
#33203 = CARTESIAN_POINT ( 'NONE',  ( -2.576863348864732117, 1.679095609600309347, 1.442554885838411849 ) ) ;
#33204 = CARTESIAN_POINT ( 'NONE',  ( 1.091055626815042645, 0.000000000000000000, -0.1968503937007883287 ) ) ;
#33205 = EDGE_CURVE ( 'NONE', #19810, #904, #42263, .T. ) ;
#33206 = DIRECTION ( 'NONE',  ( 1.000000000000000000, 0.000000000000000000, 0.000000000000000000 ) ) ;
#33207 = DIRECTION ( 'NONE',  ( 0.01601477604151182663, -0.9998717552508123996, 0.000000000000000000 ) ) ;
#33208 = ORIENTED_EDGE ( 'NONE', *, *, #28167, .F. ) ;
#33209 = EDGE_CURVE ( 'NONE', #9222, #16455, #30404, .T. ) ;
#33210 = PLANE ( 'NONE',  #3546 ) ;
#33211 = CARTESIAN_POINT ( 'NONE',  ( 0.000000000000000000, 5.905511811023623991, 0.000000000000000000 ) ) ;
#33212 = EDGE_CURVE ( 'NONE', #34644, #16311, #6905, .T. ) ;
#33213 = ORIENTED_EDGE ( 'NONE', *, *, #46005, .F. ) ;
#33214 = VECTOR ( 'NONE', #21176, 39.37007874015748143 ) ;
#33215 = DIRECTION ( 'NONE',  ( 0.000000000000000000, -1.000000000000000000, 0.000000000000000000 ) ) ;
#33216 = LINE ( 'NONE', #33476, #2207 ) ;
#33217 = VERTEX_POINT ( 'NONE', #7416 ) ;
#33218 = LINE ( 'NONE', #49163, #2370 ) ;
#33219 = EDGE_CURVE ( 'NONE', #4697, #48815, #46370, .T. ) ;
#33220 = LINE ( 'NONE', #18477, #13492 ) ;
#33221 = LINE ( 'NONE', #25967, #12004 ) ;
#33222 = VECTOR ( 'NONE', #36853, 39.37007874015748143 ) ;
#33223 = ORIENTED_EDGE ( 'NONE', *, *, #25731, .T. ) ;
#33224 = VECTOR ( 'NONE', #32262, 39.37007874015748143 ) ;
#33225 = DIRECTION ( 'NONE',  ( -0.000000000000000000, 0.000000000000000000, 1.000000000000000000 ) ) ;
#33226 = ORIENTED_EDGE ( 'NONE', *, *, #27123, .T. ) ;
#33227 = FACE_BOUND ( 'NONE', #49568, .T. ) ;
#33228 = CARTESIAN_POINT ( 'NONE',  ( -1.883550378546958282, 6.692913385826772199, -1.069467267250447495 ) ) ;
#33229 = CIRCLE ( 'NONE', #10953, 1.743387098533651480 ) ;
#33230 = VECTOR ( 'NONE', #9655, 39.37007874015748143 ) ;
#33231 = FACE_OUTER_BOUND ( 'NONE', #23042, .T. ) ;
#33232 = EDGE_CURVE ( 'NONE', #6075, #27292, #38407, .T. ) ;
#33233 = LINE ( 'NONE', #13345, #37538 ) ;
#33234 = ORIENTED_EDGE ( 'NONE', *, *, #5812, .T. ) ;
#33235 = ORIENTED_EDGE ( 'NONE', *, *, #23970, .F. ) ;
#33236 = LINE ( 'NONE', #8963, #48513 ) ;
#33237 = VERTEX_POINT ( 'NONE', #38661 ) ;
#33238 = EDGE_CURVE ( 'NONE', #22637, #22707, #34782, .T. ) ;
#33239 = CARTESIAN_POINT ( 'NONE',  ( 1.602753508900452317, 0.000000000000000000, 1.341098548255033496 ) ) ;
#33240 = ORIENTED_EDGE ( 'NONE', *, *, #43117, .T. ) ;
#33241 = CARTESIAN_POINT ( 'NONE',  ( 0.000000000000000000, 6.692913385826772199, 0.000000000000000000 ) ) ;
#33242 = EDGE_LOOP ( 'NONE', ( #30765, #4030, #863, #9599 ) ) ;
#33243 = CARTESIAN_POINT ( 'NONE',  ( -0.2727639067037602172, 3.346456692913386100, 1.102362204724404160 ) ) ;
#33244 = CARTESIAN_POINT ( 'NONE',  ( -1.833791099076586217, 1.574803149606302854, -1.151507526013721083 ) ) ;
#33245 = ORIENTED_EDGE ( 'NONE', *, *, #11674, .F. ) ;
#33246 = DIRECTION ( 'NONE',  ( 1.000000000000000000, 0.000000000000000000, -3.469446951953613696E-16 ) ) ;
#33247 = ORIENTED_EDGE ( 'NONE', *, *, #15716, .T. ) ;
#33248 = VERTEX_POINT ( 'NONE', #30909 ) ;
#33249 = ADVANCED_FACE ( 'NONE', ( #46619 ), #24697, .F. ) ;
#33250 = ORIENTED_EDGE ( 'NONE', *, *, #14094, .F. ) ;
#33251 = ORIENTED_EDGE ( 'NONE', *, *, #22834, .T. ) ;
#33252 = FACE_OUTER_BOUND ( 'NONE', #19322, .T. ) ;
#33253 = CIRCLE ( 'NONE', #29097, 1.850107469027523432 ) ;
#33254 = ORIENTED_EDGE ( 'NONE', *, *, #17112, .T. ) ;
#33255 = CARTESIAN_POINT ( 'NONE',  ( -0.6214413264104945434, 3.346456692913386100, -1.614173228346451605 ) ) ;
#33256 = ORIENTED_EDGE ( 'NONE', *, *, #36243, .T. ) ;
#33257 = LINE ( 'NONE', #49703, #22770 ) ;
#33258 = AXIS2_PLACEMENT_3D ( 'NONE', #42817, #15708, #23446 ) ;
#33259 = CIRCLE ( 'NONE', #1924, 2.164630168518208109 ) ;
#33260 = DIRECTION ( 'NONE',  ( -3.469446951953613696E-16, 0.000000000000000000, -1.000000000000000000 ) ) ;
#33261 = VERTEX_POINT ( 'NONE', #7916 ) ;
#33262 = DIRECTION ( 'NONE',  ( -0.000000000000000000, 1.000000000000000000, -0.000000000000000000 ) ) ;
#33263 = DIRECTION ( 'NONE',  ( 0.01601477604151182663, -0.9998717552508123996, 0.000000000000000000 ) ) ;
#33264 = VECTOR ( 'NONE', #32443, 39.37007874015748143 ) ;
#33265 = ORIENTED_EDGE ( 'NONE', *, *, #50747, .T. ) ;
#33266 = EDGE_CURVE ( 'NONE', #47436, #35629, #36059, .T. ) ;
#33267 = CARTESIAN_POINT ( 'NONE',  ( 0.1968503937007878568, 3.346456692913386100, 2.156388021673882438 ) ) ;
#33268 = CARTESIAN_POINT ( 'NONE',  ( -0.8942052331142552601, 3.346456692913386100, -1.907064071829739582 ) ) ;
#33269 = LINE ( 'NONE', #37397, #33446 ) ;
#33270 = DIRECTION ( 'NONE',  ( -0.000000000000000000, 1.000000000000000000, -0.000000000000000000 ) ) ;
#33271 = EDGE_CURVE ( 'NONE', #38725, #42469, #9553, .T. ) ;
#33272 = CARTESIAN_POINT ( 'NONE',  ( 0.8004649005966348874, 0.000000000000000000, -1.548759025234849762 ) ) ;
#33273 = EDGE_CURVE ( 'NONE', #10342, #11574, #4817, .T. ) ;
#33274 = ORIENTED_EDGE ( 'NONE', *, *, #37001, .F. ) ;
#33275 = CARTESIAN_POINT ( 'NONE',  ( -1.834323595590334977, 1.205361022782829114E-17, 1.151859023884900690 ) ) ;
#33276 = EDGE_CURVE ( 'NONE', #18135, #25893, #4299, .T. ) ;
#33277 = CARTESIAN_POINT ( 'NONE',  ( 1.015142113812069091, 3.267716535433071279, -2.047244094488181343 ) ) ;
#33278 = VERTEX_POINT ( 'NONE', #43526 ) ;
#33279 = PLANE ( 'NONE',  #6974 ) ;
#33280 = ORIENTED_EDGE ( 'NONE', *, *, #6405, .T. ) ;
#33281 = DIRECTION ( 'NONE',  ( 0.000000000000000000, 1.000000000000000000, 0.000000000000000000 ) ) ;
#33282 = DIRECTION ( 'NONE',  ( 1.000000000000000000, -0.000000000000000000, 0.000000000000000000 ) ) ;
#33283 = LINE ( 'NONE', #1264, #9727 ) ;
#33284 = DIRECTION ( 'NONE',  ( 9.964307797194585150E-17, -1.000000000000000000, 5.953396763000637613E-17 ) ) ;
#33285 = ADVANCED_FACE ( 'NONE', ( #39925 ), #35799, .F. ) ;
#33286 = LINE ( 'NONE', #17525, #50718 ) ;
#33287 = VERTEX_POINT ( 'NONE', #20560 ) ;
#33288 = FACE_OUTER_BOUND ( 'NONE', #7445, .T. ) ;
#33289 = VECTOR ( 'NONE', #49056, 39.37007874015748143 ) ;
#33290 = LINE ( 'NONE', #13154, #12184 ) ;
#33291 = DIRECTION ( 'NONE',  ( 0.000000000000000000, 0.000000000000000000, -1.000000000000000000 ) ) ;
#33292 = ORIENTED_EDGE ( 'NONE', *, *, #45620, .F. ) ;
#33293 = EDGE_CURVE ( 'NONE', #17266, #49145, #422, .T. ) ;
#33294 = CARTESIAN_POINT ( 'NONE',  ( 0.7423782071083084855, 3.346456692913386100, -1.574803149606293529 ) ) ;
#33295 = AXIS2_PLACEMENT_3D ( 'NONE', #26220, #22101, #49165 ) ;
#33296 = ORIENTED_EDGE ( 'NONE', *, *, #43979, .F. ) ;
#33297 = CONICAL_SURFACE ( 'NONE', #25874, 3.033577403570480779, 1.554780866114618743 ) ;
#33298 = VECTOR ( 'NONE', #20486, 39.37007874015748143 ) ;
#33299 = CARTESIAN_POINT ( 'NONE',  ( 0.8182917201112819283, 3.346456692913386100, 0.9055118110236164419 ) ) ;
#33300 = DIRECTION ( 'NONE',  ( -0.000000000000000000, 0.000000000000000000, 1.000000000000000000 ) ) ;
#33301 = EDGE_CURVE ( 'NONE', #36015, #13127, #16439, .T. ) ;
#33302 = DIRECTION ( 'NONE',  ( -0.1785568947986370392, 0.000000000000000000, 0.9839295885986295565 ) ) ;
#33303 = VECTOR ( 'NONE', #12749, 39.37007874015748143 ) ;
#33304 = CARTESIAN_POINT ( 'NONE',  ( 1.062992125984251413, 0.5905511811023621549, 1.062992125984251413 ) ) ;
#33305 = VERTEX_POINT ( 'NONE', #27526 ) ;
#33306 = EDGE_LOOP ( 'NONE', ( #25651, #7262, #41847, #45911 ) ) ;
#33307 = CARTESIAN_POINT ( 'NONE',  ( 0.000000000000000000, 3.267716535433071279, 1.417322834645662333 ) ) ;
#33308 = LINE ( 'NONE', #32540, #28136 ) ;
#33309 = FACE_BOUND ( 'NONE', #18759, .T. ) ;
#33310 = ORIENTED_EDGE ( 'NONE', *, *, #27811, .T. ) ;
#33311 = EDGE_CURVE ( 'NONE', #49369, #29685, #36317, .T. ) ;
#33312 = DIRECTION ( 'NONE',  ( 1.734723475976806848E-16, -0.000000000000000000, 1.000000000000000000 ) ) ;
#33313 = CARTESIAN_POINT ( 'NONE',  ( 0.4910466871075136464, 1.049866565067837820, -1.964251855984342265 ) ) ;
#33314 = EDGE_LOOP ( 'NONE', ( #10119, #43234, #1764, #23114 ) ) ;
#33315 = ORIENTED_EDGE ( 'NONE', *, *, #23074, .F. ) ;
#33316 = CARTESIAN_POINT ( 'NONE',  ( -1.363819533518803695, 3.267716535433071279, 2.365849761790806473E-16 ) ) ;
#33317 = DIRECTION ( 'NONE',  ( -2.582876339026340310E-17, -1.000000000000000000, 1.131632063491650798E-16 ) ) ;
#33318 = EDGE_CURVE ( 'NONE', #35927, #38936, #12306, .T. ) ;
#33319 = ORIENTED_EDGE ( 'NONE', *, *, #1309, .T. ) ;
#33320 = VERTEX_POINT ( 'NONE', #40188 ) ;
#33322 = EDGE_CURVE ( 'NONE', #50880, #30518, #28552, .T. ) ;
#33321 = EDGE_LOOP ( 'NONE', ( #37878, #27676, #8377, #27483 ) ) ;
#33323 = PLANE ( 'NONE',  #21080 ) ;
#33324 = DIRECTION ( 'NONE',  ( -1.000000000000000000, 0.000000000000000000, -0.000000000000000000 ) ) ;
#33325 = DIRECTION ( 'NONE',  ( 1.734723475976806848E-16, 0.000000000000000000, 1.000000000000000000 ) ) ;
#33326 = CARTESIAN_POINT ( 'NONE',  ( 0.08139965876239094178, 1.610780518492231694, 0.000000000000000000 ) ) ;
#33327 = VERTEX_POINT ( 'NONE', #50973 ) ;
#33328 = VERTEX_POINT ( 'NONE', #12556 ) ;
#33329 = VECTOR ( 'NONE', #6441, 39.37007874015748143 ) ;
#33330 = LINE ( 'NONE', #5698, #19995 ) ;
#33331 = DIRECTION ( 'NONE',  ( 1.000000000000000000, 0.000000000000000000, -3.469446951953613696E-16 ) ) ;
#33332 = AXIS2_PLACEMENT_3D ( 'NONE', #48248, #17564, #49011 ) ;
#33333 = DIRECTION ( 'NONE',  ( 1.734723475976806848E-16, 0.000000000000000000, 1.000000000000000000 ) ) ;
#33334 = AXIS2_PLACEMENT_3D ( 'NONE', #49227, #10785, #30417 ) ;
#33335 = DIRECTION ( 'NONE',  ( -0.000000000000000000, 1.000000000000000000, -0.000000000000000000 ) ) ;
#33336 = VECTOR ( 'NONE', #28108, 39.37007874015748143 ) ;
#33337 = DIRECTION ( 'NONE',  ( -0.000000000000000000, 1.000000000000000000, -0.000000000000000000 ) ) ;
#33338 = EDGE_CURVE ( 'NONE', #28752, #2720, #43778, .T. ) ;
#33339 = VECTOR ( 'NONE', #28930, 39.37007874015748143 ) ;
#33340 = CARTESIAN_POINT ( 'NONE',  ( 1.363819533518803029, 3.346456692913386100, -1.614173228346452715 ) ) ;
#33341 = ADVANCED_FACE ( 'NONE', ( #24182 ), #20297, .F. ) ;
#33342 = EDGE_CURVE ( 'NONE', #33109, #28267, #2783, .T. ) ;
#33343 = PLANE ( 'NONE',  #45635 ) ;
#33344 = VECTOR ( 'NONE', #49841, 39.37007874015748143 ) ;
#33345 = EDGE_LOOP ( 'NONE', ( #47748, #46035, #12701, #31205 ) ) ;
#33346 = CARTESIAN_POINT ( 'NONE',  ( -1.363819533518803473, 3.346456692913386100, -1.732283464566922726 ) ) ;
#33347 = CARTESIAN_POINT ( 'NONE',  ( -0.5455278134075208785, 3.346456692913386100, 1.062992125984246083 ) ) ;
#33348 = ORIENTED_EDGE ( 'NONE', *, *, #25745, .T. ) ;
#33349 = EDGE_LOOP ( 'NONE', ( #29988, #32858, #49694, #11010 ) ) ;
#33350 = CARTESIAN_POINT ( 'NONE',  ( -1.636583440222564301, 3.346456692913386100, 1.574803149606291530 ) ) ;
#33351 = CARTESIAN_POINT ( 'NONE',  ( -2.100227814008681637, 1.559371130916006543, -2.076109931251943319 ) ) ;
#33352 = VERTEX_POINT ( 'NONE', #39411 ) ;
#33353 = VERTEX_POINT ( 'NONE', #32450 ) ;
#33354 = CARTESIAN_POINT ( 'NONE',  ( 2.012389709219288836, 1.049866565067838264, 0.2229346560889621798 ) ) ;
#33355 = VERTEX_POINT ( 'NONE', #8939 ) ;
#33356 = PLANE ( 'NONE',  #40874 ) ;
#33357 = LINE ( 'NONE', #13728, #15660 ) ;
#33358 = EDGE_CURVE ( 'NONE', #17616, #1486, #43266, .T. ) ;
#33359 = ORIENTED_EDGE ( 'NONE', *, *, #24391, .F. ) ;
#33360 = AXIS2_PLACEMENT_3D ( 'NONE', #18638, #10881, #50079 ) ;
#33361 = ORIENTED_EDGE ( 'NONE', *, *, #13398, .F. ) ;
#33362 = CARTESIAN_POINT ( 'NONE',  ( 0.8182917201112819283, 3.346456692913386100, -0.3543307086614175816 ) ) ;
#33363 = VECTOR ( 'NONE', #3976, 39.37007874015748143 ) ;
#33364 = VERTEX_POINT ( 'NONE', #11785 ) ;
#33365 = VERTEX_POINT ( 'NONE', #19780 ) ;
#33366 = VECTOR ( 'NONE', #22915, 39.37007874015748143 ) ;
#33367 = DIRECTION ( 'NONE',  ( 1.000000000000000000, 0.000000000000000000, 0.000000000000000000 ) ) ;
#33368 = DIRECTION ( 'NONE',  ( 0.000000000000000000, 1.000000000000000000, 0.000000000000000000 ) ) ;
#33369 = DIRECTION ( 'NONE',  ( -0.000000000000000000, 1.000000000000000000, -0.000000000000000000 ) ) ;
#33370 = EDGE_CURVE ( 'NONE', #5323, #38936, #32712, .T. ) ;
#33371 = VECTOR ( 'NONE', #48718, 39.37007874015748143 ) ;
#33372 = VECTOR ( 'NONE', #36321, 39.37007874015748143 ) ;
#33373 = VERTEX_POINT ( 'NONE', #5579 ) ;
#33374 = EDGE_CURVE ( 'NONE', #3361, #40300, #13836, .T. ) ;
#33375 = PLANE ( 'NONE',  #17252 ) ;
#33376 = DIRECTION ( 'NONE',  ( -0.000000000000000000, 1.000000000000000000, -0.000000000000000000 ) ) ;
#33377 = DIRECTION ( 'NONE',  ( 1.000000000000000000, 0.000000000000000000, -3.469446951953613696E-16 ) ) ;
#33378 = EDGE_CURVE ( 'NONE', #23218, #37644, #9711, .T. ) ;
#33379 = ORIENTED_EDGE ( 'NONE', *, *, #37460, .F. ) ;
#33380 = FACE_OUTER_BOUND ( 'NONE', #27239, .T. ) ;
#33381 = FACE_OUTER_BOUND ( 'NONE', #47847, .T. ) ;
#33382 = VECTOR ( 'NONE', #23344, 39.37007874015748143 ) ;
#33383 = LINE ( 'NONE', #17367, #1026 ) ;
#33384 = ORIENTED_EDGE ( 'NONE', *, *, #9596, .F. ) ;
#33385 = VERTEX_POINT ( 'NONE', #5320 ) ;
#33386 =( NAMED_UNIT ( * ) PLANE_ANGLE_UNIT ( ) SI_UNIT ( $, .RADIAN. ) );
#33387 = CARTESIAN_POINT ( 'NONE',  ( 0.8182917201112819283, 3.346456692913386100, 0.1574803149606286423 ) ) ;
#33388 = CARTESIAN_POINT ( 'NONE',  ( 0.2727639067037602172, 3.267716535433071279, -2.148105963102950877 ) ) ;
#33389 = ADVANCED_FACE ( 'NONE', ( #37083 ), #49412, .F. ) ;
#33390 = DIRECTION ( 'NONE',  ( -0.000000000000000000, 1.000000000000000000, -0.000000000000000000 ) ) ;
#33391 = B_SPLINE_CURVE_WITH_KNOTS ( 'NONE', 3,
 ( #38384, #21614, #37374, #45332 ),
 .UNSPECIFIED., .F., .F.,
 ( 4, 4 ),
 ( 2.032896518363797548E-07, 0.002500497254889573386 ),
 .UNSPECIFIED. ) ;
#33392 = ORIENTED_EDGE ( 'NONE', *, *, #29490, .F. ) ;
#33393 = VERTEX_POINT ( 'NONE', #40955 ) ;
#33394 = CARTESIAN_POINT ( 'NONE',  ( 0.000000000000000000, 1.574803149606302854, 0.000000000000000000 ) ) ;
#33395 = ORIENTED_EDGE ( 'NONE', *, *, #29860, .F. ) ;
#33396 = DIRECTION ( 'NONE',  ( 1.000000000000000000, 0.000000000000000000, 0.000000000000000000 ) ) ;
#33397 = CARTESIAN_POINT ( 'NONE',  ( -0.3381173457103609503, 6.692913385826772199, 2.138793126519845877 ) ) ;
#33398 = ADVANCED_FACE ( 'NONE', ( #33727 ), #41211, .F. ) ;
#33399 = EDGE_CURVE ( 'NONE', #22612, #3488, #17710, .T. ) ;
#33400 = EDGE_CURVE ( 'NONE', #20580, #39173, #17451, .T. ) ;
#33401 = CARTESIAN_POINT ( 'NONE',  ( 0.4001787029124908024, 1.205361022782829114E-17, 1.929553426015793605 ) ) ;
#33402 = CARTESIAN_POINT ( 'NONE',  ( 0.1525302393087137887, 1.710345001767278994, -2.243756654240526505 ) ) ;
#33403 = PLANE ( 'NONE',  #22930 ) ;
#33404 = VERTEX_POINT ( 'NONE', #33475 ) ;
#33405 = VECTOR ( 'NONE', #17573, 39.37007874015748143 ) ;
#33406 = DIRECTION ( 'NONE',  ( -3.469446951953613696E-16, 0.000000000000000000, -1.000000000000000000 ) ) ;
#33407 = DIRECTION ( 'NONE',  ( -1.000000000000000000, 0.000000000000000000, 1.734723475976806848E-16 ) ) ;
#33408 = VECTOR ( 'NONE', #9315, 39.37007874015748143 ) ;
#33409 = CARTESIAN_POINT ( 'NONE',  ( -1.232995795418201590, 5.905511811023623991, 1.780798594093551568 ) ) ;
#33410 = AXIS2_PLACEMENT_3D ( 'NONE', #8636, #40402, #636 ) ;
#33411 = ORIENTED_EDGE ( 'NONE', *, *, #32436, .T. ) ;
#33412 = CARTESIAN_POINT ( 'NONE',  ( 2.100227814008712723, 5.905511811023623991, -2.076109931251913565 ) ) ;
#33413 = CARTESIAN_POINT ( 'NONE',  ( -1.091055626815042201, 3.346456692913386100, 0.6299212598425164567 ) ) ;
#33414 = CARTESIAN_POINT ( 'NONE',  ( 0.5455278134075216556, 0.000000000000000000, 1.692913385826762873 ) ) ;
#33415 = EDGE_LOOP ( 'NONE', ( #25036, #11902, #20698, #41665 ) ) ;
#33416 = DIRECTION ( 'NONE',  ( 0.000000000000000000, 0.000000000000000000, -1.000000000000000000 ) ) ;
#33417 = DIRECTION ( 'NONE',  ( -0.000000000000000000, -1.000000000000000000, -0.000000000000000000 ) ) ;
#33418 = VECTOR ( 'NONE', #47476, 39.37007874015748143 ) ;
#33419 = ORIENTED_EDGE ( 'NONE', *, *, #50223, .T. ) ;
#33420 = LINE ( 'NONE', #32911, #27961 ) ;
#33421 = LINE ( 'NONE', #9910, #37354 ) ;
#33422 = ORIENTED_EDGE ( 'NONE', *, *, #10803, .T. ) ;
#33423 = CARTESIAN_POINT ( 'NONE',  ( -1.070574558570679624, 1.033102224082122600, -2.336494445557213862 ) ) ;
#33424 = LINE ( 'NONE', #25150, #34216 ) ;
#33425 = DIRECTION ( 'NONE',  ( 0.000000000000000000, 0.000000000000000000, -1.000000000000000000 ) ) ;
#33426 = PLANE ( 'NONE',  #26025 ) ;
#33427 = DIRECTION ( 'NONE',  ( 0.000000000000000000, 1.000000000000000000, 0.000000000000000000 ) ) ;
#33428 = ORIENTED_EDGE ( 'NONE', *, *, #7376, .F. ) ;
#33429 = VERTEX_POINT ( 'NONE', #14088 ) ;
#33430 = PLANE ( 'NONE',  #46299 ) ;
#33431 = DIRECTION ( 'NONE',  ( -1.000000000000000000, 0.000000000000000000, -0.000000000000000000 ) ) ;
#33432 = ORIENTED_EDGE ( 'NONE', *, *, #23139, .F. ) ;
#33433 = DIRECTION ( 'NONE',  ( 1.734723475976806848E-16, -0.000000000000000000, 1.000000000000000000 ) ) ;
#33434 = DIRECTION ( 'NONE',  ( 0.000000000000000000, 1.000000000000000000, 0.000000000000000000 ) ) ;
#33435 = DIRECTION ( 'NONE',  ( 1.734723475976806848E-16, 0.000000000000000000, 1.000000000000000000 ) ) ;
#33436 = VERTEX_POINT ( 'NONE', #21331 ) ;
#33437 = ORIENTED_EDGE ( 'NONE', *, *, #32205, .F. ) ;
#33438 = ADVANCED_FACE ( 'NONE', ( #21583 ), #25447, .T. ) ;
#33439 = DIRECTION ( 'NONE',  ( -0.9998717552508122886, -0.01601477604151180928, 0.000000000000000000 ) ) ;
#33440 = DIRECTION ( 'NONE',  ( -3.469446951953613696E-16, 0.000000000000000000, -1.000000000000000000 ) ) ;
#33441 = CARTESIAN_POINT ( 'NONE',  ( 1.287906020515829919, 3.346456692913386100, -1.259842519685035134 ) ) ;
#33442 = VERTEX_POINT ( 'NONE', #29322 ) ;
#33443 = CARTESIAN_POINT ( 'NONE',  ( -2.139020239325885253, 1.673641627049041514, 0.3394120305351381872 ) ) ;
#33444 = EDGE_CURVE ( 'NONE', #38287, #24025, #25962, .T. ) ;
#33445 = DIRECTION ( 'NONE',  ( 0.000000000000000000, -1.000000000000000000, 0.000000000000000000 ) ) ;
#33446 = VECTOR ( 'NONE', #29382, 39.37007874015748143 ) ;
#33447 = ORIENTED_EDGE ( 'NONE', *, *, #17112, .F. ) ;
#33448 = CIRCLE ( 'NONE', #16096, 1.743387098533651480 ) ;
#33449 = CARTESIAN_POINT ( 'NONE',  ( 0.5433756366131596849, 1.629269058362078804, 2.902374796143934343 ) ) ;
#33450 = CIRCLE ( 'NONE', #49035, 2.165354330708661568 ) ;
#33451 = ORIENTED_EDGE ( 'NONE', *, *, #32570, .F. ) ;
#33452 = ORIENTED_EDGE ( 'NONE', *, *, #9235, .F. ) ;
#33453 = CARTESIAN_POINT ( 'NONE',  ( -0.07591351300297277671, 0.000000000000000000, 1.732283464566921172 ) ) ;
#33454 = CARTESIAN_POINT ( 'NONE',  ( 2.889674983507178219, 5.118110236220475784, -0.6090712660037604920 ) ) ;
#33455 = AXIS2_PLACEMENT_3D ( 'NONE', #44941, #33611, #2100 ) ;
#33456 = ORIENTED_EDGE ( 'NONE', *, *, #14637, .T. ) ;
#33457 = CARTESIAN_POINT ( 'NONE',  ( -0.6214413264104945434, 3.267716535433071279, -1.614173228346451605 ) ) ;
#33458 = CARTESIAN_POINT ( 'NONE',  ( 2.600183657057280051, 0.000000000000000000, 1.399218491554161892 ) ) ;
#33459 = ORIENTED_EDGE ( 'NONE', *, *, #40902, .T. ) ;
#33460 = AXIS2_PLACEMENT_3D ( 'NONE', #32659, #47580, #28760 ) ;
#33461 = EDGE_CURVE ( 'NONE', #32285, #48286, #13079, .T. ) ;
#33462 = CARTESIAN_POINT ( 'NONE',  ( 0.1067246931122726866, 0.02962905676920215767, 0.000000000000000000 ) ) ;
#33463 = LINE ( 'NONE', #33718, #2867 ) ;
#33464 = EDGE_CURVE ( 'NONE', #39618, #24556, #5068, .T. ) ;
#33465 = DIRECTION ( 'NONE',  ( 0.000000000000000000, 0.000000000000000000, -1.000000000000000000 ) ) ;
#33466 = B_SPLINE_CURVE_WITH_KNOTS ( 'NONE', 3,
 ( #49009, #13436, #41561, #18076 ),
 .UNSPECIFIED., .F., .F.,
 ( 4, 4 ),
 ( 2.174732542326846088E-07, 0.002500292828914785648 ),
 .UNSPECIFIED. ) ;
#33467 = ADVANCED_FACE ( 'NONE', ( #44549 ), #45551, .F. ) ;
#33468 = DIRECTION ( 'NONE',  ( -0.000000000000000000, 1.000000000000000000, -0.000000000000000000 ) ) ;
#33469 = LINE ( 'NONE', #21326, #13833 ) ;
#33470 = VERTEX_POINT ( 'NONE', #40696 ) ;
#33471 = DIRECTION ( 'NONE',  ( 1.000000000000000000, 0.000000000000000000, -3.469446951953613696E-16 ) ) ;
#33472 = ADVANCED_FACE ( 'NONE', ( #2220 ), #32969, .F. ) ;
#33473 = CARTESIAN_POINT ( 'NONE',  ( 1.560669927219591413, 0.000000000000000000, 1.732283464566921172 ) ) ;
#33474 = VERTEX_POINT ( 'NONE', #1448 ) ;
#33475 = CARTESIAN_POINT ( 'NONE',  ( 0.5455278134075212115, 3.346456692913386100, -1.259842519685035134 ) ) ;
#33476 = CARTESIAN_POINT ( 'NONE',  ( 0.1968503937007878568, 3.346456692913386100, 1.259842519685033357 ) ) ;
#33477 = VERTEX_POINT ( 'NONE', #17202 ) ;
#33478 = CARTESIAN_POINT ( 'NONE',  ( 1.015142113812069313, 3.346456692913386100, -0.4724409448818889246 ) ) ;
#33479 = CARTESIAN_POINT ( 'NONE',  ( -1.874262219842892208, 0.5253178361172772259, 1.064469095918958219 ) ) ;
#33480 = CARTESIAN_POINT ( 'NONE',  ( 1.015142113812069979, 3.267716535433071279, 2.047244094488179567 ) ) ;
#33481 = AXIS2_PLACEMENT_3D ( 'NONE', #46415, #18830, #14704 ) ;
#33482 = ORIENTED_EDGE ( 'NONE', *, *, #2724, .T. ) ;
#33483 = CARTESIAN_POINT ( 'NONE',  ( 0.000000000000000000, 3.267716535433071279, 0.000000000000000000 ) ) ;
#33484 = EDGE_LOOP ( 'NONE', ( #22170, #32349, #7462, #31695 ) ) ;
#33485 = FACE_BOUND ( 'NONE', #23009, .T. ) ;
#33486 = VECTOR ( 'NONE', #4641, 39.37007874015748143 ) ;
#33487 = DIRECTION ( 'NONE',  ( -1.000000000000000000, 0.000000000000000000, 0.000000000000000000 ) ) ;
#33488 = DIRECTION ( 'NONE',  ( 1.000000000000000000, 0.000000000000000000, 0.000000000000000000 ) ) ;
#33489 = CARTESIAN_POINT ( 'NONE',  ( -3.927031490892378253E-16, 3.346456692913386100, -2.204724409448811429 ) ) ;
#33490 = AXIS2_PLACEMENT_3D ( 'NONE', #39504, #20389, #40277 ) ;
#33491 = VECTOR ( 'NONE', #34677, 39.37007874015748143 ) ;
#33492 = ORIENTED_EDGE ( 'NONE', *, *, #41032, .F. ) ;
#33493 = VERTEX_POINT ( 'NONE', #48644 ) ;
#33494 = CARTESIAN_POINT ( 'NONE',  ( 1.083598637574782142, 1.637691314537677023, 2.747180975113346246 ) ) ;
#33495 = ORIENTED_EDGE ( 'NONE', *, *, #42108, .F. ) ;
#33496 = FACE_OUTER_BOUND ( 'NONE', #37472, .T. ) ;
#33497 = ORIENTED_EDGE ( 'NONE', *, *, #4544, .F. ) ;
#33498 = DIRECTION ( 'NONE',  ( -0.000000000000000000, 1.000000000000000000, -0.000000000000000000 ) ) ;
#33499 = ORIENTED_EDGE ( 'NONE', *, *, #8003, .F. ) ;
#33500 = FACE_OUTER_BOUND ( 'NONE', #35323, .T. ) ;
#33501 = LINE ( 'NONE', #45837, #42944 ) ;
#33502 = EDGE_CURVE ( 'NONE', #20098, #50692, #23614, .T. ) ;
#33503 = ORIENTED_EDGE ( 'NONE', *, *, #1965, .F. ) ;
#33504 = ADVANCED_FACE ( 'NONE', ( #13330 ), #18216, .F. ) ;
#33505 = CARTESIAN_POINT ( 'NONE',  ( -1.909347346926324906, 3.346456692913386100, -1.102362204724405492 ) ) ;
#33506 = ORIENTED_EDGE ( 'NONE', *, *, #2852, .F. ) ;
#33507 = ORIENTED_EDGE ( 'NONE', *, *, #21479, .T. ) ;
#33508 = EDGE_CURVE ( 'NONE', #6857, #26498, #200, .T. ) ;
#33509 = VECTOR ( 'NONE', #13511, 39.37007874015748143 ) ;
#33510 = ORIENTED_EDGE ( 'NONE', *, *, #4043, .F. ) ;
#33511 = VERTEX_POINT ( 'NONE', #26461 ) ;
#33512 = DIRECTION ( 'NONE',  ( -0.000000000000000000, 1.000000000000000000, -0.000000000000000000 ) ) ;
#33513 = CIRCLE ( 'NONE', #43421, 1.181102362204723200 ) ;
#33514 = CIRCLE ( 'NONE', #7910, 2.165354330708661568 ) ;
#33515 = ORIENTED_EDGE ( 'NONE', *, *, #5516, .F. ) ;
#33516 = DIRECTION ( 'NONE',  ( 0.000000000000000000, 0.6427876096865404731, -0.7660444431189771253 ) ) ;
#33517 = AXIS2_PLACEMENT_3D ( 'NONE', #35694, #32090, #31830 ) ;
#33518 = DIRECTION ( 'NONE',  ( 0.000000000000000000, 0.000000000000000000, -1.000000000000000000 ) ) ;
#33519 = EDGE_CURVE ( 'NONE', #50364, #5669, #10725, .T. ) ;
#33520 = CIRCLE ( 'NONE', #46623, 2.165354330708661568 ) ;
#33521 = DIRECTION ( 'NONE',  ( 1.000000000000000000, 0.000000000000000000, 0.000000000000000000 ) ) ;
#33522 = ORIENTED_EDGE ( 'NONE', *, *, #21574, .F. ) ;
#33523 = CIRCLE ( 'NONE', #6320, 2.244934639244525076 ) ;
#33524 = CARTESIAN_POINT ( 'NONE',  ( 1.129748414438405124, 1.627571742414081202, 1.986830176535870907 ) ) ;
#33525 = DIRECTION ( 'NONE',  ( -0.9998717552508122886, -0.01601477604151185785, 0.000000000000000000 ) ) ;
#33526 = EDGE_LOOP ( 'NONE', ( #45751, #48816, #50149, #12921 ) ) ;
#33527 = CARTESIAN_POINT ( 'NONE',  ( 2.951990591674675368, 0.000000000000000000, -0.08331184815398383348 ) ) ;
#33528 = DIRECTION ( 'NONE',  ( -0.000000000000000000, 1.000000000000000000, -0.000000000000000000 ) ) ;
#33529 = EDGE_CURVE ( 'NONE', #6756, #3555, #2718, .T. ) ;
#33530 = CARTESIAN_POINT ( 'NONE',  ( -1.091055626815042201, 3.346456692913386100, 0.6299212598425164567 ) ) ;
#33531 = DIRECTION ( 'NONE',  ( 1.734723475976806848E-16, -0.000000000000000000, 1.000000000000000000 ) ) ;
#33532 = CARTESIAN_POINT ( 'NONE',  ( 0.7229485578905374688, 0.02618475911999341987, 1.786232274300230571 ) ) ;
#33533 = CARTESIAN_POINT ( 'NONE',  ( 3.927031490892378253E-16, 3.267716535433071279, 0.7480314960629874665 ) ) ;
#33534 = ORIENTED_EDGE ( 'NONE', *, *, #35642, .T. ) ;
#33535 = DIRECTION ( 'NONE',  ( 0.000000000000000000, 1.000000000000000000, 0.000000000000000000 ) ) ;
#33536 = CARTESIAN_POINT ( 'NONE',  ( -1.712496953225537633, 0.000000000000000000, -1.102362204724405492 ) ) ;
#33537 = VERTEX_POINT ( 'NONE', #6848 ) ;
#33538 = LINE ( 'NONE', #40760, #30045 ) ;
#33539 = ORIENTED_EDGE ( 'NONE', *, *, #10298, .F. ) ;
#33540 = EDGE_CURVE ( 'NONE', #31998, #24393, #46313, .T. ) ;
#33541 = CARTESIAN_POINT ( 'NONE',  ( -2.298329623281018641, 1.584999146155742444, 1.853838580031352823 ) ) ;
#33542 = CARTESIAN_POINT ( 'NONE',  ( -0.4910466871652391374, 1.049866565877818347, -1.964251856193615531 ) ) ;
#33543 = CARTESIAN_POINT ( 'NONE',  ( -1.955085917952581909, 1.590347576141469377, 2.212843326005696554 ) ) ;
#33544 = DIRECTION ( 'NONE',  ( -1.000000000000000000, 0.000000000000000000, 1.734723475976806848E-16 ) ) ;
#33545 = CARTESIAN_POINT ( 'NONE',  ( 1.833433833923350686, 3.267716535433071279, -6.361001426713997494E-16 ) ) ;
#33546 = ORIENTED_EDGE ( 'NONE', *, *, #2852, .T. ) ;
#33547 = VECTOR ( 'NONE', #31795, 39.37007874015748143 ) ;
#33548 = DIRECTION ( 'NONE',  ( -1.000000000000000000, 0.000000000000000000, 0.000000000000000000 ) ) ;
#33549 = VECTOR ( 'NONE', #17502, 39.37007874015748143 ) ;
#33550 = ORIENTED_EDGE ( 'NONE', *, *, #25132, .T. ) ;
#33551 = CARTESIAN_POINT ( 'NONE',  ( -0.2727639067037607723, 0.000000000000000000, 0.1574803149606283648 ) ) ;
#33552 = VECTOR ( 'NONE', #49648, 39.37007874015748854 ) ;
#33553 = ORIENTED_EDGE ( 'NONE', *, *, #11322, .F. ) ;
#33554 = LINE ( 'NONE', #18297, #13936 ) ;
#33555 = LINE ( 'NONE', #8827, #12019 ) ;
#33556 = VERTEX_POINT ( 'NONE', #11481 ) ;
#33557 = CARTESIAN_POINT ( 'NONE',  ( -1.299212598425205423, 3.346456692913386100, -1.732283464566922726 ) ) ;
#33558 = CIRCLE ( 'NONE', #21976, 2.244934639244525076 ) ;
#33559 = CARTESIAN_POINT ( 'NONE',  ( 2.034508859078114629, 0.01953464615435679050, -0.4138851785833215224 ) ) ;
#33560 = VECTOR ( 'NONE', #17673, 39.37007874015748143 ) ;
#33561 = LINE ( 'NONE', #29675, #48585 ) ;
#33562 = VERTEX_POINT ( 'NONE', #18473 ) ;
#33564 = ORIENTED_EDGE ( 'NONE', *, *, #50899, .T. ) ;
#33563 = EDGE_CURVE ( 'NONE', #10447, #49658, #7104, .T. ) ;
#33565 = CARTESIAN_POINT ( 'NONE',  ( 0.08139965876239094178, 1.610780518492231694, 0.000000000000000000 ) ) ;
#33566 = FACE_BOUND ( 'NONE', #46039, .T. ) ;
#33567 = ORIENTED_EDGE ( 'NONE', *, *, #50057, .F. ) ;
#33568 = EDGE_CURVE ( 'NONE', #24413, #1162, #31104, .T. ) ;
#33569 = DIRECTION ( 'NONE',  ( 0.7071067811865483499, 1.579007132194770110E-15, -0.7071067811865466846 ) ) ;
#33570 = DIRECTION ( 'NONE',  ( -1.000000000000000000, 0.000000000000000000, 0.000000000000000000 ) ) ;
#33571 = ADVANCED_FACE ( 'NONE', ( #46561 ), #50410, .F. ) ;
#33573 = ORIENTED_EDGE ( 'NONE', *, *, #49982, .T. ) ;
#33572 = EDGE_CURVE ( 'NONE', #11612, #45138, #22595, .T. ) ;
#33574 = ORIENTED_EDGE ( 'NONE', *, *, #22909, .T. ) ;
#33575 = CARTESIAN_POINT ( 'NONE',  ( 0.000000000000000000, 3.267716535433071279, -0.3543307086614178592 ) ) ;
#33576 = CARTESIAN_POINT ( 'NONE',  ( -1.166969139818015977, 0.000000000000000000, -1.417322834645664109 ) ) ;
#33577 = EDGE_LOOP ( 'NONE', ( #49642, #43570, #31517, #36778 ) ) ;
#33578 = EDGE_LOOP ( 'NONE', ( #14825, #9526, #12258, #32377 ) ) ;
#33579 = ORIENTED_EDGE ( 'NONE', *, *, #30566, .T. ) ;
#33580 = DIRECTION ( 'NONE',  ( -0.000000000000000000, 1.000000000000000000, -0.000000000000000000 ) ) ;
#33581 = DIRECTION ( 'NONE',  ( -2.309260482754916270E-14, 0.000000000000000000, 1.000000000000000000 ) ) ;
#33582 = EDGE_CURVE ( 'NONE', #2713, #41904, #3220, .T. ) ;
#33584 = CARTESIAN_POINT ( 'NONE',  ( -2.623503965249869729, 1.569838463031876685, 1.355882097269834885 ) ) ;
#33583 = CONICAL_SURFACE ( 'NONE', #17902, 2.165354330708661568, 0.2617993877991570129 ) ;
#33585 = PLANE ( 'NONE',  #7403 ) ;
#33586 = VERTEX_POINT ( 'NONE', #10471 ) ;
#33587 = ORIENTED_EDGE ( 'NONE', *, *, #18461, .F. ) ;
#33589 = AXIS2_PLACEMENT_3D ( 'NONE', #32703, #24429, #20020 ) ;
#33588 = DIRECTION ( 'NONE',  ( 0.01601477604151182663, -0.9998717552508123996, 0.000000000000000000 ) ) ;
#33590 = LINE ( 'NONE', #2583, #33719 ) ;
#33591 = CARTESIAN_POINT ( 'NONE',  ( -0.5455278134075208785, 0.000000000000000000, 1.692913385826762873 ) ) ;
#33592 = ADVANCED_FACE ( 'NONE', ( #14597 ), #2976, .F. ) ;
#33593 = PLANE ( 'NONE',  #49000 ) ;
#33594 = DIRECTION ( 'NONE',  ( -0.9998717552508122886, -0.01601477604151180928, 0.000000000000000000 ) ) ;
#33595 = CARTESIAN_POINT ( 'NONE',  ( 1.979793062125284830, 1.470624965921384364, 2.191257344206569257 ) ) ;
#33596 = EDGE_CURVE ( 'NONE', #48779, #43306, #41965, .T. ) ;
#33597 = CARTESIAN_POINT ( 'NONE',  ( -1.166969139818015977, 3.346456692913386100, -1.753476375576570323 ) ) ;
#33598 = ORIENTED_EDGE ( 'NONE', *, *, #27176, .T. ) ;
#33599 = PLANE ( 'NONE',  #40739 ) ;
#33600 = DIRECTION ( 'NONE',  ( -0.01601477604151182663, 0.9998717552508123996, -0.000000000000000000 ) ) ;
#33601 = VECTOR ( 'NONE', #39979, 39.37007874015748143 ) ;
#33602 = ORIENTED_EDGE ( 'NONE', *, *, #15352, .F. ) ;
#33603 = EDGE_CURVE ( 'NONE', #24456, #15064, #18970, .T. ) ;
#33604 = ORIENTED_EDGE ( 'NONE', *, *, #32007, .F. ) ;
#33605 = FACE_OUTER_BOUND ( 'NONE', #28632, .T. ) ;
#33606 = VERTEX_POINT ( 'NONE', #46064 ) ;
#33607 = ADVANCED_FACE ( 'NONE', ( #38352 ), #18727, .F. ) ;
#33608 = ORIENTED_EDGE ( 'NONE', *, *, #36996, .F. ) ;
#33609 = DIRECTION ( 'NONE',  ( 1.734723475976806848E-16, 0.000000000000000000, 1.000000000000000000 ) ) ;
#33610 = VERTEX_POINT ( 'NONE', #50165 ) ;
#33611 = DIRECTION ( 'NONE',  ( 0.9959742939952384022, -1.160734090543304907E-16, 0.08963930890344089242 ) ) ;
#33612 = CARTESIAN_POINT ( 'NONE',  ( 1.584529175505357212, 0.03508075509535489578, 1.200674575404337086 ) ) ;
#33613 = VECTOR ( 'NONE', #15815, 39.37007874015748143 ) ;
#33614 = VECTOR ( 'NONE', #41843, 39.37007874015748143 ) ;
#33615 = ORIENTED_EDGE ( 'NONE', *, *, #42715, .F. ) ;
#33616 = ORIENTED_EDGE ( 'NONE', *, *, #34764, .F. ) ;
#33617 = CARTESIAN_POINT ( 'NONE',  ( 0.000000000000000000, 1.574803149606302854, 0.000000000000000000 ) ) ;
#33618 = EDGE_LOOP ( 'NONE', ( #24505, #42052, #21130, #48712 ) ) ;
#33619 = ORIENTED_EDGE ( 'NONE', *, *, #15843, .F. ) ;
#33620 = LINE ( 'NONE', #17602, #5047 ) ;
#33621 = CARTESIAN_POINT ( 'NONE',  ( -0.6214413264104945434, 3.346456692913386100, -2.074263738136479240 ) ) ;
#33622 = FACE_OUTER_BOUND ( 'NONE', #17504, .T. ) ;
#33623 = EDGE_CURVE ( 'NONE', #40629, #30339, #26715, .T. ) ;
#33624 = VERTEX_POINT ( 'NONE', #30852 ) ;
#33625 = CARTESIAN_POINT ( 'NONE',  ( -0.8949303405208606232, 5.905511811023623991, -1.971765468592543424 ) ) ;
#33626 = FACE_OUTER_BOUND ( 'NONE', #11467, .T. ) ;
#33627 = LINE ( 'NONE', #25861, #35218 ) ;
#33628 = EDGE_CURVE ( 'NONE', #20757, #43312, #7358, .T. ) ;
#33629 = VERTEX_POINT ( 'NONE', #28228 ) ;
#33630 = DIRECTION ( 'NONE',  ( -0.9998717552508122886, -0.01601477604151181275, 0.000000000000000000 ) ) ;
#33631 = DIRECTION ( 'NONE',  ( -1.000000000000000000, 0.000000000000000000, 1.734723475976806848E-16 ) ) ;
#33632 = CARTESIAN_POINT ( 'NONE',  ( -1.536664496436148184E-16, 3.267716535433071279, -1.141732283464564013 ) ) ;
#33633 = ORIENTED_EDGE ( 'NONE', *, *, #43554, .T. ) ;
#33634 = VERTEX_POINT ( 'NONE', #8369 ) ;
#33635 = CIRCLE ( 'NONE', #11353, 1.743387098533651480 ) ;
#33636 = B_SPLINE_CURVE_WITH_KNOTS ( 'NONE', 3,
 ( #26579, #50277, #3853, #35354 ),
 .UNSPECIFIED., .F., .F.,
 ( 4, 4 ),
 ( 2.051444212662578114E-07, 0.002500220176209435544 ),
 .UNSPECIFIED. ) ;
#33637 = CARTESIAN_POINT ( 'NONE',  ( -1.598711713507983578, 5.905511811023623991, -1.460438370699401522 ) ) ;
#33638 = DIRECTION ( 'NONE',  ( -0.000000000000000000, 1.000000000000000000, -0.000000000000000000 ) ) ;
#33639 = CARTESIAN_POINT ( 'NONE',  ( 0.000000000000000000, 1.574803149606302854, 0.000000000000000000 ) ) ;
#33640 = ORIENTED_EDGE ( 'NONE', *, *, #24879, .F. ) ;
#33641 = ORIENTED_EDGE ( 'NONE', *, *, #22981, .F. ) ;
#33642 = CARTESIAN_POINT ( 'NONE',  ( -0.4532322590609024759, 0.000000000000000000, -1.827234353172969561 ) ) ;
#33643 = ORIENTED_EDGE ( 'NONE', *, *, #33219, .T. ) ;
#33644 = CARTESIAN_POINT ( 'NONE',  ( 1.091055626815042423, 3.267716535433071279, -1.892679809432644143E-16 ) ) ;
#33645 = CARTESIAN_POINT ( 'NONE',  ( 0.000000000000000000, 3.267716535433071279, 0.4724409448818871482 ) ) ;
#33646 = VECTOR ( 'NONE', #28498, 39.37007874015748143 ) ;
#33647 = VECTOR ( 'NONE', #37154, 39.37007874015748143 ) ;
#33648 = EDGE_CURVE ( 'NONE', #7189, #44444, #20495, .T. ) ;
#33649 = CARTESIAN_POINT ( 'NONE',  ( -0.8067290215918269114, 6.692913385826772199, 2.009464521518169899 ) ) ;
#33650 = FACE_OUTER_BOUND ( 'NONE', #17077, .T. ) ;
#33651 = FACE_OUTER_BOUND ( 'NONE', #32948, .T. ) ;
#33652 = ORIENTED_EDGE ( 'NONE', *, *, #4765, .F. ) ;
#33653 = CARTESIAN_POINT ( 'NONE',  ( 1.215807329263347114, 1.628950133432788494, 1.938968878379255578 ) ) ;
#33654 = CARTESIAN_POINT ( 'NONE',  ( -1.909347346926324462, 0.000000000000000000, 0.4724409448818871482 ) ) ;
#33655 = VECTOR ( 'NONE', #2057, 39.37007874015748143 ) ;
#33656 = DIRECTION ( 'NONE',  ( -1.000000000000000000, 0.000000000000000000, 1.734723475976806848E-16 ) ) ;
#33657 = EDGE_CURVE ( 'NONE', #50226, #39291, #27976, .T. ) ;
#33658 = EDGE_LOOP ( 'NONE', ( #49430, #42126, #18305, #37826 ) ) ;
#33660 = LINE ( 'NONE', #17387, #33965 ) ;
#33659 = VECTOR ( 'NONE', #34366, 39.37007874015748143 ) ;
#33661 = ADVANCED_FACE ( 'NONE', ( #15604 ), #8412, .T. ) ;
#33662 = CARTESIAN_POINT ( 'NONE',  ( 1.695772546416037363, 1.477242674555747426, -2.417756147381349141 ) ) ;
#33663 = PLANE ( 'NONE',  #30455 ) ;
#33665 = EDGE_CURVE ( 'NONE', #19894, #17400, #7858, .T. ) ;
#33664 = EDGE_LOOP ( 'NONE', ( #11361, #49014, #6452, #22362 ) ) ;
#33666 = AXIS2_PLACEMENT_3D ( 'NONE', #43313, #15958, #50760 ) ;
#33667 = CARTESIAN_POINT ( 'NONE',  ( 2.919426793319799707, 5.905511811023623991, 0.4451252810446827413 ) ) ;
#33668 = B_SPLINE_CURVE_WITH_KNOTS ( 'NONE', 3,
 ( #15058, #46021, #26919, #30805 ),
 .UNSPECIFIED., .F., .F.,
 ( 4, 4 ),
 ( 0.01169383523547795622, 0.01426672609628482080 ),
 .UNSPECIFIED. ) ;
#33669 = EDGE_CURVE ( 'NONE', #1365, #36675, #35230, .T. ) ;
#33670 = ORIENTED_EDGE ( 'NONE', *, *, #40507, .F. ) ;
#33671 = CARTESIAN_POINT ( 'NONE',  ( -2.151809081513409438, 6.692913385826772199, 0.2418202932658334581 ) ) ;
#33672 = CARTESIAN_POINT ( 'NONE',  ( 1.008242765982022782, 0.5249316475426860640, 1.591564316133513568 ) ) ;
#33673 = ORIENTED_EDGE ( 'NONE', *, *, #47720, .F. ) ;
#33674 = VECTOR ( 'NONE', #40115, 39.37007874015748143 ) ;
#33675 = CARTESIAN_POINT ( 'NONE',  ( 2.932638728931774352, 5.905511811023623991, 0.3475908556738230293 ) ) ;
#33676 = EDGE_CURVE ( 'NONE', #25851, #38575, #3731, .T. ) ;
#33677 = LINE ( 'NONE', #40898, #11928 ) ;
#33678 = FACE_OUTER_BOUND ( 'NONE', #9354, .T. ) ;
#33679 = CARTESIAN_POINT ( 'NONE',  ( 0.000000000000000000, 0.000000000000000000, 0.000000000000000000 ) ) ;
#33680 = CARTESIAN_POINT ( 'NONE',  ( 1.202103465198962384, 0.5249316497054294928, 1.450716274357264135 ) ) ;
#33681 = EDGE_LOOP ( 'NONE', ( #26567, #5841, #30945, #26248 ) ) ;
#33682 = EDGE_LOOP ( 'NONE', ( #48692, #8, #31036, #46140 ) ) ;
#33683 = CARTESIAN_POINT ( 'NONE',  ( -1.416899275789439194, 0.001784216570024398704, 1.066994191199830633 ) ) ;
#33684 = CARTESIAN_POINT ( 'NONE',  ( 0.8182917201112817063, 3.346456692913386100, -1.614173228346451605 ) ) ;
#33685 = ORIENTED_EDGE ( 'NONE', *, *, #45074, .F. ) ;
#33686 = DIRECTION ( 'NONE',  ( -0.000000000000000000, 1.000000000000000000, -0.000000000000000000 ) ) ;
#33687 = CARTESIAN_POINT ( 'NONE',  ( 0.1968503937007872462, 3.267716535433071279, -1.771653543307081025 ) ) ;
#33688 = LINE ( 'NONE', #9673, #11279 ) ;
#33689 = EDGE_CURVE ( 'NONE', #14887, #14557, #4234, .T. ) ;
#33690 = EDGE_LOOP ( 'NONE', ( #36866, #4479, #37653, #29351 ) ) ;
#33691 = VERTEX_POINT ( 'NONE', #47052 ) ;
#33692 = CARTESIAN_POINT ( 'NONE',  ( -1.738955188402737440, 0.000000000000000000, -0.1273587697465547175 ) ) ;
#33693 = CARTESIAN_POINT ( 'NONE',  ( 0.5756566573088583993, 1.728235332270611879, 2.896516654582643291 ) ) ;
#33694 = VECTOR ( 'NONE', #43801, 39.37007874015748143 ) ;
#33695 = DIRECTION ( 'NONE',  ( -3.469446951953613696E-16, 0.000000000000000000, -1.000000000000000000 ) ) ;
#33696 = ADVANCED_FACE ( 'NONE', ( #12491 ), #50910, .T. ) ;
#33697 = VERTEX_POINT ( 'NONE', #11724 ) ;
#33698 = CARTESIAN_POINT ( 'NONE',  ( 0.08119777152254364916, 1.623385212329073957, 0.000000000000000000 ) ) ;
#33699 = CARTESIAN_POINT ( 'NONE',  ( 0.000000000000000000, 0.000000000000000000, 0.000000000000000000 ) ) ;
#33700 = ORIENTED_EDGE ( 'NONE', *, *, #14212, .T. ) ;
#33701 = ADVANCED_FACE ( 'NONE', ( #43461 ), #16112, .F. ) ;
#33702 = DIRECTION ( 'NONE',  ( -0.000000000000000000, 1.000000000000000000, -0.000000000000000000 ) ) ;
#33703 = VERTEX_POINT ( 'NONE', #23856 ) ;
#33705 = VERTEX_POINT ( 'NONE', #43207 ) ;
#33704 = AXIS2_PLACEMENT_3D ( 'NONE', #41940, #22326, #18449 ) ;
#33706 = PLANE ( 'NONE',  #22952 ) ;
#33707 = DIRECTION ( 'NONE',  ( 0.000000000000000000, 0.000000000000000000, -1.000000000000000000 ) ) ;
#33708 = CLOSED_SHELL ( 'NONE', ( #27480, #51007, #42695, #29808, #14151, #20725, #43208, #15982, #40296, #17194, #21416, #18054, #22371, #19393, #25864, #10524, #46227, #39412, #31169, #48943, #16785, #8979, #13924, #9715, #49526, #1391, #45779, #40023, #16278, #10461, #31485, #32775, #13723, #1501, #16204 ) ) ;
#33709 = VECTOR ( 'NONE', #21979, 39.37007874015748143 ) ;
#33710 = ORIENTED_EDGE ( 'NONE', *, *, #13585, .T. ) ;
#33711 = CARTESIAN_POINT ( 'NONE',  ( 0.3381173457103291979, 1.574803149606302854, 2.138793126519850762 ) ) ;
#33712 = EDGE_CURVE ( 'NONE', #10053, #17342, #101, .T. ) ;
#33714 = DIRECTION ( 'NONE',  ( -0.000000000000000000, 1.000000000000000000, -0.000000000000000000 ) ) ;
#33713 = AXIS2_PLACEMENT_3D ( 'NONE', #25242, #33516, #18254 ) ;
#33715 = ORIENTED_EDGE ( 'NONE', *, *, #40374, .F. ) ;
#33716 = AXIS2_PLACEMENT_3D ( 'NONE', #24700, #44806, #4820 ) ;
#33717 = DIRECTION ( 'NONE',  ( 0.000000000000000000, 0.000000000000000000, 1.000000000000000000 ) ) ;
#33718 = CARTESIAN_POINT ( 'NONE',  ( -1.439733046521776583, 3.346456692913386100, 1.537421584259135443 ) ) ;
#33719 = VECTOR ( 'NONE', #18331, 39.37007874015748143 ) ;
#33720 = DIRECTION ( 'NONE',  ( -0.000000000000000000, 0.000000000000000000, 1.000000000000000000 ) ) ;
#33721 = DIRECTION ( 'NONE',  ( -1.000000000000000000, -0.000000000000000000, -0.000000000000000000 ) ) ;
#33722 = CARTESIAN_POINT ( 'NONE',  ( -0.2430652128771642606, 5.905511811023623991, -2.151668812760861638 ) ) ;
#33723 = ORIENTED_EDGE ( 'NONE', *, *, #32297, .F. ) ;
#33724 = CARTESIAN_POINT ( 'NONE',  ( -1.598711713507983578, 6.692913385826772199, -1.460438370699401966 ) ) ;
#33725 = CARTESIAN_POINT ( 'NONE',  ( -0.5455278134075208785, 0.000000000000000000, 1.889763779527550369 ) ) ;
#33726 = ORIENTED_EDGE ( 'NONE', *, *, #9783, .T. ) ;
#33727 = FACE_OUTER_BOUND ( 'NONE', #42460, .T. ) ;
#33728 = ADVANCED_FACE ( 'NONE', ( #8110 ), #24371, .F. ) ;
#33729 = CARTESIAN_POINT ( 'NONE',  ( 1.090138530625467839, 6.692913385826772199, 1.920534397867778020 ) ) ;
#33730 = ORIENTED_EDGE ( 'NONE', *, *, #1274, .F. ) ;
#33731 = LINE ( 'NONE', #46068, #40289 ) ;
#33732 = EDGE_CURVE ( 'NONE', #30403, #24144, #6984, .T. ) ;
#33733 = DIRECTION ( 'NONE',  ( -1.000000000000000000, 0.000000000000000000, -0.000000000000000000 ) ) ;
#33734 = ADVANCED_FACE ( 'NONE', ( #24111 ), #40120, .T. ) ;
#33735 = DIRECTION ( 'NONE',  ( 0.000000000000000000, 0.000000000000000000, -1.000000000000000000 ) ) ;
#33736 = EDGE_LOOP ( 'NONE', ( #32714, #2024, #37149, #34517 ) ) ;
#33737 = CARTESIAN_POINT ( 'NONE',  ( -1.985260859929298016, 0.000000000000000000, -0.6299212598425177889 ) ) ;
#33738 = ORIENTED_EDGE ( 'NONE', *, *, #50740, .T. ) ;
#33739 = CARTESIAN_POINT ( 'NONE',  ( -1.909347346926324462, 0.000000000000000000, 0.4724409448818871482 ) ) ;
#33740 = CARTESIAN_POINT ( 'NONE',  ( 2.319222573356612749, 1.745048544795088308, -0.1534186080535354380 ) ) ;
#33741 = VECTOR ( 'NONE', #10180, 39.37007874015748143 ) ;
#33742 = VECTOR ( 'NONE', #46642, 39.37007874015748143 ) ;
#33743 = CARTESIAN_POINT ( 'NONE',  ( -0.2727639067037607723, 0.000000000000000000, 2.362204724409437961 ) ) ;
#33744 = CARTESIAN_POINT ( 'NONE',  ( -1.985260859929297794, 0.000000000000000000, 0.1181102362204704270 ) ) ;
#33745 = VECTOR ( 'NONE', #29443, 39.37007874015748143 ) ;
#33746 = ORIENTED_EDGE ( 'NONE', *, *, #34362, .F. ) ;
#33747 = ORIENTED_EDGE ( 'NONE', *, *, #30302, .F. ) ;
#33748 = CARTESIAN_POINT ( 'NONE',  ( -1.088355899089957335, 1.624853143508943942, 1.917550775237487848 ) ) ;
#33749 = EDGE_CURVE ( 'NONE', #5813, #25880, #16375, .T. ) ;
#33750 = VECTOR ( 'NONE', #11726, 39.37007874015748143 ) ;
#33751 = DIRECTION ( 'NONE',  ( 0.000000000000000000, 0.000000000000000000, -1.000000000000000000 ) ) ;
#33752 = ORIENTED_EDGE ( 'NONE', *, *, #50034, .T. ) ;
#33753 = DIRECTION ( 'NONE',  ( -3.469446951953613696E-16, 0.000000000000000000, -1.000000000000000000 ) ) ;
#33754 = EDGE_CURVE ( 'NONE', #28752, #7505, #32127, .T. ) ;
#33755 = ORIENTED_EDGE ( 'NONE', *, *, #9388, .F. ) ;
#33756 = DIRECTION ( 'NONE',  ( 0.8805955318567321166, 0.000000000000000000, 0.4738686624730094055 ) ) ;
#33757 = EDGE_CURVE ( 'NONE', #43500, #36035, #20515, .T. ) ;
#33758 = CARTESIAN_POINT ( 'NONE',  ( 2.437180031585944207, 1.757239404341893518, -1.667735833703099191 ) ) ;
#33759 = EDGE_LOOP ( 'NONE', ( #2236, #29909, #9501, #37486 ) ) ;
#33760 = EDGE_CURVE ( 'NONE', #34134, #48339, #25452, .T. ) ;
#33761 = EDGE_CURVE ( 'NONE', #42844, #13877, #42953, .T. ) ;
#33762 = LINE ( 'NONE', #26491, #43020 ) ;
#33763 = ORIENTED_EDGE ( 'NONE', *, *, #37352, .T. ) ;
#33764 = ORIENTED_EDGE ( 'NONE', *, *, #3770, .T. ) ;
#33765 = ORIENTED_EDGE ( 'NONE', *, *, #11327, .T. ) ;
#33766 = EDGE_LOOP ( 'NONE', ( #6127, #46958, #47527, #29607 ) ) ;
#33767 = DIRECTION ( 'NONE',  ( 0.000000000000000000, 0.000000000000000000, 1.000000000000000000 ) ) ;
#33768 = ORIENTED_EDGE ( 'NONE', *, *, #29269, .F. ) ;
#33769 = DIRECTION ( 'NONE',  ( -0.000000000000000000, 1.000000000000000000, -0.000000000000000000 ) ) ;
#33770 = CARTESIAN_POINT ( 'NONE',  ( 0.08139965876239094178, 1.610780518492231694, 0.000000000000000000 ) ) ;
#33771 = AXIS2_PLACEMENT_3D ( 'NONE', #21028, #9149, #24898 ) ;
#33772 = CARTESIAN_POINT ( 'NONE',  ( -1.363819533518803473, 0.000000000000000000, -1.417322834645664109 ) ) ;
#33773 = B_SPLINE_CURVE_WITH_KNOTS ( 'NONE', 3,
 ( #19077, #46420, #39467, #42821 ),
 .UNSPECIFIED., .F., .F.,
 ( 4, 4 ),
 ( 2.034152094176694738E-07, 0.002500799499442713479 ),
 .UNSPECIFIED. ) ;
#33774 = VECTOR ( 'NONE', #49855, 39.37007874015748143 ) ;
#33775 = DIRECTION ( 'NONE',  ( 1.000000000000000000, 0.000000000000000000, 0.000000000000000000 ) ) ;
#33776 = CARTESIAN_POINT ( 'NONE',  ( -0.2727639067037602172, 3.346456692913386100, 1.417322834645662777 ) ) ;
#33777 = ORIENTED_EDGE ( 'NONE', *, *, #33266, .F. ) ;
#33778 = DIRECTION ( 'NONE',  ( 0.000000000000000000, 0.000000000000000000, -1.000000000000000000 ) ) ;
#33779 = LINE ( 'NONE', #21633, #39837 ) ;
#33780 = VECTOR ( 'NONE', #813, 39.37007874015748143 ) ;
#33781 = LINE ( 'NONE', #34027, #7873 ) ;
#33782 = CARTESIAN_POINT ( 'NONE',  ( -1.530693736245496206, 6.692913385826772199, -1.531579597454065800 ) ) ;
#33783 = ORIENTED_EDGE ( 'NONE', *, *, #21768, .F. ) ;
#33784 = DIRECTION ( 'NONE',  ( -0.000000000000000000, 1.000000000000000000, -0.000000000000000000 ) ) ;
#33785 = DIRECTION ( 'NONE',  ( 1.734723475976806848E-16, -0.000000000000000000, 1.000000000000000000 ) ) ;
#33786 = VERTEX_POINT ( 'NONE', #17898 ) ;
#33787 = LINE ( 'NONE', #18025, #44401 ) ;
#33788 = DIRECTION ( 'NONE',  ( -0.000000000000000000, 1.000000000000000000, -0.000000000000000000 ) ) ;
#33789 = EDGE_CURVE ( 'NONE', #17493, #9684, #41148, .T. ) ;
#33790 = ORIENTED_EDGE ( 'NONE', *, *, #31555, .F. ) ;
#33791 = CARTESIAN_POINT ( 'NONE',  ( -0.5304089168012655620, 0.01942419597810423823, -1.736909402037482675 ) ) ;
#33792 = EDGE_CURVE ( 'NONE', #50444, #24086, #5003, .T. ) ;
#33793 = EDGE_LOOP ( 'NONE', ( #5031, #32614, #33296, #15305, #19175, #31163, #37049, #29035, #47001, #17887, #10981 ) ) ;
#33794 = CARTESIAN_POINT ( 'NONE',  ( -1.109766902767011398, 1.694103061027446788, -2.191031250744368553 ) ) ;
#33795 = EDGE_CURVE ( 'NONE', #23374, #3496, #21514, .T. ) ;
#33796 = DIRECTION ( 'NONE',  ( -1.000000000000000000, 0.000000000000000000, -0.000000000000000000 ) ) ;
#33797 = LINE ( 'NONE', #4504, #30362 ) ;
#33798 = DIRECTION ( 'NONE',  ( -1.000000000000000000, 0.000000000000000000, -0.000000000000000000 ) ) ;
#33799 = LINE ( 'NONE', #30670, #37641 ) ;
#33800 = AXIS2_PLACEMENT_3D ( 'NONE', #46701, #11369, #42848 ) ;
#33801 = ORIENTED_EDGE ( 'NONE', *, *, #33628, .T. ) ;
#33802 = CARTESIAN_POINT ( 'NONE',  ( -2.867773316779185677, 1.576133919414932638, -0.7050287376752426560 ) ) ;
#33803 = ORIENTED_EDGE ( 'NONE', *, *, #49969, .F. ) ;
#33804 = VERTEX_POINT ( 'NONE', #41394 ) ;
#33805 = LINE ( 'NONE', #24571, #30361 ) ;
#33806 = VERTEX_POINT ( 'NONE', #33412 ) ;
#33807 = CARTESIAN_POINT ( 'NONE',  ( -0.8182917201112814842, 3.346456692913386100, 0.9055118110236167750 ) ) ;
#33808 = DIRECTION ( 'NONE',  ( 1.734723475976806848E-16, 0.000000000000000000, 1.000000000000000000 ) ) ;
#33809 = EDGE_LOOP ( 'NONE', ( #1258, #45445, #21272, #29501 ) ) ;
#33810 = VECTOR ( 'NONE', #31015, 39.37007874015748143 ) ;
#33811 = LINE ( 'NONE', #29918, #26424 ) ;
#33812 = EDGE_CURVE ( 'NONE', #18870, #49731, #48583, .T. ) ;
#33813 = LINE ( 'NONE', #45894, #40572 ) ;
#33814 = DIRECTION ( 'NONE',  ( 1.000000000000000000, 0.000000000000000000, 0.000000000000000000 ) ) ;
#33815 = ORIENTED_EDGE ( 'NONE', *, *, #30942, .F. ) ;
#33816 = ORIENTED_EDGE ( 'NONE', *, *, #7315, .F. ) ;
#33817 = ADVANCED_FACE ( 'NONE', ( #5513 ), #9646, .F. ) ;
#33818 = DIRECTION ( 'NONE',  ( -0.1342332658176522420, 0.000000000000000000, -0.9909497617679352555 ) ) ;
#33819 = FACE_BOUND ( 'NONE', #3896, .T. ) ;
#33820 = ORIENTED_EDGE ( 'NONE', *, *, #37018, .F. ) ;
#33821 = AXIS2_PLACEMENT_3D ( 'NONE', #35175, #7805, #12438 ) ;
#33822 = DIRECTION ( 'NONE',  ( -0.000000000000000000, 1.000000000000000000, 0.000000000000000000 ) ) ;
#33823 = CARTESIAN_POINT ( 'NONE',  ( -1.091055626815042867, 3.267716535433071279, 1.892679809432645129E-16 ) ) ;
#33824 = ORIENTED_EDGE ( 'NONE', *, *, #45541, .T. ) ;
#33825 = EDGE_LOOP ( 'NONE', ( #16714, #20789, #28339, #5716 ) ) ;
#33826 = DIRECTION ( 'NONE',  ( -0.000000000000000000, 1.000000000000000000, -0.000000000000000000 ) ) ;
#33827 = DIRECTION ( 'NONE',  ( 0.000000000000000000, 0.000000000000000000, -1.000000000000000000 ) ) ;
#33828 = ORIENTED_EDGE ( 'NONE', *, *, #32208, .F. ) ;
#33829 = ORIENTED_EDGE ( 'NONE', *, *, #20311, .T. ) ;
#33830 = EDGE_LOOP ( 'NONE', ( #20864, #11994, #50589, #13215 ) ) ;
#33831 = PLANE ( 'NONE',  #20253 ) ;
#33832 = PLANE ( 'NONE',  #5191 ) ;
#33833 = CARTESIAN_POINT ( 'NONE',  ( 2.126910391174609671, 1.205361022782829114E-17, 0.2384475364948296372 ) ) ;
#33834 = DIRECTION ( 'NONE',  ( -0.000000000000000000, 1.000000000000000000, -0.000000000000000000 ) ) ;
#33835 = B_SPLINE_CURVE_WITH_KNOTS ( 'NONE', 3,
 ( #44619, #40772, #16513, #44115 ),
 .UNSPECIFIED., .F., .F.,
 ( 4, 4 ),
 ( 2.136435329377818075E-07, 0.002500479846613039119 ),
 .UNSPECIFIED. ) ;
#33836 = ORIENTED_EDGE ( 'NONE', *, *, #42206, .T. ) ;
#33837 = ORIENTED_EDGE ( 'NONE', *, *, #13702, .T. ) ;
#33838 = CARTESIAN_POINT ( 'NONE',  ( -1.091055626815042201, 0.000000000000000000, 0.1181102362204705658 ) ) ;
#33839 = DIRECTION ( 'NONE',  ( -0.000000000000000000, 1.000000000000000000, -0.000000000000000000 ) ) ;
#33840 = CARTESIAN_POINT ( 'NONE',  ( -1.091055626815042645, 0.000000000000000000, 2.007874015748021268 ) ) ;
#33841 = CARTESIAN_POINT ( 'NONE',  ( -0.4460728916448887249, 1.700757277111965449, 2.182451250484750638 ) ) ;
#33842 = DIRECTION ( 'NONE',  ( -0.000000000000000000, 1.000000000000000000, -0.000000000000000000 ) ) ;
#33843 = VECTOR ( 'NONE', #10260, 39.37007874015748143 ) ;
#33844 = AXIS2_PLACEMENT_3D ( 'NONE', #23322, #39330, #31084 ) ;
#33845 = DIRECTION ( 'NONE',  ( -0.000000000000000000, 1.000000000000000000, -0.000000000000000000 ) ) ;
#33846 = CARTESIAN_POINT ( 'NONE',  ( 0.8329809839909850799, 1.732245219823249638, -2.833254665166554442 ) ) ;
#33847 = ADVANCED_FACE ( 'NONE', ( #40886 ), #8874, .F. ) ;
#33848 = ORIENTED_EDGE ( 'NONE', *, *, #12198, .F. ) ;
#33849 = DIRECTION ( 'NONE',  ( -0.000000000000000000, 1.000000000000000000, -0.000000000000000000 ) ) ;
#33850 = LINE ( 'NONE', #13964, #48262 ) ;
#33851 = EDGE_CURVE ( 'NONE', #29709, #37961, #33660, .T. ) ;
#33852 = VECTOR ( 'NONE', #24263, 39.37007874015748143 ) ;
#33853 = ORIENTED_EDGE ( 'NONE', *, *, #2245, .F. ) ;
#33854 = EDGE_CURVE ( 'NONE', #28852, #15326, #5252, .T. ) ;
#33855 = VERTEX_POINT ( 'NONE', #44235 ) ;
#33856 = LINE ( 'NONE', #41588, #22878 ) ;
#33857 = ORIENTED_EDGE ( 'NONE', *, *, #47394, .F. ) ;
#33858 = ADVANCED_FACE ( 'NONE', ( #1382 ), #37531, .F. ) ;
#33859 = B_SPLINE_CURVE_WITH_KNOTS ( 'NONE', 3,
 ( #37665, #41275, #40764, #1520 ),
 .UNSPECIFIED., .F., .F.,
 ( 4, 4 ),
 ( 6.511653002970408202E-07, 0.004414110768476271068 ),
 .UNSPECIFIED. ) ;
#33860 = ORIENTED_EDGE ( 'NONE', *, *, #32499, .F. ) ;
#33861 = LINE ( 'NONE', #41846, #35303 ) ;
#33862 = VERTEX_POINT ( 'NONE', #33153 ) ;
#33863 = DIRECTION ( 'NONE',  ( -1.000000000000000000, -0.000000000000000000, -0.000000000000000000 ) ) ;
#33864 = DIRECTION ( 'NONE',  ( -1.000000000000000000, -0.000000000000000000, -0.000000000000000000 ) ) ;
#33865 = EDGE_CURVE ( 'NONE', #18980, #39410, #45236, .T. ) ;
#33866 = ORIENTED_EDGE ( 'NONE', *, *, #27386, .F. ) ;
#33867 =( REPRESENTATION_RELATIONSHIP ('NONE','NONE', #50198, #50787 ) REPRESENTATION_RELATIONSHIP_WITH_TRANSFORMATION ( #24018 )SHAPE_REPRESENTATION_RELATIONSHIP( ) );
#33868 = ORIENTED_EDGE ( 'NONE', *, *, #17227, .T. ) ;
#33869 = CARTESIAN_POINT ( 'NONE',  ( 1.363819533518803251, 3.346456692913386100, 1.102362204724403938 ) ) ;
#33870 = EDGE_LOOP ( 'NONE', ( #33002, #6744, #12693, #42938 ) ) ;
#33871 = ORIENTED_EDGE ( 'NONE', *, *, #42836, .T. ) ;
#33872 = EDGE_CURVE ( 'NONE', #33855, #30686, #13519, .T. ) ;
#33873 = CARTESIAN_POINT ( 'NONE',  ( -1.977157105026591699, 1.676234161373136189, -0.8985969286390745880 ) ) ;
#33874 = DIRECTION ( 'NONE',  ( 0.000000000000000000, 0.000000000000000000, -1.000000000000000000 ) ) ;
#33875 = CARTESIAN_POINT ( 'NONE',  ( -1.383870272338435070, 0.000000000000000000, 1.124517572066690452 ) ) ;
#33876 = CARTESIAN_POINT ( 'NONE',  ( 0.8291286199751974895, 1.205361022782829114E-17, -1.835126787948130556 ) ) ;
#33877 = CIRCLE ( 'NONE', #10756, 2.165354330708661568 ) ;
#33878 = ORIENTED_EDGE ( 'NONE', *, *, #20764, .T. ) ;
#33879 = DIRECTION ( 'NONE',  ( -0.000000000000000000, 1.000000000000000000, -0.000000000000000000 ) ) ;
#33880 = CARTESIAN_POINT ( 'NONE',  ( -1.661821349926435376, 6.692913385826772199, 1.388203579611951621 ) ) ;
#33881 = CARTESIAN_POINT ( 'NONE',  ( 1.909347346926324462, 3.346456692913386100, -0.8893194486674360633 ) ) ;
#33882 = ORIENTED_EDGE ( 'NONE', *, *, #47886, .F. ) ;
#33883 = PLANE ( 'NONE',  #20778 ) ;
#33884 = LINE ( 'NONE', #10379, #30188 ) ;
#33885 = FACE_OUTER_BOUND ( 'NONE', #5189, .T. ) ;
#33886 = ORIENTED_EDGE ( 'NONE', *, *, #28848, .T. ) ;
#33887 = ORIENTED_EDGE ( 'NONE', *, *, #49831, .F. ) ;
#33888 = VECTOR ( 'NONE', #48416, 39.37007874015748143 ) ;
#33889 = EDGE_CURVE ( 'NONE', #46463, #13286, #29256, .T. ) ;
#33890 = DIRECTION ( 'NONE',  ( -0.000000000000000000, 1.000000000000000000, -0.000000000000000000 ) ) ;
#33891 = DIRECTION ( 'NONE',  ( 0.9998717552508121775, 0.01601477604151182663, 0.000000000000000000 ) ) ;
#33892 = LINE ( 'NONE', #6764, #19699 ) ;
#33893 = ORIENTED_EDGE ( 'NONE', *, *, #1603, .F. ) ;
#33894 = EDGE_LOOP ( 'NONE', ( #46267, #2548, #16454, #20439 ) ) ;
#33895 = DIRECTION ( 'NONE',  ( 0.000000000000000000, 0.000000000000000000, -1.000000000000000000 ) ) ;
#33896 = ORIENTED_EDGE ( 'NONE', *, *, #35053, .F. ) ;
#33897 = CARTESIAN_POINT ( 'NONE',  ( 0.5455278134075216556, 3.346456692913386100, 1.062992125984246083 ) ) ;
#33898 = DIRECTION ( 'NONE',  ( 0.000000000000000000, 0.000000000000000000, -1.000000000000000000 ) ) ;
#33899 = CARTESIAN_POINT ( 'NONE',  ( 0.000000000000000000, 0.000000000000000000, 0.000000000000000000 ) ) ;
#33900 = FACE_OUTER_BOUND ( 'NONE', #16793, .T. ) ;
#33901 = CARTESIAN_POINT ( 'NONE',  ( -0.07591351300297277671, 3.267716535433071279, 1.417322834645662777 ) ) ;
#33902 = EDGE_LOOP ( 'NONE', ( #43218, #38969, #13203 ) ) ;
#33903 = DIRECTION ( 'NONE',  ( -0.000000000000000000, -1.000000000000000000, 0.000000000000000000 ) ) ;
#33904 = SURFACE_STYLE_FILL_AREA ( #25891 ) ;
#33905 = DIRECTION ( 'NONE',  ( -0.000000000000000000, 1.000000000000000000, -0.000000000000000000 ) ) ;
#33906 = EDGE_CURVE ( 'NONE', #42620, #4245, #21773, .T. ) ;
#33907 = AXIS2_PLACEMENT_3D ( 'NONE', #14463, #2338, #33594 ) ;
#33908 = ORIENTED_EDGE ( 'NONE', *, *, #32270, .T. ) ;
#33909 = CARTESIAN_POINT ( 'NONE',  ( 0.000000000000000000, 3.346456692913386100, 0.000000000000000000 ) ) ;
#33910 = VECTOR ( 'NONE', #12587, 39.37007874015748854 ) ;
#33911 = DIRECTION ( 'NONE',  ( 8.882339915255740720E-16, 0.000000000000000000, 1.000000000000000000 ) ) ;
#33912 = CARTESIAN_POINT ( 'NONE',  ( -2.182111253630085290, 0.000000000000000000, -6.146657985744592735E-16 ) ) ;
#33913 = EDGE_CURVE ( 'NONE', #28182, #50367, #28743, .T. ) ;
#33914 = VERTEX_POINT ( 'NONE', #1122 ) ;
#33915 = ADVANCED_FACE ( 'NONE', ( #17642 ), #47093, .T. ) ;
#33916 = DIRECTION ( 'NONE',  ( 0.8090169943749422332, 0.000000000000000000, 0.5877852522924802425 ) ) ;
#33917 = ORIENTED_EDGE ( 'NONE', *, *, #33789, .F. ) ;
#33918 = DIRECTION ( 'NONE',  ( -1.000000000000000000, -0.000000000000000000, -0.000000000000000000 ) ) ;
#33919 = VECTOR ( 'NONE', #48357, 39.37007874015748854 ) ;
#33920 = CARTESIAN_POINT ( 'NONE',  ( -0.8182917201112819283, 0.000000000000000000, 0.1574803149606285035 ) ) ;
#33921 = ORIENTED_EDGE ( 'NONE', *, *, #3894, .F. ) ;
#33922 = DIRECTION ( 'NONE',  ( -3.469446951953613696E-16, 0.000000000000000000, -1.000000000000000000 ) ) ;
#33923 = VECTOR ( 'NONE', #7663, 39.37007874015748143 ) ;
#33924 = DIRECTION ( 'NONE',  ( -0.8805955318567321166, 0.000000000000000000, -0.4738686624730094055 ) ) ;
#33925 = DIRECTION ( 'NONE',  ( -1.000000000000000000, -0.000000000000000000, -0.000000000000000000 ) ) ;
#33926 = DIRECTION ( 'NONE',  ( -1.000000000000000000, 0.000000000000000000, -0.000000000000000000 ) ) ;
#33927 = VERTEX_POINT ( 'NONE', #22529 ) ;
#33928 = ORIENTED_EDGE ( 'NONE', *, *, #42702, .T. ) ;
#33929 = DIRECTION ( 'NONE',  ( 0.000000000000000000, 0.000000000000000000, 1.000000000000000000 ) ) ;
#33930 = DIRECTION ( 'NONE',  ( 0.000000000000000000, 0.000000000000000000, -1.000000000000000000 ) ) ;
#33931 = VERTEX_POINT ( 'NONE', #14275 ) ;
#33932 = DIRECTION ( 'NONE',  ( 0.000000000000000000, 0.000000000000000000, -1.000000000000000000 ) ) ;
#33933 = CARTESIAN_POINT ( 'NONE',  ( -0.9302092402134520821, 3.346456692913386100, -1.889763779527552146 ) ) ;
#33934 = LINE ( 'NONE', #37557, #36836 ) ;
#33935 = ORIENTED_EDGE ( 'NONE', *, *, #47020, .T. ) ;
#33936 = EDGE_LOOP ( 'NONE', ( #38024, #6994, #45365, #36068, #29527, #13724 ) ) ;
#33937 = DIRECTION ( 'NONE',  ( -1.000000000000000000, 0.000000000000000000, 1.734723475976806848E-16 ) ) ;
#33938 = LINE ( 'NONE', #17420, #31578 ) ;
#33939 = ADVANCED_FACE ( 'NONE', ( #49848 ), #18154, .F. ) ;
#33940 = DIRECTION ( 'NONE',  ( 1.734723475976806848E-16, -0.000000000000000000, 1.000000000000000000 ) ) ;
#33941 = ORIENTED_EDGE ( 'NONE', *, *, #39602, .F. ) ;
#33942 = DIRECTION ( 'NONE',  ( -0.9998717552508122886, -0.01601477604151185785, 0.000000000000000000 ) ) ;
#33943 = FACE_BOUND ( 'NONE', #17688, .T. ) ;
#33944 = ORIENTED_EDGE ( 'NONE', *, *, #24865, .T. ) ;
#33945 = DIRECTION ( 'NONE',  ( 1.000000000000000000, -0.000000000000000000, 0.000000000000000000 ) ) ;
#33946 = VERTEX_POINT ( 'NONE', #38292 ) ;
#33947 = ORIENTED_EDGE ( 'NONE', *, *, #21611, .T. ) ;
#33948 = DIRECTION ( 'NONE',  ( 1.734723475976806848E-16, -0.000000000000000000, 1.000000000000000000 ) ) ;
#33949 = CARTESIAN_POINT ( 'NONE',  ( 0.6233543567505470673, 5.905511811023623991, -2.073689640095371267 ) ) ;
#33950 = ADVANCED_FACE ( 'NONE', ( #14024 ), #14535, .F. ) ;
#33951 = VECTOR ( 'NONE', #9709, 39.37007874015748143 ) ;
#33953 = VECTOR ( 'NONE', #44009, 39.37007874015748143 ) ;
#33952 = DIRECTION ( 'NONE',  ( -0.7071067811865481278, 0.7071067811865469066, 4.592716591420704405E-16 ) ) ;
#33954 = ORIENTED_EDGE ( 'NONE', *, *, #22914, .T. ) ;
#33955 = CARTESIAN_POINT ( 'NONE',  ( 1.583112249919723213, 0.000000000000000000, -0.7301740747847023094 ) ) ;
#33956 = PLANE ( 'NONE',  #5713 ) ;
#33957 = ORIENTED_EDGE ( 'NONE', *, *, #1374, .T. ) ;
#33958 = AXIS2_PLACEMENT_3D ( 'NONE', #37040, #13287, #49114 ) ;
#33959 = EDGE_CURVE ( 'NONE', #7103, #21112, #141, .T. ) ;
#33960 = VECTOR ( 'NONE', #25292, 39.37007874015748143 ) ;
#33961 = ORIENTED_EDGE ( 'NONE', *, *, #9337, .T. ) ;
#33962 = CARTESIAN_POINT ( 'NONE',  ( 1.062992125984251413, 0.4724409448818890911, -1.181102362204724754 ) ) ;
#33963 = DIRECTION ( 'NONE',  ( 0.000000000000000000, 1.000000000000000000, 0.000000000000000000 ) ) ;
#33964 = EDGE_CURVE ( 'NONE', #3242, #26125, #46000, .T. ) ;
#33965 = VECTOR ( 'NONE', #12755, 39.37007874015748143 ) ;
#33966 = CARTESIAN_POINT ( 'NONE',  ( 1.015142113812069313, 3.267716535433071279, 0.5905511811023579360 ) ) ;
#33967 = CARTESIAN_POINT ( 'NONE',  ( -1.661616293559047497, 0.000000000000000000, 0.5571161510599360600 ) ) ;
#33968 = DIRECTION ( 'NONE',  ( 1.734723475976806848E-16, 0.000000000000000000, 1.000000000000000000 ) ) ;
#33969 = ORIENTED_EDGE ( 'NONE', *, *, #45874, .F. ) ;
#33970 = FACE_BOUND ( 'NONE', #8321, .T. ) ;
#33971 = DIRECTION ( 'NONE',  ( -0.000000000000000000, 0.000000000000000000, 1.000000000000000000 ) ) ;
#33972 = ADVANCED_FACE ( 'NONE', ( #7293 ), #42144, .F. ) ;
#33973 = ORIENTED_EDGE ( 'NONE', *, *, #29220, .F. ) ;
#33974 = CARTESIAN_POINT ( 'NONE',  ( 1.636583440222563635, 0.000000000000000000, -1.259842519685035800 ) ) ;
#33975 = LINE ( 'NONE', #17712, #47478 ) ;
#33976 = VERTEX_POINT ( 'NONE', #26649 ) ;
#33977 = DIRECTION ( 'NONE',  ( -1.000000000000000000, 0.000000000000000000, 0.000000000000000000 ) ) ;
#33978 = EDGE_CURVE ( 'NONE', #16368, #15591, #41648, .T. ) ;
#33979 = CARTESIAN_POINT ( 'NONE',  ( 0.8455406139730251569, 3.346456692913386100, -1.929133858267711110 ) ) ;
#33980 = EDGE_CURVE ( 'NONE', #21949, #26003, #38092, .T. ) ;
#33981 = CARTESIAN_POINT ( 'NONE',  ( 0.000000000000000000, 1.574803149606302854, 0.000000000000000000 ) ) ;
#33982 = ORIENTED_EDGE ( 'NONE', *, *, #28395, .T. ) ;
#33983 = CARTESIAN_POINT ( 'NONE',  ( 0.2727639067037602172, 3.346456692913386100, -2.047244094488182231 ) ) ;
#33984 = VERTEX_POINT ( 'NONE', #34411 ) ;
#33985 = FACE_BOUND ( 'NONE', #46349, .T. ) ;
#33986 = DIRECTION ( 'NONE',  ( 0.2225209339563041788, 0.000000000000000000, 0.9749279121818259508 ) ) ;
#33987 = CONICAL_SURFACE ( 'NONE', #10855, 2.244934639244524632, 1.554780866114618743 ) ;
#33988 = AXIS2_PLACEMENT_3D ( 'NONE', #18374, #37246, #29740 ) ;
#33989 = DIRECTION ( 'NONE',  ( -0.000000000000000000, 1.000000000000000000, -0.000000000000000000 ) ) ;
#33990 = DIRECTION ( 'NONE',  ( -0.5128992774059071280, 0.000000000000000000, 0.8584487936018655452 ) ) ;
#33991 = CIRCLE ( 'NONE', #11712, 2.244934639244525076 ) ;
#33992 = VERTEX_POINT ( 'NONE', #45743 ) ;
#33993 = ORIENTED_EDGE ( 'NONE', *, *, #10201, .T. ) ;
#33994 = FACE_OUTER_BOUND ( 'NONE', #10935, .T. ) ;
#33995 = VECTOR ( 'NONE', #26435, 39.37007874015748143 ) ;
#33996 = DIRECTION ( 'NONE',  ( -0.000000000000000000, 1.000000000000000000, -0.000000000000000000 ) ) ;
#33997 = ORIENTED_EDGE ( 'NONE', *, *, #36738, .F. ) ;
#33998 = FACE_OUTER_BOUND ( 'NONE', #40716, .T. ) ;
#33999 = VECTOR ( 'NONE', #25327, 39.37007874015748143 ) ;
#34000 = ORIENTED_EDGE ( 'NONE', *, *, #11960, .T. ) ;
#34001 = LINE ( 'NONE', #17482, #35662 ) ;
#34002 = EDGE_CURVE ( 'NONE', #33327, #7706, #10407, .T. ) ;
#34003 = LINE ( 'NONE', #22623, #1726 ) ;
#34004 = ORIENTED_EDGE ( 'NONE', *, *, #1271, .F. ) ;
#34005 = DIRECTION ( 'NONE',  ( 1.283101021437939896E-16, 1.000000000000000000, -1.154811821032073265E-17 ) ) ;
#34006 = VERTEX_POINT ( 'NONE', #29770 ) ;
#34007 = ORIENTED_EDGE ( 'NONE', *, *, #23002, .T. ) ;
#34008 = EDGE_CURVE ( 'NONE', #38652, #22332, #49559, .T. ) ;
#34009 = ADVANCED_FACE ( 'NONE', ( #10149 ), #46247, .F. ) ;
#34010 = EDGE_CURVE ( 'NONE', #38070, #6857, #29748, .T. ) ;
#34011 = ORIENTED_EDGE ( 'NONE', *, *, #1367, .F. ) ;
#34012 = ORIENTED_EDGE ( 'NONE', *, *, #34821, .F. ) ;
#34013 = CARTESIAN_POINT ( 'NONE',  ( 0.2156685157584260770, 1.624173731825095723, -2.945280361644574185 ) ) ;
#34014 = EDGE_LOOP ( 'NONE', ( #27905, #47951, #27806, #13730 ) ) ;
#34015 = CARTESIAN_POINT ( 'NONE',  ( -1.166969139818015977, 0.000000000000000000, 1.732283464566920950 ) ) ;
#34016 = DIRECTION ( 'NONE',  ( -3.986037398843765983E-20, -1.000000000000000000, -1.160734090543304660E-16 ) ) ;
#34017 = CIRCLE ( 'NONE', #20814, 2.165354330708661568 ) ;
#34018 = CARTESIAN_POINT ( 'NONE',  ( 2.491402175429654253, 0.000000000000000000, -1.585592796919505831 ) ) ;
#34019 = VECTOR ( 'NONE', #49187, 39.37007874015748143 ) ;
#34020 = LINE ( 'NONE', #41259, #49153 ) ;
#34021 = CARTESIAN_POINT ( 'NONE',  ( 1.905671854841463952, 1.748959039950288341, 2.256015092822681645 ) ) ;
#34022 = ORIENTED_EDGE ( 'NONE', *, *, #21569, .T. ) ;
#34023 = CARTESIAN_POINT ( 'NONE',  ( 1.560669927219590747, 0.000000000000000000, -0.1574803149606304187 ) ) ;
#34024 = CARTESIAN_POINT ( 'NONE',  ( 0.000000000000000000, 3.346456692913386100, 0.000000000000000000 ) ) ;
#34025 = VECTOR ( 'NONE', #28455, 39.37007874015748143 ) ;
#34026 = EDGE_CURVE ( 'NONE', #14063, #39780, #2658, .T. ) ;
#34027 = CARTESIAN_POINT ( 'NONE',  ( -1.636583440222564301, 0.000000000000000000, 1.574803149606291530 ) ) ;
#34028 = LINE ( 'NONE', #49716, #36372 ) ;
#34029 = AXIS2_PLACEMENT_3D ( 'NONE', #28981, #5502, #21248 ) ;
#34030 = VECTOR ( 'NONE', #5434, 39.37007874015748143 ) ;
#34031 = VERTEX_POINT ( 'NONE', #7040 ) ;
#34032 = DIRECTION ( 'NONE',  ( -0.000000000000000000, 1.000000000000000000, -0.000000000000000000 ) ) ;
#34033 = CARTESIAN_POINT ( 'NONE',  ( -1.740398808985498258, 1.907947403895145864E-05, 0.1027251841395684928 ) ) ;
#34034 = VERTEX_POINT ( 'NONE', #22787 ) ;
#34035 = LINE ( 'NONE', #41515, #41109 ) ;
#34036 = EDGE_CURVE ( 'NONE', #49090, #19294, #38538, .T. ) ;
#34037 = CARTESIAN_POINT ( 'NONE',  ( -2.122091976112999490, 1.205361022782829114E-17, 0.4338754535132819390 ) ) ;
#34038 = ADVANCED_FACE ( 'NONE', ( #15037 ), #30784, .F. ) ;
#34039 = EDGE_LOOP ( 'NONE', ( #36380, #14664, #6412, #45615 ) ) ;
#34040 = ADVANCED_FACE ( 'NONE', ( #8558 ), #48753, .T. ) ;
#34041 = EDGE_LOOP ( 'NONE', ( #29286, #49359, #2604, #17256 ) ) ;
#34042 = FACE_OUTER_BOUND ( 'NONE', #37833, .T. ) ;
#34043 = DIRECTION ( 'NONE',  ( -0.000000000000000000, 1.000000000000000000, -0.000000000000000000 ) ) ;
#34044 = CARTESIAN_POINT ( 'NONE',  ( 0.4696143004045478797, 3.267716535433071279, -0.9842519685039348154 ) ) ;
#34045 = CARTESIAN_POINT ( 'NONE',  ( 0.2508718039770792552, 1.711920121901901348, -2.238407143905190910 ) ) ;
#34046 = FACE_OUTER_BOUND ( 'NONE', #19852, .T. ) ;
#34047 = EDGE_LOOP ( 'NONE', ( #20989, #10152, #34169, #20559 ) ) ;
#34048 = DIRECTION ( 'NONE',  ( 1.734723475976806848E-16, -0.000000000000000000, 1.000000000000000000 ) ) ;
#34049 = ORIENTED_EDGE ( 'NONE', *, *, #37160, .T. ) ;
#34050 = ORIENTED_EDGE ( 'NONE', *, *, #43889, .F. ) ;
#34051 = CARTESIAN_POINT ( 'NONE',  ( -1.650279682448762886, 0.0005104048319611981764, 0.5879535613212861778 ) ) ;
#34052 = ORIENTED_EDGE ( 'NONE', *, *, #8616, .T. ) ;
#34053 = FACE_OUTER_BOUND ( 'NONE', #19405, .T. ) ;
#34054 = PLANE ( 'NONE',  #9556 ) ;
#34055 = ORIENTED_EDGE ( 'NONE', *, *, #17357, .T. ) ;
#34056 = DIRECTION ( 'NONE',  ( -3.981026654148454344E-17, 1.000000000000000000, -1.225234019452869602E-16 ) ) ;
#34057 = DIRECTION ( 'NONE',  ( 0.000000000000000000, 0.000000000000000000, 1.000000000000000000 ) ) ;
#34058 = AXIS2_PLACEMENT_3D ( 'NONE', #40159, #4781, #8907 ) ;
#34059 = DIRECTION ( 'NONE',  ( -0.7227948638273978821, -8.018518666443169432E-17, 0.6910626489868580968 ) ) ;
#34060 = ORIENTED_EDGE ( 'NONE', *, *, #18048, .T. ) ;
#34061 = ORIENTED_EDGE ( 'NONE', *, *, #28138, .T. ) ;
#34062 = FACE_OUTER_BOUND ( 'NONE', #40312, .T. ) ;
#34063 = FACE_BOUND ( 'NONE', #36344, .T. ) ;
#34064 = ORIENTED_EDGE ( 'NONE', *, *, #26390, .F. ) ;
#34065 = AXIS2_PLACEMENT_3D ( 'NONE', #12151, #20921, #25049 ) ;
#34066 = VECTOR ( 'NONE', #48764, 39.37007874015748143 ) ;
#34067 = DIRECTION ( 'NONE',  ( 0.000000000000000000, -1.000000000000000000, 0.000000000000000000 ) ) ;
#34068 = CARTESIAN_POINT ( 'NONE',  ( -0.5404877333192481537, 0.006475226164817101532, -1.773429173509019297 ) ) ;
#34069 = EDGE_CURVE ( 'NONE', #33511, #2264, #4279, .T. ) ;
#34070 = ORIENTED_EDGE ( 'NONE', *, *, #30981, .F. ) ;
#34071 = VERTEX_POINT ( 'NONE', #11417 ) ;
#34072 = DIRECTION ( 'NONE',  ( -0.000000000000000000, 1.000000000000000000, -0.000000000000000000 ) ) ;
#34073 = EDGE_CURVE ( 'NONE', #30262, #30424, #35420, .T. ) ;
#34074 = AXIS2_PLACEMENT_3D ( 'NONE', #48387, #13075, #44296 ) ;
#34075 = CARTESIAN_POINT ( 'NONE',  ( -1.405664884363581502, 1.586962458333645021, 1.683711065981816857 ) ) ;
#34076 = ORIENTED_EDGE ( 'NONE', *, *, #24693, .T. ) ;
#34077 = ORIENTED_EDGE ( 'NONE', *, *, #42210, .T. ) ;
#34078 = ORIENTED_EDGE ( 'NONE', *, *, #2397, .F. ) ;
#34079 = DIRECTION ( 'NONE',  ( -3.469446951953613696E-16, 0.000000000000000000, -1.000000000000000000 ) ) ;
#34080 = CARTESIAN_POINT ( 'NONE',  ( -2.182111253630085290, 3.267716535433071279, -0.3149606299212589500 ) ) ;
#34081 = DIRECTION ( 'NONE',  ( 1.000000000000000000, 0.000000000000000000, -3.469446951953613696E-16 ) ) ;
#34082 = DIRECTION ( 'NONE',  ( 1.000000000000000000, 0.000000000000000000, -3.469446951953613696E-16 ) ) ;
#34083 = ORIENTED_EDGE ( 'NONE', *, *, #1975, .T. ) ;
#34084 = ORIENTED_EDGE ( 'NONE', *, *, #31225, .F. ) ;
#34085 = DIRECTION ( 'NONE',  ( -0.000000000000000000, -1.000000000000000000, -0.000000000000000000 ) ) ;
#34086 = DIRECTION ( 'NONE',  ( 1.000000000000000000, 0.000000000000000000, 0.000000000000000000 ) ) ;
#34087 = CARTESIAN_POINT ( 'NONE',  ( 1.181102362204724310, 0.000000000000000000, -1.181102362204724754 ) ) ;
#34088 = EDGE_CURVE ( 'NONE', #50026, #49624, #35928, .T. ) ;
#34089 = CARTESIAN_POINT ( 'NONE',  ( 3.927031490892378253E-16, 3.346456692913386100, 2.007874015748021268 ) ) ;
#34090 = CARTESIAN_POINT ( 'NONE',  ( 3.927031490892378253E-16, 0.000000000000000000, 0.7480314960629874665 ) ) ;
#34091 = EDGE_CURVE ( 'NONE', #8095, #39490, #31295, .T. ) ;
#34092 = PLANE ( 'NONE',  #3672 ) ;
#34093 = FACE_OUTER_BOUND ( 'NONE', #30551, .T. ) ;
#34094 = EDGE_CURVE ( 'NONE', #11610, #24163, #3319, .T. ) ;
#34095 = CIRCLE ( 'NONE', #48044, 2.165354330708661568 ) ;
#34096 = ORIENTED_EDGE ( 'NONE', *, *, #34131, .F. ) ;
#34097 = CARTESIAN_POINT ( 'NONE',  ( 2.947574761915768171, 2.755905511811027164, -0.1816379373804909991 ) ) ;
#34098 = CARTESIAN_POINT ( 'NONE',  ( 2.106197740627111514, 0.000000000000000000, -1.299212598425194320 ) ) ;
#34099 = ADVANCED_FACE ( 'NONE', ( #42890 ), #15288, .F. ) ;
#34100 = VECTOR ( 'NONE', #32908, 39.37007874015748143 ) ;
#34101 = ORIENTED_EDGE ( 'NONE', *, *, #11410, .F. ) ;
#34102 = VECTOR ( 'NONE', #13291, 39.37007874015748143 ) ;
#34103 = VERTEX_POINT ( 'NONE', #46742 ) ;
#34104 = VECTOR ( 'NONE', #29245, 39.37007874015748143 ) ;
#34105 = CARTESIAN_POINT ( 'NONE',  ( 0.000000000000000000, 3.267716535433071279, 0.000000000000000000 ) ) ;
#34106 = VERTEX_POINT ( 'NONE', #35164 ) ;
#34107 = AXIS2_PLACEMENT_3D ( 'NONE', #30532, #42138, #34407 ) ;
#34108 = ORIENTED_EDGE ( 'NONE', *, *, #12475, .T. ) ;
#34109 = LINE ( 'NONE', #2860, #12230 ) ;
#34110 = VERTEX_POINT ( 'NONE', #19901 ) ;
#34111 = CARTESIAN_POINT ( 'NONE',  ( -2.100190309385016274, 0.000000000000000000, 0.5298329251847215815 ) ) ;
#34112 = LINE ( 'NONE', #2863, #22269 ) ;
#34113 = ORIENTED_EDGE ( 'NONE', *, *, #17639, .T. ) ;
#34114 = VERTEX_POINT ( 'NONE', #46987 ) ;
#34115 = LINE ( 'NONE', #37487, #10677 ) ;
#34116 = VERTEX_POINT ( 'NONE', #7539 ) ;
#34117 = ORIENTED_EDGE ( 'NONE', *, *, #49110, .F. ) ;
#34118 = CARTESIAN_POINT ( 'NONE',  ( 0.000000000000000000, 3.267716535433071279, 1.889763779527550369 ) ) ;
#34119 = CARTESIAN_POINT ( 'NONE',  ( -1.909347346926324462, 3.267716535433071279, 0.7874015748031456541 ) ) ;
#34120 = DIRECTION ( 'NONE',  ( -0.01601477604151182663, 0.9998717552508123996, -0.000000000000000000 ) ) ;
#34121 = DIRECTION ( 'NONE',  ( -1.000000000000000000, 0.000000000000000000, 0.000000000000000000 ) ) ;
#34122 = EDGE_LOOP ( 'NONE', ( #49003, #50044, #20437, #2650 ) ) ;
#34123 = LINE ( 'NONE', #38002, #37866 ) ;
#34124 = DIRECTION ( 'NONE',  ( -1.000000000000000000, -0.000000000000000000, -0.000000000000000000 ) ) ;
#34125 = CARTESIAN_POINT ( 'NONE',  ( -1.743516651958532115, 0.0004834999639498254787, -0.009673880220434260407 ) ) ;
#34126 = ORIENTED_EDGE ( 'NONE', *, *, #43731, .F. ) ;
#34127 = FACE_OUTER_BOUND ( 'NONE', #26049, .T. ) ;
#34128 = VECTOR ( 'NONE', #10193, 39.37007874015748143 ) ;
#34129 = LINE ( 'NONE', #2121, #24405 ) ;
#34130 = ADVANCED_FACE ( 'NONE', ( #43142 ), #28163, .F. ) ;
#34131 = EDGE_CURVE ( 'NONE', #35860, #23592, #39797, .T. ) ;
#34132 = ORIENTED_EDGE ( 'NONE', *, *, #49581, .F. ) ;
#34133 = AXIS2_PLACEMENT_3D ( 'NONE', #30923, #3551, #8191 ) ;
#34134 = VERTEX_POINT ( 'NONE', #24308 ) ;
#34135 = CARTESIAN_POINT ( 'NONE',  ( -1.528563137326103050, 27.09235863320434134, 73.21064473650069715 ) ) ;
#34136 = EDGE_CURVE ( 'NONE', #12204, #24976, #4427, .T. ) ;
#34137 = AXIS2_PLACEMENT_3D ( 'NONE', #10172, #25922, #41670 ) ;
#34138 = VECTOR ( 'NONE', #24038, 39.37007874015748143 ) ;
#34139 = B_SPLINE_CURVE_WITH_KNOTS ( 'NONE', 3,
 ( #30914, #47375, #39417, #3545 ),
 .UNSPECIFIED., .F., .F.,
 ( 4, 4 ),
 ( 0.01440155393167629264, 0.03074911278961747763 ),
 .UNSPECIFIED. ) ;
#34140 = LINE ( 'NONE', #41370, #22300 ) ;
#34141 = CARTESIAN_POINT ( 'NONE',  ( 1.388309139374679146, 1.631713065620022274, -1.827118126197171399 ) ) ;
#34142 = ADVANCED_FACE ( 'NONE', ( #7791 ), #39033, .F. ) ;
#34143 = FACE_OUTER_BOUND ( 'NONE', #28171, .T. ) ;
#34144 = ORIENTED_EDGE ( 'NONE', *, *, #32305, .T. ) ;
#34145 = VERTEX_POINT ( 'NONE', #47501 ) ;
#34146 = AXIS2_PLACEMENT_3D ( 'NONE', #10089, #25830, #29453 ) ;
#34147 = PLANE ( 'NONE',  #19702 ) ;
#34148 = CARTESIAN_POINT ( 'NONE',  ( 2.695799277629594037, 1.662794757381320654, -1.205759334241453651 ) ) ;
#34149 = VERTEX_POINT ( 'NONE', #3921 ) ;
#34150 = CARTESIAN_POINT ( 'NONE',  ( 1.287906020515829919, 0.000000000000000000, -1.574803149606294417 ) ) ;
#34151 = CARTESIAN_POINT ( 'NONE',  ( -0.3486774197067334935, 3.346456692913386100, 0.4330708661417290162 ) ) ;
#34152 = EDGE_CURVE ( 'NONE', #50816, #31303, #16045, .T. ) ;
#34153 = CARTESIAN_POINT ( 'NONE',  ( 0.08139965876239094178, 1.610780518492231694, 0.000000000000000000 ) ) ;
#34154 = CARTESIAN_POINT ( 'NONE',  ( 0.1067246931122726866, 0.02962905676920215767, 0.000000000000000000 ) ) ;
#34155 = CARTESIAN_POINT ( 'NONE',  ( -1.712499999658713801, 0.5249316497054298258, -0.7854770530685656338 ) ) ;
#34156 = ORIENTED_EDGE ( 'NONE', *, *, #38686, .F. ) ;
#34157 = CARTESIAN_POINT ( 'NONE',  ( 2.080833746290526420, 1.646223005948175278, -1.432513710245896243 ) ) ;
#34158 = DIRECTION ( 'NONE',  ( -3.469446951953613696E-16, 0.000000000000000000, -1.000000000000000000 ) ) ;
#34159 = EDGE_CURVE ( 'NONE', #36331, #50486, #12571, .T. ) ;
#34160 = PLANE ( 'NONE',  #983 ) ;
#34161 = ORIENTED_EDGE ( 'NONE', *, *, #11098, .T. ) ;
#34162 = CARTESIAN_POINT ( 'NONE',  ( 1.636583440222563635, 0.000000000000000000, -1.259842519685035800 ) ) ;
#34163 = CARTESIAN_POINT ( 'NONE',  ( -1.645894780863148332, 0.6447981115998611124, -0.5410498576272523286 ) ) ;
#34164 = FACE_OUTER_BOUND ( 'NONE', #28456, .T. ) ;
#34165 = VERTEX_POINT ( 'NONE', #47755 ) ;
#34166 = PLANE ( 'NONE',  #22591 ) ;
#34167 = AXIS2_PLACEMENT_3D ( 'NONE', #11387, #30257, #42866 ) ;
#34168 = VECTOR ( 'NONE', #12543, 39.37007874015748854 ) ;
#34169 = ORIENTED_EDGE ( 'NONE', *, *, #5915, .F. ) ;
#34170 = CIRCLE ( 'NONE', #11884, 2.106299212598425008 ) ;
#34171 = LINE ( 'NONE', #30032, #33774 ) ;
#34172 = ORIENTED_EDGE ( 'NONE', *, *, #25080, .F. ) ;
#34173 = DIRECTION ( 'NONE',  ( -0.3513748240813305279, 0.000000000000000000, -0.9362348706397418674 ) ) ;
#34174 = EDGE_CURVE ( 'NONE', #7950, #3576, #43654, .T. ) ;
#34175 = AXIS2_PLACEMENT_3D ( 'NONE', #13149, #9015, #1006 ) ;
#34176 = VECTOR ( 'NONE', #32510, 39.37007874015748143 ) ;
#34177 = LINE ( 'NONE', #7553, #12832 ) ;
#34178 = CARTESIAN_POINT ( 'NONE',  ( -1.068402561569949061, 5.905511811023623991, -1.884154513482187765 ) ) ;
#34179 = FACE_OUTER_BOUND ( 'NONE', #36, .T. ) ;
#34180 = EDGE_LOOP ( 'NONE', ( #2169, #2130, #2527 ) ) ;
#34181 = ORIENTED_EDGE ( 'NONE', *, *, #38026, .T. ) ;
#34182 = CARTESIAN_POINT ( 'NONE',  ( 1.833433833923350686, 3.267716535433071279, -6.361001426713997494E-16 ) ) ;
#34183 = VECTOR ( 'NONE', #20878, 39.37007874015748143 ) ;
#34184 = CARTESIAN_POINT ( 'NONE',  ( 0.5455278134075212115, 3.267716535433071279, -0.9448818897637765168 ) ) ;
#34185 = ORIENTED_EDGE ( 'NONE', *, *, #34488, .T. ) ;
#34186 = CARTESIAN_POINT ( 'NONE',  ( -1.217747569163365018, 1.597917297168418793, -2.415255414932540479 ) ) ;
#34187 = DIRECTION ( 'NONE',  ( 3.986037398843765983E-20, 1.000000000000000000, 1.160734090543304660E-16 ) ) ;
#34188 = DIRECTION ( 'NONE',  ( -1.000000000000000000, 0.000000000000000000, 0.000000000000000000 ) ) ;
#34189 = ORIENTED_EDGE ( 'NONE', *, *, #8007, .T. ) ;
#34190 = ORIENTED_EDGE ( 'NONE', *, *, #23102, .F. ) ;
#34191 = FACE_OUTER_BOUND ( 'NONE', #48470, .T. ) ;
#34192 = CARTESIAN_POINT ( 'NONE',  ( 0.5455278134075212115, 0.000000000000000000, -6.146657985744592735E-16 ) ) ;
#34193 = DIRECTION ( 'NONE',  ( -1.000000000000000000, 0.000000000000000000, -0.000000000000000000 ) ) ;
#34194 = ORIENTED_EDGE ( 'NONE', *, *, #22085, .T. ) ;
#34195 = SURFACE_STYLE_FILL_AREA ( #6575 ) ;
#34196 = DIRECTION ( 'NONE',  ( 0.000000000000000000, 1.000000000000000000, 0.000000000000000000 ) ) ;
#34197 = ORIENTED_EDGE ( 'NONE', *, *, #42017, .T. ) ;
#34198 = ADVANCED_FACE ( 'NONE', ( #43909 ), #12170, .F. ) ;
#34199 = LINE ( 'NONE', #17683, #993 ) ;
#34200 = VERTEX_POINT ( 'NONE', #25582 ) ;
#34201 = VERTEX_POINT ( 'NONE', #33093 ) ;
#34202 = LINE ( 'NONE', #21816, #19615 ) ;
#34203 = CARTESIAN_POINT ( 'NONE',  ( -1.985260859929297572, 3.346456692913386100, 0.3149606299212578953 ) ) ;
#34204 = EDGE_CURVE ( 'NONE', #28082, #50303, #21205, .T. ) ;
#34205 = LINE ( 'NONE', #32752, #24764 ) ;
#34206 = EDGE_CURVE ( 'NONE', #36591, #14599, #32578, .T. ) ;
#34207 = CARTESIAN_POINT ( 'NONE',  ( 0.000000000000000000, 0.000000000000000000, 0.000000000000000000 ) ) ;
#34208 = ADVANCED_FACE ( 'NONE', ( #1582 ), #36189, .F. ) ;
#34209 = CARTESIAN_POINT ( 'NONE',  ( -0.8942052331142552601, 3.267716535433071279, -1.771653543307081025 ) ) ;
#34210 = ORIENTED_EDGE ( 'NONE', *, *, #39189, .F. ) ;
#34211 = VECTOR ( 'NONE', #19454, 39.37007874015748143 ) ;
#34212 = CIRCLE ( 'NONE', #16051, 2.244934639244525076 ) ;
#34213 = ORIENTED_EDGE ( 'NONE', *, *, #47854, .T. ) ;
#34214 = LINE ( 'NONE', #34464, #40131 ) ;
#34215 = DIRECTION ( 'NONE',  ( 1.734723475976806848E-16, -0.000000000000000000, 1.000000000000000000 ) ) ;
#34216 = VECTOR ( 'NONE', #48345, 39.37007874015748143 ) ;
#34217 = ADVANCED_FACE ( 'NONE', ( #5714 ), #9841, .F. ) ;
#34218 = DIRECTION ( 'NONE',  ( -1.000000000000000000, 0.000000000000000000, -0.000000000000000000 ) ) ;
#34219 = CARTESIAN_POINT ( 'NONE',  ( -1.363819533518803029, 3.346456692913386100, 1.417322834645662777 ) ) ;
#34220 = LINE ( 'NONE', #41205, #32830 ) ;
#34221 = AXIS2_PLACEMENT_3D ( 'NONE', #44313, #37098, #21090 ) ;
#34222 = ORIENTED_EDGE ( 'NONE', *, *, #47263, .F. ) ;
#34223 = DIRECTION ( 'NONE',  ( -0.01601477604151182663, 0.9998717552508123996, -0.000000000000000000 ) ) ;
#34224 = EDGE_CURVE ( 'NONE', #35324, #13112, #4942, .T. ) ;
#34225 = LINE ( 'NONE', #38350, #14955 ) ;
#34226 = ORIENTED_EDGE ( 'NONE', *, *, #22487, .T. ) ;
#34227 = CARTESIAN_POINT ( 'NONE',  ( 0.000000000000000000, 3.267716535433071279, 0.9055118110236167750 ) ) ;
#34228 = DIRECTION ( 'NONE',  ( 0.000000000000000000, -1.000000000000000000, 0.000000000000000000 ) ) ;
#34229 = VERTEX_POINT ( 'NONE', #21460 ) ;
#34230 = CARTESIAN_POINT ( 'NONE',  ( -0.6866523217321213179, 0.01134346163807614834, 1.689521298909904212 ) ) ;
#34231 = EDGE_CURVE ( 'NONE', #31088, #38922, #17335, .T. ) ;
#34232 = DIRECTION ( 'NONE',  ( 0.000000000000000000, 1.000000000000000000, 0.000000000000000000 ) ) ;
#34233 = DIRECTION ( 'NONE',  ( -3.469446951953613696E-16, 0.000000000000000000, -1.000000000000000000 ) ) ;
#34234 = ORIENTED_EDGE ( 'NONE', *, *, #35985, .T. ) ;
#34235 = CARTESIAN_POINT ( 'NONE',  ( -0.5455278134075211005, 3.267716535433071279, 9.463399047163218249E-17 ) ) ;
#34236 = ORIENTED_EDGE ( 'NONE', *, *, #629, .T. ) ;
#34237 = FACE_BOUND ( 'NONE', #21619, .T. ) ;
#34238 = EDGE_CURVE ( 'NONE', #31389, #19986, #1322, .T. ) ;
#34239 = DIRECTION ( 'NONE',  ( -0.9998717552508122886, -0.01601477604151185785, 0.000000000000000000 ) ) ;
#34240 = CARTESIAN_POINT ( 'NONE',  ( 0.000000000000000000, 3.267716535433071279, -1.102362204724405492 ) ) ;
#34241 = CARTESIAN_POINT ( 'NONE',  ( 1.833433833923351353, 0.000000000000000000, -0.9448818897637765168 ) ) ;
#34242 = EDGE_LOOP ( 'NONE', ( #45656, #22458, #1732, #41473 ) ) ;
#34243 = ORIENTED_EDGE ( 'NONE', *, *, #14336, .F. ) ;
#34244 = DIRECTION ( 'NONE',  ( 1.734723475976806848E-16, -0.000000000000000000, 1.000000000000000000 ) ) ;
#34245 = VECTOR ( 'NONE', #22462, 39.37007874015748143 ) ;
#34246 = CYLINDRICAL_SURFACE ( 'NONE', #720, 1.181102362204723200 ) ;
#34247 = VECTOR ( 'NONE', #4901, 39.37007874015748143 ) ;
#34248 = ADVANCED_FACE ( 'NONE', ( #5453 ), #20679, .F. ) ;
#34249 = CIRCLE ( 'NONE', #16926, 2.106299212598425008 ) ;
#34250 = LINE ( 'NONE', #8766, #8728 ) ;
#34251 = FACE_OUTER_BOUND ( 'NONE', #20767, .T. ) ;
#34252 = ADVANCED_FACE ( 'NONE', ( #16823 ), #44429, .F. ) ;
#34253 = DIRECTION ( 'NONE',  ( -0.000000000000000000, 1.000000000000000000, -0.000000000000000000 ) ) ;
#34254 = ORIENTED_EDGE ( 'NONE', *, *, #792, .F. ) ;
#34255 = VERTEX_POINT ( 'NONE', #33350 ) ;
#34256 = CARTESIAN_POINT ( 'NONE',  ( -2.182111253630085290, 0.000000000000000000, 0.7480314960629874665 ) ) ;
#34257 = LINE ( 'NONE', #17737, #49514 ) ;
#34258 = VECTOR ( 'NONE', #49674, 39.37007874015748143 ) ;
#34259 = VERTEX_POINT ( 'NONE', #13460 ) ;
#34260 = CARTESIAN_POINT ( 'NONE',  ( 1.287906020515830141, 3.346456692913386100, -0.3149606299212596716 ) ) ;
#34261 = ORIENTED_EDGE ( 'NONE', *, *, #45704, .T. ) ;
#34262 = ORIENTED_EDGE ( 'NONE', *, *, #32043, .T. ) ;
#34263 = EDGE_CURVE ( 'NONE', #30628, #24596, #9583, .T. ) ;
#34264 = ORIENTED_EDGE ( 'NONE', *, *, #38565, .F. ) ;
#34265 = ORIENTED_EDGE ( 'NONE', *, *, #47915, .F. ) ;
#34266 = DIRECTION ( 'NONE',  ( -0.000000000000000000, 1.000000000000000000, -0.000000000000000000 ) ) ;
#34267 = EDGE_CURVE ( 'NONE', #8712, #47418, #49028, .T. ) ;
#34268 = ORIENTED_EDGE ( 'NONE', *, *, #50916, .F. ) ;
#34269 = CARTESIAN_POINT ( 'NONE',  ( -1.985260859929297572, 0.000000000000000000, 0.6299212598425164567 ) ) ;
#34270 = LINE ( 'NONE', #22893, #29365 ) ;
#34271 = CARTESIAN_POINT ( 'NONE',  ( -0.8182917201112814842, 3.346456692913386100, 0.4724409448818872592 ) ) ;
#34272 = CARTESIAN_POINT ( 'NONE',  ( -0.5442969769572160166, 1.633567243362389565, -2.157199947919104854 ) ) ;
#34273 = CARTESIAN_POINT ( 'NONE',  ( -0.2727639067037611054, 3.346456692913386100, -2.148105963102950877 ) ) ;
#34274 = VECTOR ( 'NONE', #7912, 39.37007874015748143 ) ;
#34275 = VERTEX_POINT ( 'NONE', #8812 ) ;
#34276 = FACE_OUTER_BOUND ( 'NONE', #30106, .T. ) ;
#34277 = DIRECTION ( 'NONE',  ( 0.000000000000000000, -1.000000000000000000, 0.000000000000000000 ) ) ;
#34278 = VECTOR ( 'NONE', #29066, 39.37007874015748143 ) ;
#34279 = CARTESIAN_POINT ( 'NONE',  ( 1.836694934015037806, 1.638894784719147513, 1.401770057403159520 ) ) ;
#34280 = VECTOR ( 'NONE', #42159, 39.37007874015748143 ) ;
#34281 = CARTESIAN_POINT ( 'NONE',  ( 1.602753508900452317, 0.000000000000000000, 1.341098548255033496 ) ) ;
#34282 = ORIENTED_EDGE ( 'NONE', *, *, #16836, .T. ) ;
#34283 = LINE ( 'NONE', #18780, #25654 ) ;
#34284 = CARTESIAN_POINT ( 'NONE',  ( -0.8182917201112819283, 3.346456692913386100, 2.004783788421104163 ) ) ;
#34285 = ORIENTED_EDGE ( 'NONE', *, *, #36148, .T. ) ;
#34286 = FACE_OUTER_BOUND ( 'NONE', #45071, .T. ) ;
#34287 = VECTOR ( 'NONE', #38503, 39.37007874015748143 ) ;
#34288 = EDGE_CURVE ( 'NONE', #33634, #6021, #45177, .T. ) ;
#34289 = FACE_OUTER_BOUND ( 'NONE', #31276, .T. ) ;
#34290 = VECTOR ( 'NONE', #17788, 39.37007874015748143 ) ;
#34291 = ORIENTED_EDGE ( 'NONE', *, *, #17652, .T. ) ;
#34292 = B_SPLINE_CURVE_WITH_KNOTS ( 'NONE', 3,
 ( #20187, #35954, #28189, #47776 ),
 .UNSPECIFIED., .F., .F.,
 ( 4, 4 ),
 ( 0.0001278591145448624699, 0.05010727685611865434 ),
 .UNSPECIFIED. ) ;
#34293 = DIRECTION ( 'NONE',  ( -0.000000000000000000, 1.000000000000000000, -0.000000000000000000 ) ) ;
#34294 = EDGE_LOOP ( 'NONE', ( #25368, #7764, #34897, #32276 ) ) ;
#34295 = CARTESIAN_POINT ( 'NONE',  ( -1.909347346926324684, 3.267716535433071279, 3.312189666507128175E-16 ) ) ;
#34296 = EDGE_CURVE ( 'NONE', #13472, #18093, #26569, .T. ) ;
#34297 = CARTESIAN_POINT ( 'NONE',  ( -1.546905380132658436, 1.650317032603659140, -1.547079516075193117 ) ) ;
#34298 = CARTESIAN_POINT ( 'NONE',  ( -0.8182917201112814842, 0.000000000000000000, 0.7874015748031456541 ) ) ;
#34299 = EDGE_CURVE ( 'NONE', #22884, #41400, #9352, .T. ) ;
#34300 = LINE ( 'NONE', #35050, #32551 ) ;
#34301 = CARTESIAN_POINT ( 'NONE',  ( 1.825231763105664928, 0.5249316475426857309, -0.4670754312686604681 ) ) ;
#34302 = ORIENTED_EDGE ( 'NONE', *, *, #39734, .F. ) ;
#34303 = EDGE_CURVE ( 'NONE', #4450, #12364, #48522, .T. ) ;
#34304 = CARTESIAN_POINT ( 'NONE',  ( 0.07982360342473591996, 1.709180471932028711, 0.000000000000000000 ) ) ;
#34305 = ORIENTED_EDGE ( 'NONE', *, *, #24100, .F. ) ;
#34306 = ORIENTED_EDGE ( 'NONE', *, *, #8664, .T. ) ;
#34307 = CARTESIAN_POINT ( 'NONE',  ( -1.909347346926324684, 3.267716535433071279, 3.312189666507128175E-16 ) ) ;
#34308 = ORIENTED_EDGE ( 'NONE', *, *, #49898, .T. ) ;
#34309 = EDGE_CURVE ( 'NONE', #28890, #33278, #32841, .T. ) ;
#34310 = CARTESIAN_POINT ( 'NONE',  ( 1.833433833923351353, 3.346456692913386100, -0.3149606299212596716 ) ) ;
#34311 = DIRECTION ( 'NONE',  ( 0.000000000000000000, 1.000000000000000000, 0.000000000000000000 ) ) ;
#34312 = ORIENTED_EDGE ( 'NONE', *, *, #28167, .T. ) ;
#34313 = DIRECTION ( 'NONE',  ( 1.734723475976806848E-16, -0.000000000000000000, 1.000000000000000000 ) ) ;
#34314 = CARTESIAN_POINT ( 'NONE',  ( 1.363819533518803251, 3.267716535433071279, -2.365849761790805487E-16 ) ) ;
#34315 = AXIS2_PLACEMENT_3D ( 'NONE', #25631, #44480, #10141 ) ;
#34316 = DIRECTION ( 'NONE',  ( 1.000000000000000000, 0.000000000000000000, 0.000000000000000000 ) ) ;
#34317 = VECTOR ( 'NONE', #7788, 39.37007874015748143 ) ;
#34318 = EDGE_LOOP ( 'NONE', ( #22848, #35906, #33969, #5553 ) ) ;
#34319 = ORIENTED_EDGE ( 'NONE', *, *, #7655, .F. ) ;
#34320 = VECTOR ( 'NONE', #6133, 39.37007874015748143 ) ;
#34321 = PLANE ( 'NONE',  #24880 ) ;
#34322 = FACE_BOUND ( 'NONE', #26124, .T. ) ;
#34323 = ORIENTED_EDGE ( 'NONE', *, *, #48266, .F. ) ;
#34324 = VECTOR ( 'NONE', #31900, 39.37007874015748143 ) ;
#34325 = ADVANCED_FACE ( 'NONE', ( #19532 ), #18789, .F. ) ;
#34326 = DIRECTION ( 'NONE',  ( 0.000000000000000000, 1.160734090543304660E-16, -1.000000000000000000 ) ) ;
#34327 = DIRECTION ( 'NONE',  ( -3.469446951953613696E-16, 0.000000000000000000, -1.000000000000000000 ) ) ;
#34328 = VECTOR ( 'NONE', #26372, 39.37007874015748143 ) ;
#34329 = ORIENTED_EDGE ( 'NONE', *, *, #32399, .T. ) ;
#34330 = EDGE_LOOP ( 'NONE', ( #19088, #50504, #34012, #24637 ) ) ;
#34331 = EDGE_CURVE ( 'NONE', #8583, #35716, #6911, .T. ) ;
#34332 = LINE ( 'NONE', #50016, #26481 ) ;
#34333 = VECTOR ( 'NONE', #9477, 39.37007874015748143 ) ;
#34334 = CARTESIAN_POINT ( 'NONE',  ( 1.091055626815042645, 3.267716535433071279, -1.892679809432644389E-16 ) ) ;
#34335 = ORIENTED_EDGE ( 'NONE', *, *, #17058, .F. ) ;
#34336 = ORIENTED_EDGE ( 'NONE', *, *, #21580, .T. ) ;
#34337 = CARTESIAN_POINT ( 'NONE',  ( -2.100227814008681637, 1.559371130916006543, -2.076109931251943319 ) ) ;
#34338 = DIRECTION ( 'NONE',  ( 1.734723475976806848E-16, 0.000000000000000000, 1.000000000000000000 ) ) ;
#34339 = CARTESIAN_POINT ( 'NONE',  ( -0.2727639067037605503, 3.267716535433071279, 4.731699523581609741E-17 ) ) ;
#34340 = VERTEX_POINT ( 'NONE', #14663 ) ;
#34341 = EDGE_LOOP ( 'NONE', ( #35428, #8886, #32662, #17588 ) ) ;
#34342 = CARTESIAN_POINT ( 'NONE',  ( 0.4696143004045476022, 3.346456692913386100, -2.113816876263008293 ) ) ;
#34343 = CARTESIAN_POINT ( 'NONE',  ( 4.200216290258821831E-16, 3.346456692913386100, 2.165354330708661568 ) ) ;
#34344 = CARTESIAN_POINT ( 'NONE',  ( 2.074656761899007051, 6.692913385826772199, -0.6223516566630626912 ) ) ;
#34345 = FACE_OUTER_BOUND ( 'NONE', #34047, .T. ) ;
#34346 = CARTESIAN_POINT ( 'NONE',  ( 1.062992125984251413, 0.000000000000000000, -1.181102362204724754 ) ) ;
#34347 = CARTESIAN_POINT ( 'NONE',  ( 0.000000000000000000, 3.267716535433071279, 0.000000000000000000 ) ) ;
#34348 = VECTOR ( 'NONE', #37656, 39.37007874015748143 ) ;
#34349 = DIRECTION ( 'NONE',  ( -0.000000000000000000, 1.000000000000000000, -0.000000000000000000 ) ) ;
#34350 = ORIENTED_EDGE ( 'NONE', *, *, #18872, .T. ) ;
#34351 = VECTOR ( 'NONE', #33512, 39.37007874015748143 ) ;
#34352 = LINE ( 'NONE', #18600, #39919 ) ;
#34353 = DIRECTION ( 'NONE',  ( -1.000000000000000000, 0.000000000000000000, 0.000000000000000000 ) ) ;
#34354 = VECTOR ( 'NONE', #22083, 39.37007874015748143 ) ;
#34355 = ORIENTED_EDGE ( 'NONE', *, *, #22227, .F. ) ;
#34356 = VECTOR ( 'NONE', #14048, 39.37007874015748143 ) ;
#34357 = ORIENTED_EDGE ( 'NONE', *, *, #15377, .T. ) ;
#34358 = CARTESIAN_POINT ( 'NONE',  ( -1.166969139818015977, 3.346456692913386100, -0.4724409448818886470 ) ) ;
#34359 = DIRECTION ( 'NONE',  ( -0.000000000000000000, 0.000000000000000000, 1.000000000000000000 ) ) ;
#34360 = EDGE_CURVE ( 'NONE', #49094, #1746, #6662, .T. ) ;
#34361 = ORIENTED_EDGE ( 'NONE', *, *, #9108, .F. ) ;
#34362 = EDGE_CURVE ( 'NONE', #11498, #31195, #3287, .T. ) ;
#34363 = EDGE_CURVE ( 'NONE', #11539, #49795, #3224, .T. ) ;
#34364 = AXIS2_PLACEMENT_3D ( 'NONE', #42422, #15062, #46768 ) ;
#34365 = VERTEX_POINT ( 'NONE', #38416 ) ;
#34366 = DIRECTION ( 'NONE',  ( -0.000000000000000000, 1.000000000000000000, -0.000000000000000000 ) ) ;
#34367 = VERTEX_POINT ( 'NONE', #38914 ) ;
#34368 = DIRECTION ( 'NONE',  ( 0.000000000000000000, -1.000000000000000000, 0.000000000000000000 ) ) ;
#34369 = DIRECTION ( 'NONE',  ( 1.000000000000000000, 0.000000000000000000, 0.000000000000000000 ) ) ;
#34370 = VERTEX_POINT ( 'NONE', #3548 ) ;
#34371 = CARTESIAN_POINT ( 'NONE',  ( 0.000000000000000000, 0.07874015748031502893, 1.682967650661292502 ) ) ;
#34372 = ORIENTED_EDGE ( 'NONE', *, *, #7966, .F. ) ;
#34373 = EDGE_LOOP ( 'NONE', ( #29539, #10382, #21300, #5043 ) ) ;
#34374 = CARTESIAN_POINT ( 'NONE',  ( 1.363819533518803251, 3.346456692913386100, 0.2755905511810996522 ) ) ;
#34375 = DIRECTION ( 'NONE',  ( 1.734723475976806848E-16, 0.000000000000000000, 1.000000000000000000 ) ) ;
#34376 = CARTESIAN_POINT ( 'NONE',  ( 2.182111253630085290, 3.267716535433071279, -3.785359618865289765E-16 ) ) ;
#34377 = PLANE ( 'NONE',  #4604 ) ;
#34378 = EDGE_CURVE ( 'NONE', #35330, #15755, #3040, .T. ) ;
#34379 = ORIENTED_EDGE ( 'NONE', *, *, #34238, .F. ) ;
#34380 = EDGE_CURVE ( 'NONE', #43136, #39958, #14915, .T. ) ;
#34381 = DIRECTION ( 'NONE',  ( -0.000000000000000000, 0.000000000000000000, 1.000000000000000000 ) ) ;
#34382 = CARTESIAN_POINT ( 'NONE',  ( -1.583112249919712999, 0.000000000000000000, -0.7301740747847248469 ) ) ;
#34383 = DIRECTION ( 'NONE',  ( 0.000000000000000000, -1.000000000000000000, 0.000000000000000000 ) ) ;
#34384 = VECTOR ( 'NONE', #21774, 39.37007874015748143 ) ;
#34385 = ORIENTED_EDGE ( 'NONE', *, *, #33266, .T. ) ;
#34386 = EDGE_CURVE ( 'NONE', #27803, #13111, #42272, .T. ) ;
#34387 = DIRECTION ( 'NONE',  ( -0.000000000000000000, 1.000000000000000000, -0.000000000000000000 ) ) ;
#34388 = CIRCLE ( 'NONE', #40989, 2.164630168518208109 ) ;
#34389 = EDGE_CURVE ( 'NONE', #20810, #35404, #46626, .T. ) ;
#34390 = ORIENTED_EDGE ( 'NONE', *, *, #45852, .F. ) ;
#34391 = ORIENTED_EDGE ( 'NONE', *, *, #22658, .T. ) ;
#34392 = DIRECTION ( 'NONE',  ( 1.734723475976806848E-16, -0.000000000000000000, 1.000000000000000000 ) ) ;
#34393 = VECTOR ( 'NONE', #12152, 39.37007874015748143 ) ;
#34394 = CARTESIAN_POINT ( 'NONE',  ( 1.363819533518803251, 3.346456692913386100, 1.417322834645662777 ) ) ;
#34395 = CARTESIAN_POINT ( 'NONE',  ( 2.988781320759228421, 2.755905511811027164, -0.1748580315756570747 ) ) ;
#34396 = VERTEX_POINT ( 'NONE', #38668 ) ;
#34397 = ORIENTED_EDGE ( 'NONE', *, *, #16722, .F. ) ;
#34398 =( NAMED_UNIT ( * ) PLANE_ANGLE_UNIT ( ) SI_UNIT ( $, .RADIAN. ) );
#34399 = LINE ( 'NONE', #14010, #49806 ) ;
#34400 = ORIENTED_EDGE ( 'NONE', *, *, #104, .T. ) ;
#34401 = CARTESIAN_POINT ( 'NONE',  ( 0.000000000000000000, 3.267716535433071279, 0.000000000000000000 ) ) ;
#34402 = CARTESIAN_POINT ( 'NONE',  ( -0.8182917201112814842, 3.346456692913386100, 1.417322834645662777 ) ) ;
#34403 = CARTESIAN_POINT ( 'NONE',  ( 0.3015460593140593115, 0.000000000000000000, 1.937268728265797213 ) ) ;
#34404 = CARTESIAN_POINT ( 'NONE',  ( -2.454875160333845674, 3.346456692913386100, -0.03937007874015881204 ) ) ;
#34405 = CARTESIAN_POINT ( 'NONE',  ( -1.522953965282238586, 0.003526770554233742919, 0.8754220627670087351 ) ) ;
#34406 = ORIENTED_EDGE ( 'NONE', *, *, #10361, .T. ) ;
#34407 = DIRECTION ( 'NONE',  ( 1.734723475976806848E-16, 0.000000000000000000, 1.000000000000000000 ) ) ;
#34408 = DIRECTION ( 'NONE',  ( 1.734723475976806848E-16, -0.000000000000000000, 1.000000000000000000 ) ) ;
#34409 = CARTESIAN_POINT ( 'NONE',  ( 0.2727639067037604392, 3.267716535433071279, -1.299212598425193210 ) ) ;
#34410 = VERTEX_POINT ( 'NONE', #30663 ) ;
#34411 = CARTESIAN_POINT ( 'NONE',  ( -0.6094175224461334528, 1.205361022782829114E-17, 1.763844451117148271 ) ) ;
#34412 = LINE ( 'NONE', #46249, #34457 ) ;
#34413 = LINE ( 'NONE', #23283, #4871 ) ;
#34414 = CIRCLE ( 'NONE', #26155, 2.066929133858268042 ) ;
#34415 = ORIENTED_EDGE ( 'NONE', *, *, #23168, .T. ) ;
#34416 = VECTOR ( 'NONE', #3415, 39.37007874015748143 ) ;
#34417 = CARTESIAN_POINT ( 'NONE',  ( -1.195183497228115035E-16, 0.000000000000000000, 0.3149606299212576177 ) ) ;
#34418 = EDGE_CURVE ( 'NONE', #47614, #35680, #39164, .T. ) ;
#34419 = VECTOR ( 'NONE', #22584, 39.37007874015748854 ) ;
#34420 = ADVANCED_FACE ( 'NONE', ( #22911 ), #50225, .T. ) ;
#34421 = EDGE_LOOP ( 'NONE', ( #12000, #5733, #36597, #23047 ) ) ;
#34422 = CARTESIAN_POINT ( 'NONE',  ( 0.08119777152254364916, 1.623385212329073957, 0.000000000000000000 ) ) ;
#34423 = VERTEX_POINT ( 'NONE', #49979 ) ;
#34424 = CARTESIAN_POINT ( 'NONE',  ( -0.8182917201112819283, 3.346456692913386100, 0.1574803149606285035 ) ) ;
#34425 = ADVANCED_FACE ( 'NONE', ( #15164 ), #15668, .F. ) ;
#34426 = CARTESIAN_POINT ( 'NONE',  ( -0.5455278134075214336, 3.346456692913386100, -0.9448818897637762948 ) ) ;
#34427 = DIRECTION ( 'NONE',  ( 1.734723475976806848E-16, 0.000000000000000000, 1.000000000000000000 ) ) ;
#34428 = DIRECTION ( 'NONE',  ( -3.469446951953613696E-16, 0.000000000000000000, -1.000000000000000000 ) ) ;
#34429 = SHAPE_REPRESENTATION ( 'Rotor', ( #26741 ), #43195 ) ;
#34430 = ORIENTED_EDGE ( 'NONE', *, *, #26071, .T. ) ;
#34431 = VERTEX_POINT ( 'NONE', #27534 ) ;
#34432 = ORIENTED_EDGE ( 'NONE', *, *, #8970, .F. ) ;
#34433 = PLANE ( 'NONE',  #25722 ) ;
#34434 = LINE ( 'NONE', #50123, #49365 ) ;
#34435 = ORIENTED_EDGE ( 'NONE', *, *, #39126, .F. ) ;
#34436 = CARTESIAN_POINT ( 'NONE',  ( -0.5455278134075214336, 0.000000000000000000, -8.878505979408855953E-16 ) ) ;
#34437 = CARTESIAN_POINT ( 'NONE',  ( 1.636583440222563857, 3.346456692913386100, -0.6299212598425181220 ) ) ;
#34438 = LINE ( 'NONE', #41174, #38487 ) ;
#34439 = VECTOR ( 'NONE', #13830, 39.37007874015748143 ) ;
#34440 = VERTEX_POINT ( 'NONE', #7422 ) ;
#34441 = ORIENTED_EDGE ( 'NONE', *, *, #17394, .T. ) ;
#34442 = EDGE_CURVE ( 'NONE', #39633, #41705, #15422, .T. ) ;
#34443 = CARTESIAN_POINT ( 'NONE',  ( 1.015142113812069979, 3.346456692913386100, 1.535433070866133898 ) ) ;
#34444 = CARTESIAN_POINT ( 'NONE',  ( -1.946505901478384759, -1.354463203825560094E-16, 0.9915739042680192794 ) ) ;
#34445 = DIRECTION ( 'NONE',  ( -0.000000000000000000, 1.000000000000000000, -0.000000000000000000 ) ) ;
#34446 = VERTEX_POINT ( 'NONE', #30413 ) ;
#34447 = FACE_BOUND ( 'NONE', #22188, .T. ) ;
#34448 = VERTEX_POINT ( 'NONE', #11543 ) ;
#34449 = EDGE_CURVE ( 'NONE', #38883, #39559, #43021, .T. ) ;
#34450 = LINE ( 'NONE', #37569, #30702 ) ;
#34451 = ORIENTED_EDGE ( 'NONE', *, *, #32305, .F. ) ;
#34452 = VERTEX_POINT ( 'NONE', #11792 ) ;
#34453 = FACE_OUTER_BOUND ( 'NONE', #23420, .T. ) ;
#34454 = CARTESIAN_POINT ( 'NONE',  ( 0.2727639067037610499, 3.346456692913386100, 2.047244094488179567 ) ) ;
#34455 = LINE ( 'NONE', #30323, #18169 ) ;
#34456 = VECTOR ( 'NONE', #302, 39.37007874015748143 ) ;
#34457 = VECTOR ( 'NONE', #39034, 39.37007874015748143 ) ;
#34458 = DIRECTION ( 'NONE',  ( 1.086719731106943413E-16, -1.000000000000000000, 4.078527368698718974E-17 ) ) ;
#34459 = PRODUCT_DEFINITION_CONTEXT ( 'detailed design', #20352, 'design' ) ;
#34460 = DIRECTION ( 'NONE',  ( -0.000000000000000000, 1.000000000000000000, -0.000000000000000000 ) ) ;
#34461 = ORIENTED_EDGE ( 'NONE', *, *, #11265, .F. ) ;
#34462 = AXIS2_PLACEMENT_3D ( 'NONE', #26806, #38698, #34326 ) ;
#34463 = EDGE_LOOP ( 'NONE', ( #21312, #9204, #32084, #3945 ) ) ;
#34464 = CARTESIAN_POINT ( 'NONE',  ( -1.536664496436148184E-16, 0.000000000000000000, -1.141732283464564013 ) ) ;
#34465 = LINE ( 'NONE', #14840, #32547 ) ;
#34466 = AXIS2_PLACEMENT_3D ( 'NONE', #37162, #29402, #17030 ) ;
#34467 = CARTESIAN_POINT ( 'NONE',  ( 0.1968503937007877735, 3.267716535433071279, 2.007874015748021268 ) ) ;
#34468 = AXIS2_PLACEMENT_3D ( 'NONE', #44644, #48746, #5424 ) ;
#34469 = PLANE ( 'NONE',  #614 ) ;
#34470 = LINE ( 'NONE', #42705, #24546 ) ;
#34471 = ORIENTED_EDGE ( 'NONE', *, *, #32106, .F. ) ;
#34472 = FACE_OUTER_BOUND ( 'NONE', #23855, .T. ) ;
#34473 = AXIS2_PLACEMENT_3D ( 'NONE', #4167, #32771, #29387 ) ;
#34474 = DIRECTION ( 'NONE',  ( -0.000000000000000000, 1.000000000000000000, -0.000000000000000000 ) ) ;
#34475 = ORIENTED_EDGE ( 'NONE', *, *, #2533, .T. ) ;
#34476 = CARTESIAN_POINT ( 'NONE',  ( 0.7423782071083087075, 0.000000000000000000, 0.3149606299212576177 ) ) ;
#34477 = CARTESIAN_POINT ( 'NONE',  ( 0.5455278134075217666, 0.000000000000000000, 1.574803149606291974 ) ) ;
#34478 = EDGE_LOOP ( 'NONE', ( #28485, #2042, #35009, #26791 ) ) ;
#34479 = LINE ( 'NONE', #34728, #23842 ) ;
#34480 = DIRECTION ( 'NONE',  ( -0.000000000000000000, 1.000000000000000000, -0.000000000000000000 ) ) ;
#34481 = PLANE ( 'NONE',  #39197 ) ;
#34482 = EDGE_CURVE ( 'NONE', #42262, #45506, #16768, .T. ) ;
#34483 = ADVANCED_FACE ( 'NONE', ( #38169 ), #43785, .F. ) ;
#34484 = ORIENTED_EDGE ( 'NONE', *, *, #33166, .F. ) ;
#34485 = CARTESIAN_POINT ( 'NONE',  ( 0.04921259842519690175, 0.02870789531899127500, 1.849213118431110914 ) ) ;
#34486 = VERTEX_POINT ( 'NONE', #20571 ) ;
#34487 = FACE_BOUND ( 'NONE', #50299, .T. ) ;
#34488 = EDGE_CURVE ( 'NONE', #33365, #45283, #35550, .T. ) ;
#34489 = DIRECTION ( 'NONE',  ( -1.000000000000000000, -0.000000000000000000, -0.000000000000000000 ) ) ;
#34491 = EDGE_CURVE ( 'NONE', #33914, #4458, #12829, .T. ) ;
#34490 = CARTESIAN_POINT ( 'NONE',  ( 1.930190994932111215, 1.205361022782829114E-17, -0.9827944786818438860 ) ) ;
#34492 = VECTOR ( 'NONE', #14164, 39.37007874015748143 ) ;
#34493 = ADVANCED_FACE ( 'NONE', ( #36067 ), #28562, .F. ) ;
#34494 = ORIENTED_EDGE ( 'NONE', *, *, #28837, .F. ) ;
#34495 = ORIENTED_EDGE ( 'NONE', *, *, #37582, .F. ) ;
#34496 = LINE ( 'NONE', #49931, #19076 ) ;
#34497 = DIRECTION ( 'NONE',  ( -2.582876339026340310E-17, -1.000000000000000000, 1.131632063491650798E-16 ) ) ;
#34498 = CONICAL_SURFACE ( 'NONE', #48445, 2.244934639244524632, 1.554780866114618743 ) ;
#34499 = DIRECTION ( 'NONE',  ( -3.469446951953613696E-16, 0.000000000000000000, -1.000000000000000000 ) ) ;
#34500 = CARTESIAN_POINT ( 'NONE',  ( 0.1450362469327829418, 5.905511811023623991, -2.160491579385212191 ) ) ;
#34501 = CARTESIAN_POINT ( 'NONE',  ( -0.4161812636739087856, 0.000000000000000000, -1.692983086477939825 ) ) ;
#34502 = VECTOR ( 'NONE', #32416, 39.37007874015748143 ) ;
#34503 = AXIS2_PLACEMENT_3D ( 'NONE', #9590, #13975, #20685 ) ;
#34504 = ORIENTED_EDGE ( 'NONE', *, *, #46557, .T. ) ;
#34505 = EDGE_CURVE ( 'NONE', #18049, #18215, #40579, .T. ) ;
#34506 = ORIENTED_EDGE ( 'NONE', *, *, #23901, .T. ) ;
#34507 = CARTESIAN_POINT ( 'NONE',  ( -0.8942052331142551491, 3.267716535433071279, 3.102397620449222974E-16 ) ) ;
#34508 = AXIS2_PLACEMENT_3D ( 'NONE', #13369, #2258, #2763 ) ;
#34509 = DIRECTION ( 'NONE',  ( -0.9998717552508121775, -0.01601477604151182663, 0.000000000000000000 ) ) ;
#34510 = EDGE_LOOP ( 'NONE', ( #36588, #29463, #43687, #14160 ) ) ;
#34511 = EDGE_CURVE ( 'NONE', #46791, #49048, #13088, .T. ) ;
#34512 = CARTESIAN_POINT ( 'NONE',  ( -1.363819533518803473, 0.000000000000000000, -1.614173228346451605 ) ) ;
#34513 = ORIENTED_EDGE ( 'NONE', *, *, #6581, .F. ) ;
#34514 = ORIENTED_EDGE ( 'NONE', *, *, #1412, .T. ) ;
#34515 = AXIS2_PLACEMENT_3D ( 'NONE', #20818, #28045, #21076 ) ;
#34516 = EDGE_CURVE ( 'NONE', #20168, #35311, #16706, .T. ) ;
#34517 = ORIENTED_EDGE ( 'NONE', *, *, #48681, .F. ) ;
#34518 = VERTEX_POINT ( 'NONE', #39676 ) ;
#34519 = FACE_OUTER_BOUND ( 'NONE', #43238, .T. ) ;
#34520 = DIRECTION ( 'NONE',  ( 1.000000000000000000, -0.000000000000000000, 0.000000000000000000 ) ) ;
#34521 = EDGE_CURVE ( 'NONE', #6492, #23952, #26129, .T. ) ;
#34522 = CARTESIAN_POINT ( 'NONE',  ( 1.034308760555261886, 1.626043101691516890, -2.034340803895991812 ) ) ;
#34523 = AXIS2_PLACEMENT_3D ( 'NONE', #45321, #17982, #21351 ) ;
#34524 = CARTESIAN_POINT ( 'NONE',  ( 1.909347346926324684, 3.346456692913386100, 0.4724409448818868706 ) ) ;
#34525 = DIRECTION ( 'NONE',  ( -0.01601477604151182663, 0.9998717552508123996, -0.000000000000000000 ) ) ;
#34526 = CARTESIAN_POINT ( 'NONE',  ( 1.503187667178186970, 0.5249316475426856199, 1.135806887101860729 ) ) ;
#34527 = ORIENTED_EDGE ( 'NONE', *, *, #12567, .T. ) ;
#34528 = CARTESIAN_POINT ( 'NONE',  ( -1.486187880958815377, 3.346456692913386100, -1.574803149606293307 ) ) ;
#34529 = FACE_OUTER_BOUND ( 'NONE', #36698, .T. ) ;
#34530 = CARTESIAN_POINT ( 'NONE',  ( 0.1968503937007878568, 3.346456692913386100, 2.204724409448808764 ) ) ;
#34531 = CARTESIAN_POINT ( 'NONE',  ( 0.000000000000000000, 0.000000000000000000, 0.000000000000000000 ) ) ;
#34532 = VECTOR ( 'NONE', #29736, 39.37007874015748143 ) ;
#34533 = VECTOR ( 'NONE', #49738, 39.37007874015748143 ) ;
#34534 = ORIENTED_EDGE ( 'NONE', *, *, #9843, .F. ) ;
#34535 = LINE ( 'NONE', #14654, #28959 ) ;
#34536 = FACE_OUTER_BOUND ( 'NONE', #760, .T. ) ;
#34537 = ORIENTED_EDGE ( 'NONE', *, *, #12392, .T. ) ;
#34538 = DIRECTION ( 'NONE',  ( -0.3166081466550567658, 0.000000000000000000, -0.9485564197619719140 ) ) ;
#34539 = DIRECTION ( 'NONE',  ( 1.000000000000000000, 0.000000000000000000, 0.000000000000000000 ) ) ;
#34540=STYLED_ITEM('',(#51073),#41217);
#34541 = CARTESIAN_POINT ( 'NONE',  ( -3.414809992080329023E-17, 3.346456692913386100, -0.1968503937007874405 ) ) ;
#34542 = CONICAL_SURFACE ( 'NONE', #41987, 2.244934639244524632, 1.554780866114618743 ) ;
#34543 = EDGE_LOOP ( 'NONE', ( #5302, #16871, #15593, #41237 ) ) ;
#34544 = CARTESIAN_POINT ( 'NONE',  ( -2.695799277629577162, 1.578813927010291218, -1.205759334241492731 ) ) ;
#34545 = EDGE_CURVE ( 'NONE', #32403, #23735, #4061, .T. ) ;
#34546 = CARTESIAN_POINT ( 'NONE',  ( 0.000000000000000000, 2.755905511811024056, 0.000000000000000000 ) ) ;
#34547 = DIRECTION ( 'NONE',  ( -3.986037398843765983E-20, -1.000000000000000000, -1.160734090543304660E-16 ) ) ;
#34548 = LINE ( 'NONE', #14669, #13574 ) ;
#34549 = CARTESIAN_POINT ( 'NONE',  ( 0.7423782071083090406, 3.267716535433071279, -2.575641807848711180E-16 ) ) ;
#34550 = ORIENTED_EDGE ( 'NONE', *, *, #12126, .T. ) ;
#34551 = EDGE_CURVE ( 'NONE', #31670, #421, #7924, .T. ) ;
#34552 = DIRECTION ( 'NONE',  ( 0.9998717552508121775, 0.01601477604151182663, 0.000000000000000000 ) ) ;
#34553 = ORIENTED_EDGE ( 'NONE', *, *, #41226, .T. ) ;
#34554 = ORIENTED_EDGE ( 'NONE', *, *, #20344, .T. ) ;
#34555 = DIRECTION ( 'NONE',  ( 1.734723475976806848E-16, -0.000000000000000000, 1.000000000000000000 ) ) ;
#34556 = EDGE_LOOP ( 'NONE', ( #17614, #33921, #16250 ) ) ;
#34557 = DIRECTION ( 'NONE',  ( -1.000000000000000000, 0.000000000000000000, 0.000000000000000000 ) ) ;
#34558 = LINE ( 'NONE', #42288, #2963 ) ;
#34559 = ORIENTED_EDGE ( 'NONE', *, *, #19501, .T. ) ;
#34560 = PLANE ( 'NONE',  #23 ) ;
#34561 = AXIS2_PLACEMENT_3D ( 'NONE', #42667, #31058, #15308 ) ;
#34562 = FACE_OUTER_BOUND ( 'NONE', #3554, .T. ) ;
#34563 = DIRECTION ( 'NONE',  ( -0.000000000000000000, 1.000000000000000000, -0.000000000000000000 ) ) ;
#34564 = ORIENTED_EDGE ( 'NONE', *, *, #25995, .T. ) ;
#34565 = ORIENTED_EDGE ( 'NONE', *, *, #21667, .T. ) ;
#34566 = CARTESIAN_POINT ( 'NONE',  ( -1.362940969001253944, 0.6859011407150840123, -1.392964542809770556 ) ) ;
#34567 = FACE_BOUND ( 'NONE', #30783, .T. ) ;
#34568 = ORIENTED_EDGE ( 'NONE', *, *, #34449, .T. ) ;
#34569 = VECTOR ( 'NONE', #9110, 39.37007874015748143 ) ;
#34570 = DIRECTION ( 'NONE',  ( 1.000000000000000000, -0.000000000000000000, 0.000000000000000000 ) ) ;
#34571 = EDGE_CURVE ( 'NONE', #16142, #5543, #31944, .T. ) ;
#34572 = ORIENTED_EDGE ( 'NONE', *, *, #41543, .T. ) ;
#34573 = ORIENTED_EDGE ( 'NONE', *, *, #30155, .F. ) ;
#34574 = VECTOR ( 'NONE', #27474, 39.37007874015748143 ) ;
#34575 = CARTESIAN_POINT ( 'NONE',  ( -0.3486774197067337711, 3.267716535433071279, 1.209717811016578338E-16 ) ) ;
#34576 = DIRECTION ( 'NONE',  ( -0.000000000000000000, -1.000000000000000000, -0.000000000000000000 ) ) ;
#34577 = EDGE_LOOP ( 'NONE', ( #20277, #25768, #14436, #17056 ) ) ;
#34578 = AXIS2_PLACEMENT_3D ( 'NONE', #25399, #44749, #5784 ) ;
#34579 = LINE ( 'NONE', #46413, #702 ) ;
#34580 = ADVANCED_FACE ( 'NONE', ( #8949 ), #23667, .F. ) ;
#34581 = ORIENTED_EDGE ( 'NONE', *, *, #37760, .T. ) ;
#34582 = CARTESIAN_POINT ( 'NONE',  ( -2.145579962785661543, 1.559576214923994453, -2.028675302499262312 ) ) ;
#34583 = DIRECTION ( 'NONE',  ( 0.000000000000000000, 0.000000000000000000, -1.000000000000000000 ) ) ;
#34584 = EDGE_CURVE ( 'NONE', #26794, #9867, #29093, .T. ) ;
#34585 = CARTESIAN_POINT ( 'NONE',  ( -0.8942052331142552601, 0.000000000000000000, -1.259842519685034690 ) ) ;
#34586 = ORIENTED_EDGE ( 'NONE', *, *, #17268, .F. ) ;
#34587 = ORIENTED_EDGE ( 'NONE', *, *, #5822, .T. ) ;
#34588 = DIRECTION ( 'NONE',  ( 0.000000000000000000, -1.000000000000000000, 0.000000000000000000 ) ) ;
#34589 = FACE_OUTER_BOUND ( 'NONE', #18773, .T. ) ;
#34590 = LINE ( 'NONE', #15214, #20861 ) ;
#34591 = EDGE_CURVE ( 'NONE', #8821, #3678, #48152, .T. ) ;
#34592 = DIRECTION ( 'NONE',  ( 7.237058681235204266E-17, -1.000000000000000000, 9.074984547606538936E-17 ) ) ;
#34593 = EDGE_CURVE ( 'NONE', #41617, #4117, #16447, .T. ) ;
#34594 = FACE_OUTER_BOUND ( 'NONE', #13227, .T. ) ;
#34595 = CARTESIAN_POINT ( 'NONE',  ( 0.000000000000000000, 0.000000000000000000, -2.066929133858268042 ) ) ;
#34596 = AXIS2_PLACEMENT_3D ( 'NONE', #17539, #49247, #2558 ) ;
#34597 = CARTESIAN_POINT ( 'NONE',  ( 2.932638728931774352, 1.205361022782829114E-17, 0.3475908556738223631 ) ) ;
#34598 = ORIENTED_EDGE ( 'NONE', *, *, #42116, .T. ) ;
#34599 = DIRECTION ( 'NONE',  ( -3.469446951953613696E-16, 0.000000000000000000, -1.000000000000000000 ) ) ;
#34600 = LINE ( 'NONE', #50529, #21153 ) ;
#34601 = ORIENTED_EDGE ( 'NONE', *, *, #33889, .T. ) ;
#34603 = EDGE_CURVE ( 'NONE', #21491, #22636, #27790, .T. ) ;
#34602 = ORIENTED_EDGE ( 'NONE', *, *, #42900, .F. ) ;
#34604 = DIRECTION ( 'NONE',  ( -1.000000000000000000, 0.000000000000000000, -0.000000000000000000 ) ) ;
#34605 = AXIS2_PLACEMENT_3D ( 'NONE', #42627, #46229, #46722 ) ;
#34606 = DIRECTION ( 'NONE',  ( -1.000000000000000000, 0.000000000000000000, 5.782411586589357392E-17 ) ) ;
#34607 = VERTEX_POINT ( 'NONE', #4827 ) ;
#34608 = EDGE_CURVE ( 'NONE', #50705, #42620, #20824, .T. ) ;
#34609 = ADVANCED_FACE ( 'NONE', ( #9462 ), #29331, .F. ) ;
#34610 = EDGE_CURVE ( 'NONE', #50288, #21767, #5587, .T. ) ;
#34611 = ORIENTED_EDGE ( 'NONE', *, *, #21304, .T. ) ;
#34612 = CARTESIAN_POINT ( 'NONE',  ( -0.2727639067037602727, 3.267716535433071279, 0.5905511811023582691 ) ) ;
#34613 = VECTOR ( 'NONE', #45006, 39.37007874015748143 ) ;
#34614 = ORIENTED_EDGE ( 'NONE', *, *, #50334, .T. ) ;
#34615 = CARTESIAN_POINT ( 'NONE',  ( 2.225020958752729872, 1.645114536686943296, 0.6712079458291126954 ) ) ;
#34616 = CARTESIAN_POINT ( 'NONE',  ( 0.000000000000000000, 3.267716535433071279, -0.03937007874015908959 ) ) ;
#34617 = ORIENTED_EDGE ( 'NONE', *, *, #35072, .T. ) ;
#34618 = CARTESIAN_POINT ( 'NONE',  ( -1.985260859929297572, 3.346456692913386100, -6.146657985744592735E-16 ) ) ;
#34619 = ORIENTED_EDGE ( 'NONE', *, *, #19814, .T. ) ;
#34620 = ORIENTED_EDGE ( 'NONE', *, *, #18084, .F. ) ;
#34621 = DIRECTION ( 'NONE',  ( -0.9998717552508121775, -0.01601477604151182663, 0.000000000000000000 ) ) ;
#34622 = LINE ( 'NONE', #46210, #15291 ) ;
#34623 = VERTEX_POINT ( 'NONE', #49667 ) ;
#34624 = CARTESIAN_POINT ( 'NONE',  ( -0.8942052331142552601, 3.267716535433071279, -1.574803149606293529 ) ) ;
#34625 = LINE ( 'NONE', #18631, #11014 ) ;
#34626 = VECTOR ( 'NONE', #25415, 39.37007874015748143 ) ;
#34627 = EDGE_CURVE ( 'NONE', #40529, #21172, #45064, .T. ) ;
#34628 = VERTEX_POINT ( 'NONE', #37091 ) ;
#34629 = DIRECTION ( 'NONE',  ( 0.000000000000000000, 0.000000000000000000, -1.000000000000000000 ) ) ;
#34630 = B_SPLINE_CURVE_WITH_KNOTS ( 'NONE', 3,
 ( #38764, #3392, #15014, #49826 ),
 .UNSPECIFIED., .F., .F.,
 ( 4, 4 ),
 ( 4.798888246254521888E-05, 0.002548021674202805703 ),
 .UNSPECIFIED. ) ;
#34631 = ORIENTED_EDGE ( 'NONE', *, *, #41745, .T. ) ;
#34632 = ORIENTED_EDGE ( 'NONE', *, *, #26974, .T. ) ;
#34633 =( NAMED_UNIT ( * ) SI_UNIT ( $, .STERADIAN. ) SOLID_ANGLE_UNIT ( ) );
#34634 = EDGE_CURVE ( 'NONE', #2922, #43170, #25458, .T. ) ;
#34635 = CARTESIAN_POINT ( 'NONE',  ( 0.07982360342473591996, 1.709180471932028711, 0.000000000000000000 ) ) ;
#34636 = VECTOR ( 'NONE', #20348, 39.37007874015748143 ) ;
#34637 = CARTESIAN_POINT ( 'NONE',  ( 1.287906020515830141, 0.000000000000000000, 0.4330708661417287386 ) ) ;
#34638 = VECTOR ( 'NONE', #15331, 39.37007874015748143 ) ;
#34639 = EDGE_CURVE ( 'NONE', #47515, #11356, #29844, .T. ) ;
#34640 = EDGE_CURVE ( 'NONE', #31327, #28604, #40967, .T. ) ;
#34641 = CARTESIAN_POINT ( 'NONE',  ( -1.959565595350794220, 0.5253755374352464536, -0.8910779565606279373 ) ) ;
#34642 = LINE ( 'NONE', #35397, #40401 ) ;
#34643 = VERTEX_POINT ( 'NONE', #17968 ) ;
#34645 = EDGE_CURVE ( 'NONE', #15165, #34963, #41219, .T. ) ;
#34644 = VERTEX_POINT ( 'NONE', #13595 ) ;
#34646 = LINE ( 'NONE', #22769, #31250 ) ;
#34647 = DIRECTION ( 'NONE',  ( 1.734723475976806848E-16, -0.000000000000000000, 1.000000000000000000 ) ) ;
#34648 = AXIS2_PLACEMENT_3D ( 'NONE', #5723, #44183, #21467 ) ;
#34649 = EDGE_LOOP ( 'NONE', ( #29055, #39074, #3356, #26969 ) ) ;
#34650 = CARTESIAN_POINT ( 'NONE',  ( 0.000000000000000000, 0.000000000000000000, 0.000000000000000000 ) ) ;
#34651 = DIRECTION ( 'NONE',  ( -1.118904554427321068E-16, -1.000000000000000000, -3.087980359898530052E-17 ) ) ;
#34652 = CARTESIAN_POINT ( 'NONE',  ( -1.195183497228115035E-16, 0.000000000000000000, -0.9448818897637765168 ) ) ;
#34653 = CARTESIAN_POINT ( 'NONE',  ( 0.002207914879453961969, 6.692913385826772199, 0.04916304461325451958 ) ) ;
#34654 = DIRECTION ( 'NONE',  ( -0.01601477604151182663, 0.9998717552508123996, -0.000000000000000000 ) ) ;
#34655 = ORIENTED_EDGE ( 'NONE', *, *, #16199, .T. ) ;
#34656 = CARTESIAN_POINT ( 'NONE',  ( 2.043634885149959057, 6.692913385826772199, 0.7157624142946238388 ) ) ;
#34657 = DIRECTION ( 'NONE',  ( 0.01601477604151182663, -0.9998717552508123996, 0.000000000000000000 ) ) ;
#34658 = ADVANCED_FACE ( 'NONE', ( #5840 ), #17212, .F. ) ;
#34659 = DIRECTION ( 'NONE',  ( 1.000000000000000000, 0.000000000000000000, 0.000000000000000000 ) ) ;
#34660 = VERTEX_POINT ( 'NONE', #21590 ) ;
#34661 = DIRECTION ( 'NONE',  ( 1.000000000000000000, 0.000000000000000000, 0.000000000000000000 ) ) ;
#34662 = EDGE_CURVE ( 'NONE', #27595, #14000, #9845, .T. ) ;
#34663 = CARTESIAN_POINT ( 'NONE',  ( -1.166969139818015977, 0.000000000000000000, -0.4724409448818886470 ) ) ;
#34664 = DIRECTION ( 'NONE',  ( 1.000000000000000000, -0.000000000000000000, 0.000000000000000000 ) ) ;
#34665 = VERTEX_POINT ( 'NONE', #24953 ) ;
#34666 = EDGE_CURVE ( 'NONE', #38782, #1604, #1711, .T. ) ;
#34667 = LINE ( 'NONE', #50350, #35786 ) ;
#34668 = EDGE_CURVE ( 'NONE', #13594, #24976, #21848, .T. ) ;
#34669 = ORIENTED_EDGE ( 'NONE', *, *, #23041, .T. ) ;
#34670 = DIRECTION ( 'NONE',  ( -0.000000000000000000, 1.000000000000000000, -0.000000000000000000 ) ) ;
#34671 = EDGE_LOOP ( 'NONE', ( #50694, #40937, #6037, #31236 ) ) ;
#34672 = FACE_OUTER_BOUND ( 'NONE', #50608, .T. ) ;
#34673 = ORIENTED_EDGE ( 'NONE', *, *, #27872, .F. ) ;
#34674 = AXIS2_PLACEMENT_3D ( 'NONE', #25064, #40816, #5438 ) ;
#34675 = DIRECTION ( 'NONE',  ( -0.9998717552508121775, -0.01601477604151182316, 0.000000000000000000 ) ) ;
#34676 = CARTESIAN_POINT ( 'NONE',  ( 1.287906020515830363, 3.267716535433071279, -4.468321617281356063E-16 ) ) ;
#34677 = DIRECTION ( 'NONE',  ( -0.000000000000000000, 1.000000000000000000, -0.000000000000000000 ) ) ;
#34678 = VECTOR ( 'NONE', #31946, 39.37007874015748854 ) ;
#34679 = ORIENTED_EDGE ( 'NONE', *, *, #44155, .F. ) ;
#34680 = ORIENTED_EDGE ( 'NONE', *, *, #23990, .F. ) ;
#34681 = ORIENTED_EDGE ( 'NONE', *, *, #16659, .T. ) ;
#34682 = DIRECTION ( 'NONE',  ( 0.000000000000000000, 1.000000000000000000, 0.000000000000000000 ) ) ;
#34683 = CARTESIAN_POINT ( 'NONE',  ( -1.133754555558240673, 0.009760511380980992774, 1.372484652545675532 ) ) ;
#34684 = ORIENTED_EDGE ( 'NONE', *, *, #9473, .F. ) ;
#34685 = DIRECTION ( 'NONE',  ( -1.000000000000000000, 0.000000000000000000, -0.000000000000000000 ) ) ;
#34686 = DIRECTION ( 'NONE',  ( 1.000000000000000000, 0.000000000000000000, 0.000000000000000000 ) ) ;
#34687 = CIRCLE ( 'NONE', #12413, 2.165354330708661568 ) ;
#34688 = CARTESIAN_POINT ( 'NONE',  ( 0.000000000000000000, 3.267716535433071279, 0.5905511811023582691 ) ) ;
#34689 = ORIENTED_EDGE ( 'NONE', *, *, #7765, .F. ) ;
#34690 = ORIENTED_EDGE ( 'NONE', *, *, #32115, .F. ) ;
#34691 = DIRECTION ( 'NONE',  ( -0.000000000000000000, 1.000000000000000000, -0.000000000000000000 ) ) ;
#34692 = CARTESIAN_POINT ( 'NONE',  ( 0.000000000000000000, 3.267716535433071279, -0.9842519685039348154 ) ) ;
#34693 = PLANE ( 'NONE',  #45916 ) ;
#34694 = ORIENTED_EDGE ( 'NONE', *, *, #7404, .T. ) ;
#34695 = CARTESIAN_POINT ( 'NONE',  ( 0.6502734851936936566, 1.718317270777941941, -2.171228911417812046 ) ) ;
#34696 = ORIENTED_EDGE ( 'NONE', *, *, #25319, .T. ) ;
#34697 = DIRECTION ( 'NONE',  ( 0.000000000000000000, 0.000000000000000000, -1.000000000000000000 ) ) ;
#34698 = VERTEX_POINT ( 'NONE', #13846 ) ;
#34699 = ORIENTED_EDGE ( 'NONE', *, *, #8769, .F. ) ;
#34700 = PLANE ( 'NONE',  #27062 ) ;
#34701 = CARTESIAN_POINT ( 'NONE',  ( -2.823445274216743073, 0.000000000000000000, 0.8656477926280280455 ) ) ;
#34702 = DIRECTION ( 'NONE',  ( -1.000000000000000000, -0.000000000000000000, -0.000000000000000000 ) ) ;
#34703 = ADVANCED_FACE ( 'NONE', ( #25209 ), #17459, .F. ) ;
#34704 = CARTESIAN_POINT ( 'NONE',  ( -0.1491611873099766838, 0.5239554268833609418, -2.206323420686062686 ) ) ;
#34705 = DIRECTION ( 'NONE',  ( 1.000000000000000000, 0.000000000000000000, 0.000000000000000000 ) ) ;
#34706 = VERTEX_POINT ( 'NONE', #25713 ) ;
#34707 = EDGE_CURVE ( 'NONE', #17342, #39701, #41466, .T. ) ;
#34708 = ADVANCED_FACE ( 'NONE', ( #25970 ), #6093, .F. ) ;
#34709 = B_SPLINE_CURVE_WITH_KNOTS ( 'NONE', 3,
 ( #18908, #10317, #36930, #1804 ),
 .UNSPECIFIED., .F., .F.,
 ( 4, 4 ),
 ( 0.0002206499228107822511, 0.04984066487308089904 ),
 .UNSPECIFIED. ) ;
#34710 = ORIENTED_EDGE ( 'NONE', *, *, #11384, .F. ) ;
#34711 = CARTESIAN_POINT ( 'NONE',  ( -2.071704270381554913, 3.267716535433071279, 0.6299212598425164567 ) ) ;
#34712 = PLANE ( 'NONE',  #41603 ) ;
#34713 = VECTOR ( 'NONE', #35604, 39.37007874015748143 ) ;
#34714 = VECTOR ( 'NONE', #20589, 39.37007874015748854 ) ;
#34715 = CARTESIAN_POINT ( 'NONE',  ( -1.712496953225537188, 0.000000000000000000, 0.1574803149606286423 ) ) ;
#34716 = CARTESIAN_POINT ( 'NONE',  ( 2.063617991565069865, 1.675337772409502435, 1.054594607282280050 ) ) ;
#34717 = VERTEX_POINT ( 'NONE', #32976 ) ;
#34718 = CARTESIAN_POINT ( 'NONE',  ( -1.463531759593973858, 0.5244536452976792384, 1.600348737355761886 ) ) ;
#34719 = VECTOR ( 'NONE', #8711, 39.37007874015748143 ) ;
#34720 = ADVANCED_FACE ( 'NONE', ( #37604 ), #2229, .F. ) ;
#34721 = CARTESIAN_POINT ( 'NONE',  ( 1.287906020515830141, 3.346456692913386100, 0.6299212598425161236 ) ) ;
#34722 = ORIENTED_EDGE ( 'NONE', *, *, #9664, .F. ) ;
#34723 = VECTOR ( 'NONE', #46809, 39.37007874015748143 ) ;
#34724 = CARTESIAN_POINT ( 'NONE',  ( -0.07591351300297340121, 0.000000000000000000, -0.3543307086614175816 ) ) ;
#34725 = EDGE_CURVE ( 'NONE', #50319, #4205, #15107, .T. ) ;
#34726 = CARTESIAN_POINT ( 'NONE',  ( 1.152568299495707382, 6.692913385826772199, 1.833124570921553342 ) ) ;
#34727 =( BOUNDED_CURVE ( )  B_SPLINE_CURVE ( 3, ( #48507, #44153, #8795, #24543 ),
 .UNSPECIFIED., .F., .F. ) 
 B_SPLINE_CURVE_WITH_KNOTS ( ( 4, 4 ),
 ( 3.976082376286302900, 4.026957665532088448 ),
 .UNSPECIFIED. ) 
 CURVE ( )  GEOMETRIC_REPRESENTATION_ITEM ( )  RATIONAL_B_SPLINE_CURVE ( ( 1.000000000000000000, 0.9997843203757749153, 0.9997843203757749153, 1.000000000000000000 ) ) 
 REPRESENTATION_ITEM ( '' )  );
#34728 = CARTESIAN_POINT ( 'NONE',  ( 1.979793062125284830, 1.205361022782829114E-17, 2.191257344206568813 ) ) ;
#34729 = DIRECTION ( 'NONE',  ( 1.000000000000000000, -0.000000000000000000, 0.000000000000000000 ) ) ;
#34730 = CARTESIAN_POINT ( 'NONE',  ( 0.07982360342473591996, 1.709180471932028711, 0.000000000000000000 ) ) ;
#34731 = CARTESIAN_POINT ( 'NONE',  ( 1.363819533518803251, 0.000000000000000000, -0.03937007874015908959 ) ) ;
#34732 = B_SPLINE_CURVE_WITH_KNOTS ( 'NONE', 3,
 ( #43248, #7898, #9691, #32952 ),
 .UNSPECIFIED., .F., .F.,
 ( 4, 4 ),
 ( 0.000000000000000000, 1.000000000000000000 ),
 .UNSPECIFIED. ) ;
#34733 = ADVANCED_FACE ( 'NONE', ( #50171 ), #30863, .F. ) ;
#34734 = ORIENTED_EDGE ( 'NONE', *, *, #25806, .T. ) ;
#34735 = DIRECTION ( 'NONE',  ( 1.734723475976806848E-16, 0.000000000000000000, 1.000000000000000000 ) ) ;
#34736 = VERTEX_POINT ( 'NONE', #42215 ) ;
#34737 = FACE_BOUND ( 'NONE', #22425, .T. ) ;
#34738 = CARTESIAN_POINT ( 'NONE',  ( 0.7145799201508789000, 1.574803149606302854, 2.044048657746659448 ) ) ;
#34739 = CARTESIAN_POINT ( 'NONE',  ( 1.363819533518803251, 3.346456692913386100, -0.9842519685039348154 ) ) ;
#34740 = ORIENTED_EDGE ( 'NONE', *, *, #4988, .F. ) ;
#34741 = ORIENTED_EDGE ( 'NONE', *, *, #16474, .F. ) ;
#34742 = DIRECTION ( 'NONE',  ( -3.986037398843765983E-20, -1.000000000000000000, -1.160734090543304660E-16 ) ) ;
#34743 = DIRECTION ( 'NONE',  ( 1.734723475976806848E-16, -0.000000000000000000, 1.000000000000000000 ) ) ;
#34744 = FACE_OUTER_BOUND ( 'NONE', #8976, .T. ) ;
#34745 = DIRECTION ( 'NONE',  ( 1.734723475976806848E-16, -0.000000000000000000, 1.000000000000000000 ) ) ;
#34746 = DIRECTION ( 'NONE',  ( -0.000000000000000000, 1.000000000000000000, -0.000000000000000000 ) ) ;
#34747 = AXIS2_PLACEMENT_3D ( 'NONE', #11286, #22649, #14652 ) ;
#34748 = CARTESIAN_POINT ( 'NONE',  ( -0.2727639067037602172, 0.000000000000000000, 2.047244094488179567 ) ) ;
#34749 = VECTOR ( 'NONE', #26184, 39.37007874015748143 ) ;
#34750 = ORIENTED_EDGE ( 'NONE', *, *, #3173, .F. ) ;
#34751 = ORIENTED_EDGE ( 'NONE', *, *, #7425, .F. ) ;
#34752 = CARTESIAN_POINT ( 'NONE',  ( -1.312248418042854192, 5.905511811023623991, -1.722429524498108711 ) ) ;
#34753 = PLANE ( 'NONE',  #40535 ) ;
#34754 = VECTOR ( 'NONE', #50927, 39.37007874015748143 ) ;
#34755 = ORIENTED_EDGE ( 'NONE', *, *, #25041, .T. ) ;
#34756 = CARTESIAN_POINT ( 'NONE',  ( 0.2727639067037605503, 3.267716535433071279, -4.731699523581609125E-17 ) ) ;
#34757 = ORIENTED_EDGE ( 'NONE', *, *, #47253, .F. ) ;
#34758 = CONICAL_SURFACE ( 'NONE', #32291, 1.850107469027523210, 0.6386652850508578450 ) ;
#34759 = ORIENTED_EDGE ( 'NONE', *, *, #9791, .T. ) ;
#34760 = VECTOR ( 'NONE', #48834, 39.37007874015748143 ) ;
#34761 = ORIENTED_EDGE ( 'NONE', *, *, #47322, .T. ) ;
#34762 = ORIENTED_EDGE ( 'NONE', *, *, #8723, .F. ) ;
#34763 = CARTESIAN_POINT ( 'NONE',  ( 1.015142113812069091, 0.000000000000000000, -1.417322834645664331 ) ) ;
#34764 = EDGE_CURVE ( 'NONE', #43265, #35577, #46568, .T. ) ;
#34765 = ADVANCED_FACE ( 'NONE', ( #50665 ), #49270, .F. ) ;
#34766 = CARTESIAN_POINT ( 'NONE',  ( -1.712496953225537855, 3.346456692913386100, -1.226315847645294221 ) ) ;
#34767 = EDGE_CURVE ( 'NONE', #25092, #209, #28816, .T. ) ;
#34768 = CARTESIAN_POINT ( 'NONE',  ( 1.883550378546973603, 0.000000000000000000, -1.069467267250420628 ) ) ;
#34769 = EDGE_CURVE ( 'NONE', #47582, #26865, #30606, .T. ) ;
#34770 = EDGE_CURVE ( 'NONE', #35609, #31365, #7114, .T. ) ;
#34771 = DIRECTION ( 'NONE',  ( -1.267583980596137654E-16, 1.000000000000000000, -2.300325776299734791E-17 ) ) ;
#34772 = CARTESIAN_POINT ( 'NONE',  ( 1.956098637639549720, 1.739232450405700847, -1.232242025355393844 ) ) ;
#34773 = DIRECTION ( 'NONE',  ( 1.734723475976806848E-16, -0.000000000000000000, 1.000000000000000000 ) ) ;
#34774 = EDGE_LOOP ( 'NONE', ( #20990, #32816, #47224, #18383 ) ) ;
#34775 = CARTESIAN_POINT ( 'NONE',  ( -0.2727639067037602172, 3.346456692913386100, 2.047244094488179567 ) ) ;
#34776 = PLANE ( 'NONE',  #11019 ) ;
#34777 = DIRECTION ( 'NONE',  ( -0.9749279121818259508, -0.000000000000000000, 0.2225209339563041788 ) ) ;
#34778 = CARTESIAN_POINT ( 'NONE',  ( 1.669153017917641924, 1.205361022782829114E-17, 1.268159837793114031 ) ) ;
#34779 = VECTOR ( 'NONE', #44485, 39.37007874015748143 ) ;
#34780 = ORIENTED_EDGE ( 'NONE', *, *, #32740, .T. ) ;
#34781 = AXIS2_PLACEMENT_3D ( 'NONE', #9098, #48297, #1091 ) ;
#34782 = LINE ( 'NONE', #3282, #40512 ) ;
#34783 = EDGE_CURVE ( 'NONE', #46441, #37232, #11239, .T. ) ;
#34784 = PLANE ( 'NONE',  #23639 ) ;
#34785 = ORIENTED_EDGE ( 'NONE', *, *, #31728, .T. ) ;
#34786 = CARTESIAN_POINT ( 'NONE',  ( 1.014069264286641792, 0.4724409448818898127, 1.014069264286641570 ) ) ;
#34787 = CARTESIAN_POINT ( 'NONE',  ( 0.04921259842519669359, 1.617808935111010760, 2.717264019652364304 ) ) ;
#34788 = VECTOR ( 'NONE', #49745, 39.37007874015748143 ) ;
#34789 = EDGE_CURVE ( 'NONE', #18884, #18853, #22858, .T. ) ;
#34790 = VECTOR ( 'NONE', #24728, 39.37007874015748143 ) ;
#34791 = CARTESIAN_POINT ( 'NONE',  ( 2.225020958752729872, 1.645114536686943296, 0.6712079458291126954 ) ) ;
#34792 = VERTEX_POINT ( 'NONE', #26968 ) ;
#34793 = PLANE ( 'NONE',  #23131 ) ;
#34794 = FACE_OUTER_BOUND ( 'NONE', #16569, .T. ) ;
#34795 = VECTOR ( 'NONE', #32383, 39.37007874015748143 ) ;
#34796 = PLANE ( 'NONE',  #27021 ) ;
#34797 = DIRECTION ( 'NONE',  ( -0.9639628606958512425, 1.288287287306305776E-16, -0.2660368455666826670 ) ) ;
#34798 = DIRECTION ( 'NONE',  ( 1.000000000000000000, 0.000000000000000000, 0.000000000000000000 ) ) ;
#34799 = ORIENTED_EDGE ( 'NONE', *, *, #22947, .T. ) ;
#34800 = ORIENTED_EDGE ( 'NONE', *, *, #7130, .F. ) ;
#34801 = EDGE_LOOP ( 'NONE', ( #30034, #26814, #9300, #38510 ) ) ;
#34802 = DIRECTION ( 'NONE',  ( -1.000000000000000000, 0.000000000000000000, 0.000000000000000000 ) ) ;
#34803 = ORIENTED_EDGE ( 'NONE', *, *, #30525, .F. ) ;
#34804 = CARTESIAN_POINT ( 'NONE',  ( 3.616083068348484413E-16, 2.362204724409439294, 2.952755905511811552 ) ) ;
#34805 = CARTESIAN_POINT ( 'NONE',  ( 0.000000000000000000, 3.267716535433071279, 0.000000000000000000 ) ) ;
#34806 = ADVANCED_FACE ( 'NONE', ( #15364 ), #19476, .F. ) ;
#34807 = EDGE_LOOP ( 'NONE', ( #15336, #13433, #20434, #39776 ) ) ;
#34808 = CARTESIAN_POINT ( 'NONE',  ( 0.4696143004045479352, 3.346456692913386100, 0.1574803149606283648 ) ) ;
#34809 = CARTESIAN_POINT ( 'NONE',  ( -1.636583440222564301, 0.000000000000000000, -1.456692913385822186 ) ) ;
#34810 = ORIENTED_EDGE ( 'NONE', *, *, #8466, .T. ) ;
#34811 = VERTEX_POINT ( 'NONE', #34485 ) ;
#34812 = LINE ( 'NONE', #45392, #10068 ) ;
#34813 = FACE_BOUND ( 'NONE', #17474, .T. ) ;
#34814 = VERTEX_POINT ( 'NONE', #31113 ) ;
#34815 = AXIS2_PLACEMENT_3D ( 'NONE', #10817, #26560, #42064 ) ;
#34816 = LINE ( 'NONE', #50258, #17983 ) ;
#34817 = ORIENTED_EDGE ( 'NONE', *, *, #43598, .T. ) ;
#34818 = ORIENTED_EDGE ( 'NONE', *, *, #47230, .T. ) ;
#34819 = PLANE ( 'NONE',  #21624 ) ;
#34820 = VECTOR ( 'NONE', #24724, 39.37007874015748143 ) ;
#34821 = EDGE_CURVE ( 'NONE', #44668, #23557, #23105, .T. ) ;
#34822 = DIRECTION ( 'NONE',  ( -0.6631698831091616952, -0.000000000000000000, 0.7484689079293679326 ) ) ;
#34823 = ORIENTED_EDGE ( 'NONE', *, *, #25610, .T. ) ;
#34824 = AXIS2_PLACEMENT_3D ( 'NONE', #11261, #26993, #7390 ) ;
#34825 = CARTESIAN_POINT ( 'NONE',  ( 2.160407304981128984, 2.755905511811027164, -0.1462862061266579361 ) ) ;
#34826 = ORIENTED_EDGE ( 'NONE', *, *, #235, .F. ) ;
#34827 = CARTESIAN_POINT ( 'NONE',  ( 0.7423782071083092626, 3.346456692913386100, 1.889763779527550369 ) ) ;
#34828 = EDGE_CURVE ( 'NONE', #4909, #12116, #19218, .T. ) ;
#34829 = VECTOR ( 'NONE', #12426, 39.37007874015748143 ) ;
#34830 = FACE_OUTER_BOUND ( 'NONE', #46361, .T. ) ;
#34831 = EDGE_CURVE ( 'NONE', #42424, #24628, #42720, .T. ) ;
#34832 = EDGE_CURVE ( 'NONE', #49027, #24066, #4897, .T. ) ;
#34833 = LINE ( 'NONE', #15207, #38761 ) ;
#34834 = ORIENTED_EDGE ( 'NONE', *, *, #39435, .T. ) ;
#34835 = ORIENTED_EDGE ( 'NONE', *, *, #38218, .F. ) ;
#34836 = DIRECTION ( 'NONE',  ( -0.000000000000000000, 1.000000000000000000, -0.000000000000000000 ) ) ;
#34837 = CARTESIAN_POINT ( 'NONE',  ( -1.091055626815042645, 0.000000000000000000, -0.9448818897637760728 ) ) ;
#34838 = CARTESIAN_POINT ( 'NONE',  ( -0.5304089168012655620, 0.01942419597810423823, -1.736909402037482675 ) ) ;
#34839 = DIRECTION ( 'NONE',  ( -0.6234898018587319291, -1.160734090543304907E-16, -0.7818314824680311359 ) ) ;
#34840 = LINE ( 'NONE', #38962, #17385 ) ;
#34841 = CARTESIAN_POINT ( 'NONE',  ( 1.319349709118413205, 0.000000000000000000, 1.584915398547334764 ) ) ;
#34842 = ADVANCED_FACE ( 'NONE', ( #3231 ), #26224, .F. ) ;
#34843 = FACE_OUTER_BOUND ( 'NONE', #14191, .T. ) ;
#34844 = EDGE_LOOP ( 'NONE', ( #30655, #38817, #47236, #33868 ) ) ;
#34845 = CARTESIAN_POINT ( 'NONE',  ( 1.833433833923350909, 3.267716535433071279, -1.456692913385823296 ) ) ;
#34846 = CARTESIAN_POINT ( 'NONE',  ( 0.000000000000000000, 3.267716535433071279, 0.4724409448818869817 ) ) ;
#34847 = EDGE_CURVE ( 'NONE', #43448, #37038, #2987, .T. ) ;
#34848 = VERTEX_POINT ( 'NONE', #11490 ) ;
#34849 = ORIENTED_EDGE ( 'NONE', *, *, #22914, .F. ) ;
#34850 = PLANE ( 'NONE',  #38262 ) ;
#34851 = CIRCLE ( 'NONE', #12591, 1.743387098533651480 ) ;
#34852 = DIRECTION ( 'NONE',  ( -3.986037398843765983E-20, -1.000000000000000000, -1.160734090543304660E-16 ) ) ;
#34853 = ORIENTED_EDGE ( 'NONE', *, *, #19408, .T. ) ;
#34854 = EDGE_CURVE ( 'NONE', #24511, #14359, #42962, .T. ) ;
#34855 = AXIS2_PLACEMENT_3D ( 'NONE', #21807, #45267, #17169 ) ;
#34856 = CARTESIAN_POINT ( 'NONE',  ( 0.8449282472259149745, 1.688626626580369994, 2.111245994233534429 ) ) ;
#34857 = ORIENTED_EDGE ( 'NONE', *, *, #37760, .F. ) ;
#34858 = DIRECTION ( 'NONE',  ( -0.000000000000000000, 1.000000000000000000, -0.000000000000000000 ) ) ;
#34859 = VECTOR ( 'NONE', #18947, 39.37007874015748143 ) ;
#34860 = EDGE_CURVE ( 'NONE', #4117, #33862, #19729, .T. ) ;
#34861 = EDGE_LOOP ( 'NONE', ( #37318, #50111, #10564, #18599 ) ) ;
#34862 = VECTOR ( 'NONE', #37261, 39.37007874015748143 ) ;
#34863 = VECTOR ( 'NONE', #24892, 39.37007874015748143 ) ;
#34864 = PLANE ( 'NONE',  #10355 ) ;
#34865 = FACE_OUTER_BOUND ( 'NONE', #27999, .T. ) ;
#34866 = ORIENTED_EDGE ( 'NONE', *, *, #25741, .T. ) ;
#34867 = CIRCLE ( 'NONE', #31595, 1.743387098533651480 ) ;
#34868 = DIRECTION ( 'NONE',  ( 0.000000000000000000, 1.000000000000000000, -0.000000000000000000 ) ) ;
#34869 = EDGE_LOOP ( 'NONE', ( #34060, #24242, #49510, #3530 ) ) ;
#34870 = VERTEX_POINT ( 'NONE', #47573 ) ;
#34871 = EDGE_CURVE ( 'NONE', #44433, #35684, #43219, .T. ) ;
#34872 = CARTESIAN_POINT ( 'NONE',  ( 3.519654186525858491E-16, 2.344748451760389596, 2.874015748031496731 ) ) ;
#34873 = CARTESIAN_POINT ( 'NONE',  ( -1.420868632364155282, 0.000000000000000000, 1.070159647439151707 ) ) ;
#34874 = DIRECTION ( 'NONE',  ( 0.000000000000000000, 0.000000000000000000, -1.000000000000000000 ) ) ;
#34875 = EDGE_CURVE ( 'NONE', #41125, #1816, #27730, .T. ) ;
#34876 = ORIENTED_EDGE ( 'NONE', *, *, #11756, .T. ) ;
#34877 = CARTESIAN_POINT ( 'NONE',  ( -2.151809081513409438, 1.574803149606302854, 0.2418202932658341242 ) ) ;
#34878 = CARTESIAN_POINT ( 'NONE',  ( 0.002207914879453961535, -5.712274067634378313E-18, 0.04916304461325374242 ) ) ;
#34879 = ORIENTED_EDGE ( 'NONE', *, *, #40059, .F. ) ;
#34880 = CARTESIAN_POINT ( 'NONE',  ( 0.000000000000000000, 1.574803149606302854, 0.000000000000000000 ) ) ;
#34881 = ORIENTED_EDGE ( 'NONE', *, *, #30819, .F. ) ;
#34882 = ORIENTED_EDGE ( 'NONE', *, *, #22351, .T. ) ;
#34883 = CARTESIAN_POINT ( 'NONE',  ( 2.213833626531446441, 33.40587228752335136, 73.35348184813385330 ) ) ;
#34884 = VERTEX_POINT ( 'NONE', #44246 ) ;
#34885 = DIRECTION ( 'NONE',  ( 0.000000000000000000, 1.000000000000000000, 0.000000000000000000 ) ) ;
#34886 = ADVANCED_FACE ( 'NONE', ( #631 ), #35490, .F. ) ;
#34887 = CARTESIAN_POINT ( 'NONE',  ( 1.539674616754186820, 0.000000000000000000, -1.403993126671013059 ) ) ;
#34888 = CARTESIAN_POINT ( 'NONE',  ( 1.979793062125284608, 1.651646828087945051, 2.191257344206569257 ) ) ;
#34889 = ADVANCED_FACE ( 'NONE', ( #31616 ), #23866, .F. ) ;
#34890 = DIRECTION ( 'NONE',  ( -3.469446951953613696E-16, 0.000000000000000000, -1.000000000000000000 ) ) ;
#34891 = ORIENTED_EDGE ( 'NONE', *, *, #38383, .F. ) ;
#34892 = ORIENTED_EDGE ( 'NONE', *, *, #23847, .F. ) ;
#34893 = AXIS2_PLACEMENT_3D ( 'NONE', #31510, #16010, #12652 ) ;
#34894 = LINE ( 'NONE', #20148, #50147 ) ;
#34895 = LINE ( 'NONE', #30768, #21862 ) ;
#34896 = VECTOR ( 'NONE', #47314, 39.37007874015748143 ) ;
#34897 = ORIENTED_EDGE ( 'NONE', *, *, #22195, .F. ) ;
#34898 = FACE_OUTER_BOUND ( 'NONE', #6116, .T. ) ;
#34899 = LINE ( 'NONE', #41887, #15213 ) ;
#34900 = VECTOR ( 'NONE', #50323, 39.37007874015748143 ) ;
#34901 = VECTOR ( 'NONE', #36623, 39.37007874015748143 ) ;
#34902 = CARTESIAN_POINT ( 'NONE',  ( 0.000000000000000000, 3.346456692913386100, 0.000000000000000000 ) ) ;
#34903 = LINE ( 'NONE', #42383, #17027 ) ;
#34904 = CARTESIAN_POINT ( 'NONE',  ( -2.454875160333845674, 0.000000000000000000, -0.03937007874015881204 ) ) ;
#34905 = VECTOR ( 'NONE', #14270, 39.37007874015748143 ) ;
#34906 = ORIENTED_EDGE ( 'NONE', *, *, #45770, .F. ) ;
#34907 = CARTESIAN_POINT ( 'NONE',  ( 1.902660579019252562, 1.639951345248664039, -1.314902632263422966 ) ) ;
#34908 = DIRECTION ( 'NONE',  ( 0.000000000000000000, 1.000000000000000000, 0.000000000000000000 ) ) ;
#34909 = EDGE_LOOP ( 'NONE', ( #20345, #36736, #21814, #50371 ) ) ;
#34910 = CARTESIAN_POINT ( 'NONE',  ( -2.734482843737247038, 1.572033689214636709, -1.115254632218712016 ) ) ;
#34911 = CARTESIAN_POINT ( 'NONE',  ( 0.4696143004045479907, 3.267716535433071279, -1.629301903132387999E-16 ) ) ;
#34912 = CARTESIAN_POINT ( 'NONE',  ( 0.1067246931122726866, 0.02962905676920215767, 0.000000000000000000 ) ) ;
#34913 = EDGE_LOOP ( 'NONE', ( #5488, #31823, #12963, #30449 ) ) ;
#34914 = EDGE_CURVE ( 'NONE', #25659, #46790, #36262, .T. ) ;
#34915 = EDGE_LOOP ( 'NONE', ( #37576, #25883, #12246, #8980 ) ) ;
#34916 = CARTESIAN_POINT ( 'NONE',  ( -2.071704270381554913, 3.346456692913386100, -0.6299212598425177889 ) ) ;
#34917 = ORIENTED_EDGE ( 'NONE', *, *, #49254, .F. ) ;
#34918 = LINE ( 'NONE', #31554, #23710 ) ;
#34919 = EDGE_CURVE ( 'NONE', #3939, #41046, #5012, .T. ) ;
#34920 = ORIENTED_EDGE ( 'NONE', *, *, #11862, .T. ) ;
#34921 = CARTESIAN_POINT ( 'NONE',  ( 2.010699302595137627, 0.01941208527870304928, -0.5094071868683279769 ) ) ;
#34922 = CARTESIAN_POINT ( 'NONE',  ( -1.439733046521776361, 3.267716535433071279, 4.995077429881866871E-16 ) ) ;
#34923 = CARTESIAN_POINT ( 'NONE',  ( 2.182111253630085290, 3.346456692913386100, 0.6299212598425161236 ) ) ;
#34924 = EDGE_CURVE ( 'NONE', #919, #15390, #32136, .T. ) ;
#34925 = EDGE_CURVE ( 'NONE', #10877, #22183, #110, .T. ) ;
#34926 = ORIENTED_EDGE ( 'NONE', *, *, #7355, .T. ) ;
#34927 = VECTOR ( 'NONE', #45710, 39.37007874015748143 ) ;
#34928 = ORIENTED_EDGE ( 'NONE', *, *, #49872, .F. ) ;
#34929 = ORIENTED_EDGE ( 'NONE', *, *, #38216, .T. ) ;
#34930 = LINE ( 'NONE', #34182, #47898 ) ;
#34931 = FACE_OUTER_BOUND ( 'NONE', #20619, .T. ) ;
#34932 = ORIENTED_EDGE ( 'NONE', *, *, #32360, .T. ) ;
#34933 = ORIENTED_EDGE ( 'NONE', *, *, #13789, .F. ) ;
#34934 = AXIS2_PLACEMENT_3D ( 'NONE', #34546, #46132, #49474 ) ;
#34935 = CARTESIAN_POINT ( 'NONE',  ( -2.142805232260984738, 5.905511811023623991, 0.3399247426648309700 ) ) ;
#34936 = LINE ( 'NONE', #34437, #12082 ) ;
#34937 = DIRECTION ( 'NONE',  ( -1.000000000000000000, 0.000000000000000000, 1.734723475976806848E-16 ) ) ;
#34938 = VECTOR ( 'NONE', #4349, 39.37007874015748143 ) ;
#34939 = CONICAL_SURFACE ( 'NONE', #7699, 2.246510896728926010, 0.01601546068027819014 ) ;
#34940 = ORIENTED_EDGE ( 'NONE', *, *, #25507, .F. ) ;
#34941 = EDGE_LOOP ( 'NONE', ( #23754, #33030, #16635, #24093 ) ) ;
#34942 = DIRECTION ( 'NONE',  ( 1.000000000000000000, 0.000000000000000000, -3.469446951953613696E-16 ) ) ;
#34943 = CARTESIAN_POINT ( 'NONE',  ( 4.268512490100411402E-16, 0.000000000000000000, 0.9448818897637749625 ) ) ;
#34944 = FACE_OUTER_BOUND ( 'NONE', #11047, .T. ) ;
#34945 = EDGE_CURVE ( 'NONE', #43549, #45835, #7865, .T. ) ;
#34946 = ORIENTED_EDGE ( 'NONE', *, *, #31871, .F. ) ;
#34947 = CARTESIAN_POINT ( 'NONE',  ( 0.000000000000000000, 5.905511811023623991, 0.000000000000000000 ) ) ;
#34948 = CARTESIAN_POINT ( 'NONE',  ( -0.07591351300297333182, 3.267716535433071279, -0.1574803149606301411 ) ) ;
#34949 = CIRCLE ( 'NONE', #34146, 2.164630168518208109 ) ;
#34950 = ORIENTED_EDGE ( 'NONE', *, *, #21768, .T. ) ;
#34951 = DIRECTION ( 'NONE',  ( -0.9998717552508122886, -0.01601477604151181275, 0.000000000000000000 ) ) ;
#34952 = ORIENTED_EDGE ( 'NONE', *, *, #3327, .T. ) ;
#34953 = EDGE_LOOP ( 'NONE', ( #21238, #13721, #49178, #42815 ) ) ;
#34954 = LINE ( 'NONE', #31585, #21307 ) ;
#34955 = DIRECTION ( 'NONE',  ( -0.000000000000000000, 1.000000000000000000, -0.000000000000000000 ) ) ;
#34956 = EDGE_CURVE ( 'NONE', #42980, #29226, #39359, .T. ) ;
#34957 = LINE ( 'NONE', #8088, #39571 ) ;
#34958 = CYLINDRICAL_SURFACE ( 'NONE', #17038, 2.106299212598425008 ) ;
#34959 = ADVANCED_FACE ( 'NONE', ( #31366 ), #28237, .F. ) ;
#34960 = ADVANCED_FACE ( 'NONE', ( #43469 ), #32391, .F. ) ;
#34961 = LINE ( 'NONE', #50638, #21377 ) ;
#34962 = ORIENTED_EDGE ( 'NONE', *, *, #33712, .T. ) ;
#34963 = VERTEX_POINT ( 'NONE', #4243 ) ;
#34964 = DIRECTION ( 'NONE',  ( -1.000000000000000000, -0.000000000000000000, -0.000000000000000000 ) ) ;
#34965 = CARTESIAN_POINT ( 'NONE',  ( 0.000000000000000000, 3.267716535433071279, -0.4724409448818884805 ) ) ;
#34966 = DIRECTION ( 'NONE',  ( -0.000000000000000000, 1.000000000000000000, -0.000000000000000000 ) ) ;
#34967 = VECTOR ( 'NONE', #34327, 39.37007874015748143 ) ;
#34968 = FACE_OUTER_BOUND ( 'NONE', #31626, .T. ) ;
#34969 = CARTESIAN_POINT ( 'NONE',  ( -0.8942052331142545940, 3.267716535433071279, 3.102397620449221495E-16 ) ) ;
#34970 = ORIENTED_EDGE ( 'NONE', *, *, #22978, .T. ) ;
#34971 = CIRCLE ( 'NONE', #19289, 2.244934639244525076 ) ;
#34972 = CARTESIAN_POINT ( 'NONE',  ( -0.04921259842519706829, 1.707113721008201024, 2.241222193722145484 ) ) ;
#34973 = AXIS2_PLACEMENT_3D ( 'NONE', #48063, #17629, #33134 ) ;
#34974 = DIRECTION ( 'NONE',  ( -3.469446951953613696E-16, 0.000000000000000000, -1.000000000000000000 ) ) ;
#34975 = VECTOR ( 'NONE', #32909, 39.37007874015748143 ) ;
#34976 = AXIS2_PLACEMENT_3D ( 'NONE', #31230, #23723, #27336 ) ;
#34977 = ORIENTED_EDGE ( 'NONE', *, *, #4647, .T. ) ;
#34978 = DIRECTION ( 'NONE',  ( -0.000000000000000000, 0.000000000000000000, 1.000000000000000000 ) ) ;
#34979 = CARTESIAN_POINT ( 'NONE',  ( -0.2492758785930729581, 1.703909341437327862, -2.220674960591680680 ) ) ;
#34980 = CARTESIAN_POINT ( 'NONE',  ( -2.889674983507169337, 1.575089141731351505, -0.6090712660038034576 ) ) ;
#34981 = CARTESIAN_POINT ( 'NONE',  ( 0.2727639067037610499, 0.000000000000000000, 1.417322834645662777 ) ) ;
#34982 = DIRECTION ( 'NONE',  ( 0.000000000000000000, 0.000000000000000000, -1.000000000000000000 ) ) ;
#34983 = LINE ( 'NONE', #42468, #24392 ) ;
#34984 = VECTOR ( 'NONE', #25263, 39.37007874015748143 ) ;
#34985 = ORIENTED_EDGE ( 'NONE', *, *, #1893, .T. ) ;
#34986 = CARTESIAN_POINT ( 'NONE',  ( -1.022004635462139488, 1.695497469272269964, -2.235637960992456819 ) ) ;
#34987 = EDGE_LOOP ( 'NONE', ( #7304, #44621, #30442, #21168, #3288, #34078, #19054, #7838, #23797, #20797, #10196 ) ) ;
#34988 = DIRECTION ( 'NONE',  ( 1.734723475976806848E-16, 0.000000000000000000, 1.000000000000000000 ) ) ;
#34989 = DIRECTION ( 'NONE',  ( -1.000000000000000000, -0.000000000000000000, -0.000000000000000000 ) ) ;
#34990 = CARTESIAN_POINT ( 'NONE',  ( 0.000000000000000000, 3.267716535433071279, 0.3149606299212576177 ) ) ;
#34991 = EDGE_CURVE ( 'NONE', #45413, #15688, #12766, .T. ) ;
#34992 = EDGE_CURVE ( 'NONE', #17453, #18200, #20506, .T. ) ;
#34993 = ADVANCED_FACE ( 'NONE', ( #12247, #40133, #31884, #4759, #43722, #24121, #20239, #1132 ), #29528, .F. ) ;
#34994 = ORIENTED_EDGE ( 'NONE', *, *, #35217, .F. ) ;
#34995 = ORIENTED_EDGE ( 'NONE', *, *, #7786, .F. ) ;
#34996 = CARTESIAN_POINT ( 'NONE',  ( 1.474379988472116487, 1.633091647787944911, 1.762361831087230213 ) ) ;
#34997 = CARTESIAN_POINT ( 'NONE',  ( -2.411880484304812278, 1.575048720448358752, 0.2770493584408288412 ) ) ;
#34998 = CARTESIAN_POINT ( 'NONE',  ( -0.3486774197067339376, 0.000000000000000000, -0.6299212598425175669 ) ) ;
#34999 = DIRECTION ( 'NONE',  ( 0.000000000000000000, 0.000000000000000000, -1.000000000000000000 ) ) ;
#35000 = CARTESIAN_POINT ( 'NONE',  ( 0.5455278134075212115, 3.267716535433071279, -9.463399047163220715E-17 ) ) ;
#35001 = ADVANCED_FACE ( 'NONE', ( #25905 ), #41655, .F. ) ;
#35002 = CARTESIAN_POINT ( 'NONE',  ( 1.636583440222563857, 3.267716535433071279, 0.7480314960629872445 ) ) ;
#35003 = ORIENTED_EDGE ( 'NONE', *, *, #39996, .F. ) ;
#35004 = CARTESIAN_POINT ( 'NONE',  ( 0.08139965876239094178, 1.610780518492231694, 0.000000000000000000 ) ) ;
#35005 = CARTESIAN_POINT ( 'NONE',  ( 0.1067246931122726866, 0.02962905676920215767, 0.000000000000000000 ) ) ;
#35006 = VECTOR ( 'NONE', #47797, 39.37007874015748143 ) ;
#35007 = CARTESIAN_POINT ( 'NONE',  ( -1.166969139818015977, 3.346456692913386100, -0.7874015748031470974 ) ) ;
#35008 = AXIS2_PLACEMENT_3D ( 'NONE', #8354, #39337, #88 ) ;
#35009 = ORIENTED_EDGE ( 'NONE', *, *, #20336, .T. ) ;
#35010 = DIRECTION ( 'NONE',  ( 0.01601477604151182663, -0.9998717552508123996, 0.000000000000000000 ) ) ;
#35011 = VECTOR ( 'NONE', #3398, 39.37007874015748143 ) ;
#35012 = ORIENTED_EDGE ( 'NONE', *, *, #27302, .F. ) ;
#35013 = EDGE_LOOP ( 'NONE', ( #35380, #17985, #19233, #32093 ) ) ;
#35014 = EDGE_CURVE ( 'NONE', #36931, #24770, #36769, .T. ) ;
#35015 = VECTOR ( 'NONE', #19791, 39.37007874015748143 ) ;
#35016 = AXIS2_PLACEMENT_3D ( 'NONE', #36629, #21138, #33026 ) ;
#35017 = ADVANCED_FACE ( 'NONE', ( #13019 ), #45496, .F. ) ;
#35018 = VERTEX_POINT ( 'NONE', #45245 ) ;
#35019 = ORIENTED_EDGE ( 'NONE', *, *, #19024, .F. ) ;
#35020 = LINE ( 'NONE', #50696, #26875 ) ;
#35021 = EDGE_CURVE ( 'NONE', #25300, #9567, #7430, .T. ) ;
#35022 = EDGE_LOOP ( 'NONE', ( #27731, #12005, #29999, #9052, #13870, #23595, #31576, #34471, #40156, #45361, #33192 ) ) ;
#35023 = CIRCLE ( 'NONE', #16067, 2.443628662382284489 ) ;
#35024 = EDGE_CURVE ( 'NONE', #19298, #30179, #37028, .T. ) ;
#35025 = LINE ( 'NONE', #15400, #35343 ) ;
#35026 = EDGE_CURVE ( 'NONE', #596, #21677, #40721, .T. ) ;
#35027 = PLANE ( 'NONE',  #38444 ) ;
#35028 = CARTESIAN_POINT ( 'NONE',  ( -1.919487379551519490, 0.5250046931542878825, 0.9770346176326605292 ) ) ;
#35029 = CARTESIAN_POINT ( 'NONE',  ( 2.734482843737263025, 1.452693199995327644, -1.115254632218672270 ) ) ;
#35030 = DIRECTION ( 'NONE',  ( 1.000000000000000000, -0.000000000000000000, 0.000000000000000000 ) ) ;
#35031 = CARTESIAN_POINT ( 'NONE',  ( 1.560669927219590525, 3.346456692913386100, 0.9055118110236164419 ) ) ;
#35032 = VERTEX_POINT ( 'NONE', #9140 ) ;
#35033 = DIRECTION ( 'NONE',  ( 1.734723475976806848E-16, -0.000000000000000000, 1.000000000000000000 ) ) ;
#35034 = LINE ( 'NONE', #7410, #25875 ) ;
#35035 = DIRECTION ( 'NONE',  ( -0.000000000000000000, 0.000000000000000000, 1.000000000000000000 ) ) ;
#35036 = CARTESIAN_POINT ( 'NONE',  ( 0.000000000000000000, 3.267716535433071279, 0.1181102362204704270 ) ) ;
#35037 = VERTEX_POINT ( 'NONE', #32653 ) ;
#35038 = CARTESIAN_POINT ( 'NONE',  ( 4.200216290258821831E-16, 3.346456692913386100, 2.165354330708661568 ) ) ;
#35039 = DIRECTION ( 'NONE',  ( 7.097135778201662695E-17, 1.000000000000000000, -1.075170113095010447E-16 ) ) ;
#35040 = ORIENTED_EDGE ( 'NONE', *, *, #17111, .T. ) ;
#35041 = CARTESIAN_POINT ( 'NONE',  ( -1.181102362204724088, 0.5905511811023621549, 1.062992125984251413 ) ) ;
#35042 = CARTESIAN_POINT ( 'NONE',  ( -1.632855683316659867, 1.205361022782829114E-17, -0.6443965869051290207 ) ) ;
#35043 = VECTOR ( 'NONE', #46978, 39.37007874015748143 ) ;
#35044 = VECTOR ( 'NONE', #25762, 39.37007874015748143 ) ;
#35045 = DIRECTION ( 'NONE',  ( -1.000000000000000000, -0.000000000000000000, -0.000000000000000000 ) ) ;
#35046 = ORIENTED_EDGE ( 'NONE', *, *, #22933, .T. ) ;
#35047 = LINE ( 'NONE', #4309, #44572 ) ;
#35048 = VECTOR ( 'NONE', #15617, 39.37007874015748143 ) ;
#35049 = DIRECTION ( 'NONE',  ( 0.000000000000000000, 0.000000000000000000, -1.000000000000000000 ) ) ;
#35050 = CARTESIAN_POINT ( 'NONE',  ( 0.8182917201112817063, 3.346456692913386100, -1.732283464566923614 ) ) ;
#35051 = CARTESIAN_POINT ( 'NONE',  ( -1.439733046521776583, 3.346456692913386100, -1.617383112398506295 ) ) ;
#35052 = EDGE_LOOP ( 'NONE', ( #15056, #14626, #11714, #29094 ) ) ;
#35053 = EDGE_CURVE ( 'NONE', #50445, #9022, #43809, .T. ) ;
#35054 = AXIS2_PLACEMENT_3D ( 'NONE', #44504, #12253, #9148 ) ;
#35055 = ORIENTED_EDGE ( 'NONE', *, *, #7195, .F. ) ;
#35056 = ORIENTED_EDGE ( 'NONE', *, *, #37933, .T. ) ;
#35057 = EDGE_CURVE ( 'NONE', #45880, #50600, #33420, .T. ) ;
#35058 = DIRECTION ( 'NONE',  ( -3.986037398843765983E-20, -1.000000000000000000, -1.160734090543304660E-16 ) ) ;
#35059 = ORIENTED_EDGE ( 'NONE', *, *, #12182, .T. ) ;
#35060 = DIRECTION ( 'NONE',  ( 1.000000000000000000, 0.000000000000000000, 0.000000000000000000 ) ) ;
#35061 = CARTESIAN_POINT ( 'NONE',  ( -0.04921259842519767197, 6.692913385826772199, 2.164795024401847456 ) ) ;
#35062 = ORIENTED_EDGE ( 'NONE', *, *, #25476, .T. ) ;
#35063 = EDGE_CURVE ( 'NONE', #22677, #44810, #13275, .T. ) ;
#35064 = CARTESIAN_POINT ( 'NONE',  ( -1.117755760306017088, 0.3937007874015748254, -2.093391932325144326E-16 ) ) ;
#35065 = VERTEX_POINT ( 'NONE', #25393 ) ;
#35066 = CARTESIAN_POINT ( 'NONE',  ( 0.08119777152254364916, 1.623385212329073957, 0.000000000000000000 ) ) ;
#35067 = VERTEX_POINT ( 'NONE', #5524 ) ;
#35068 = ORIENTED_EDGE ( 'NONE', *, *, #12069, .F. ) ;
#35069 = LINE ( 'NONE', #28071, #36415 ) ;
#35070 = VERTEX_POINT ( 'NONE', #37541 ) ;
#35071 = CARTESIAN_POINT ( 'NONE',  ( -0.8942052331142547050, 0.000000000000000000, 0.6299212598425164567 ) ) ;
#35072 = EDGE_CURVE ( 'NONE', #30518, #13474, #21273, .T. ) ;
#35073 = ORIENTED_EDGE ( 'NONE', *, *, #25653, .F. ) ;
#35074 = ORIENTED_EDGE ( 'NONE', *, *, #37532, .T. ) ;
#35075 = DIRECTION ( 'NONE',  ( 0.000000000000000000, 1.000000000000000000, 0.000000000000000000 ) ) ;
#35076 = VECTOR ( 'NONE', #45104, 39.37007874015748143 ) ;
#35077 = EDGE_CURVE ( 'NONE', #31986, #50925, #22886, .T. ) ;
#35078 = CARTESIAN_POINT ( 'NONE',  ( -1.195183497228115035E-16, 3.346456692913386100, -1.574803149606293529 ) ) ;
#35079 = CONICAL_SURFACE ( 'NONE', #21049, 2.244934639244524632, 1.554780866114618743 ) ;
#35080 = ADVANCED_FACE ( 'NONE', ( #37285 ), #17397, .F. ) ;
#35081 = VERTEX_POINT ( 'NONE', #9654 ) ;
#35082 = DIRECTION ( 'NONE',  ( -3.469446951953613696E-16, 0.000000000000000000, -1.000000000000000000 ) ) ;
#35083 = AXIS2_PLACEMENT_3D ( 'NONE', #22540, #42660, #7305 ) ;
#35084 = EDGE_LOOP ( 'NONE', ( #6630, #25639, #33452, #36858 ) ) ;
#35085 = DIRECTION ( 'NONE',  ( -0.000000000000000000, 1.000000000000000000, -0.000000000000000000 ) ) ;
#35086 = DIRECTION ( 'NONE',  ( 0.000000000000000000, 1.000000000000000000, 0.000000000000000000 ) ) ;
#35087 = VECTOR ( 'NONE', #24005, 39.37007874015748143 ) ;
#35088 = CARTESIAN_POINT ( 'NONE',  ( 2.378961647330872786, 3.346456692913386100, 0.6299212598425161236 ) ) ;
#35089 = ORIENTED_EDGE ( 'NONE', *, *, #2423, .F. ) ;
#35090 = ORIENTED_EDGE ( 'NONE', *, *, #7824, .F. ) ;
#35091 = AXIS2_PLACEMENT_3D ( 'NONE', #45385, #18047, #33808 ) ;
#35092 = DIRECTION ( 'NONE',  ( 0.9909497617679331460, 0.000000000000000000, 0.1342332658176667026 ) ) ;
#35093 = FACE_OUTER_BOUND ( 'NONE', #24592, .T. ) ;
#35094 = DIRECTION ( 'NONE',  ( -3.469446951953613696E-16, 0.000000000000000000, -1.000000000000000000 ) ) ;
#35095 = CARTESIAN_POINT ( 'NONE',  ( -0.5455278134075213226, 3.267716535433071279, 9.463399047163221947E-17 ) ) ;
#35096 = DIRECTION ( 'NONE',  ( -0.000000000000000000, 0.000000000000000000, 1.000000000000000000 ) ) ;
#35097 = LINE ( 'NONE', #26580, #7841 ) ;
#35098 = LINE ( 'NONE', #35862, #7732 ) ;
#35099 = ORIENTED_EDGE ( 'NONE', *, *, #46492, .T. ) ;
#35100 = CARTESIAN_POINT ( 'NONE',  ( 2.182111253630085290, 0.000000000000000000, -1.161035397307311917E-15 ) ) ;
#35101 = ORIENTED_EDGE ( 'NONE', *, *, #3780, .F. ) ;
#35102 = ORIENTED_EDGE ( 'NONE', *, *, #16410, .F. ) ;
#35103 = LINE ( 'NONE', #42833, #29998 ) ;
#35104 = LINE ( 'NONE', #496, #36075 ) ;
#35105 = ORIENTED_EDGE ( 'NONE', *, *, #10238, .F. ) ;
#35106 = AXIS2_PLACEMENT_3D ( 'NONE', #45427, #21970, #28676 ) ;
#35107 = CARTESIAN_POINT ( 'NONE',  ( 0.000000000000000000, 3.267716535433071279, -0.1574803149606298636 ) ) ;
#35108 = EDGE_CURVE ( 'NONE', #17272, #42090, #49099, .T. ) ;
#35109 = AXIS2_PLACEMENT_3D ( 'NONE', #6354, #48904, #13593 ) ;
#35110 = ORIENTED_EDGE ( 'NONE', *, *, #1761, .T. ) ;
#35111 = CARTESIAN_POINT ( 'NONE',  ( -0.07591351300297277671, 3.346456692913386100, 0.7874015748031456541 ) ) ;
#35112 = AXIS2_PLACEMENT_3D ( 'NONE', #24905, #44000, #16137 ) ;
#35113 = VERTEX_POINT ( 'NONE', #6026 ) ;
#35114 = EDGE_CURVE ( 'NONE', #17408, #810, #2158, .T. ) ;
#35115 = DIRECTION ( 'NONE',  ( 3.586865599282426309E-17, -1.000000000000000000, -1.103923720497134591E-16 ) ) ;
#35116 = CARTESIAN_POINT ( 'NONE',  ( 0.000000000000000000, 3.267716535433071279, 2.204724409448808764 ) ) ;
#35117 = EDGE_CURVE ( 'NONE', #28628, #3517, #22292, .T. ) ;
#35118 = VECTOR ( 'NONE', #1611, 39.37007874015748143 ) ;
#35119 = EDGE_CURVE ( 'NONE', #29278, #20848, #31044, .T. ) ;
#35120 = ORIENTED_EDGE ( 'NONE', *, *, #34645, .T. ) ;
#35121 = VECTOR ( 'NONE', #49364, 39.37007874015748143 ) ;
#35123 = LINE ( 'NONE', #50800, #42035 ) ;
#35122 = B_SPLINE_CURVE_WITH_KNOTS ( 'NONE', 3,
 ( #48867, #13553, #21808, #45026 ),
 .UNSPECIFIED., .F., .F.,
 ( 4, 4 ),
 ( 2.396442697539120721E-07, 0.01971986562029358347 ),
 .UNSPECIFIED. ) ;
#35124 = EDGE_LOOP ( 'NONE', ( #20543, #29714, #13865, #19066 ) ) ;
#35125 = ORIENTED_EDGE ( 'NONE', *, *, #22092, .F. ) ;
#35126 = LINE ( 'NONE', #41858, #10318 ) ;
#35127 = CARTESIAN_POINT ( 'NONE',  ( 0.1968503937007875237, 3.267716535433071279, -6.829619984160660511E-17 ) ) ;
#35128 = FACE_OUTER_BOUND ( 'NONE', #1594, .T. ) ;
#35129 = ORIENTED_EDGE ( 'NONE', *, *, #13289, .F. ) ;
#35130 = DIRECTION ( 'NONE',  ( -0.9998717552508122886, -0.01601477604151180928, 0.000000000000000000 ) ) ;
#35131 = ADVANCED_FACE ( 'NONE', ( #22793 ), #22537, .T. ) ;
#35132 = DIRECTION ( 'NONE',  ( -0.9998717552508122886, -0.01601477604151180928, 0.000000000000000000 ) ) ;
#35133 = ORIENTED_EDGE ( 'NONE', *, *, #21209, .T. ) ;
#35134 = CARTESIAN_POINT ( 'NONE',  ( -1.636583440222564301, 3.346456692913386100, -1.456692913385822186 ) ) ;
#35135 = EDGE_CURVE ( 'NONE', #6369, #2307, #18414, .T. ) ;
#35136 = ORIENTED_EDGE ( 'NONE', *, *, #28824, .T. ) ;
#35137 = ORIENTED_EDGE ( 'NONE', *, *, #38847, .F. ) ;
#35138 = DIRECTION ( 'NONE',  ( 0.4357934065752705477, -0.2785571346213377986, -0.8558563136047258046 ) ) ;
#35139 = ORIENTED_EDGE ( 'NONE', *, *, #30289, .T. ) ;
#35140 = FACE_OUTER_BOUND ( 'NONE', #33902, .T. ) ;
#35141 = CARTESIAN_POINT ( 'NONE',  ( 1.287906020515830141, 3.346456692913386100, -0.9448818897637765168 ) ) ;
#35142 = EDGE_CURVE ( 'NONE', #10888, #11679, #34171, .T. ) ;
#35144 = PLANE ( 'NONE',  #44023 ) ;
#35143 = AXIS2_PLACEMENT_3D ( 'NONE', #46487, #38285, #30528 ) ;
#35145 = PLANE ( 'NONE',  #34605 ) ;
#35146 = VERTEX_POINT ( 'NONE', #10671 ) ;
#35147 = VERTEX_POINT ( 'NONE', #49605 ) ;
#35148 = VECTOR ( 'NONE', #26584, 39.37007874015748143 ) ;
#35149 = VECTOR ( 'NONE', #12866, 39.37007874015748143 ) ;
#35150 = DIRECTION ( 'NONE',  ( 0.9998717552508121775, 0.01601477604151182663, 0.000000000000000000 ) ) ;
#35151 = ORIENTED_EDGE ( 'NONE', *, *, #8597, .T. ) ;
#35152 = DIRECTION ( 'NONE',  ( -1.000000000000000000, -0.000000000000000000, -0.000000000000000000 ) ) ;
#35153 = ADVANCED_FACE ( 'NONE', ( #42153 ), #10413, .F. ) ;
#35154 = DIRECTION ( 'NONE',  ( 0.000000000000000000, 1.000000000000000000, 0.000000000000000000 ) ) ;
#35155 = AXIS2_PLACEMENT_3D ( 'NONE', #17858, #9089, #29479 ) ;
#35156 = AXIS2_PLACEMENT_3D ( 'NONE', #10197, #45038, #13062 ) ;
#35157 = CARTESIAN_POINT ( 'NONE',  ( 0.000000000000000000, 3.267716535433071279, 0.000000000000000000 ) ) ;
#35158 = CARTESIAN_POINT ( 'NONE',  ( 1.243113849864399656, 1.731386041893312022, 2.176571955408725056 ) ) ;
#35159 = CARTESIAN_POINT ( 'NONE',  ( -1.583112249919712999, 0.000000000000000000, -0.7301740747847248469 ) ) ;
#35160 = AXIS2_PLACEMENT_3D ( 'NONE', #27042, #27550, #31694 ) ;
#35161 = EDGE_LOOP ( 'NONE', ( #33280, #17919, #25712, #33510 ) ) ;
#35162 = CARTESIAN_POINT ( 'NONE',  ( 1.636583440222563635, 3.346456692913386100, -0.9448818897637765168 ) ) ;
#35163 = ORIENTED_EDGE ( 'NONE', *, *, #31777, .F. ) ;
#35164 = CARTESIAN_POINT ( 'NONE',  ( 1.909347346926324684, 3.346456692913386100, 0.1574803149606280872 ) ) ;
#35165 = LINE ( 'NONE', #38041, #18717 ) ;
#35166 = CARTESIAN_POINT ( 'NONE',  ( 0.000000000000000000, 3.267716535433071279, 2.204724409448808764 ) ) ;
#35167 = ORIENTED_EDGE ( 'NONE', *, *, #12503, .F. ) ;
#35168 = ORIENTED_EDGE ( 'NONE', *, *, #833, .T. ) ;
#35169 = PLANE ( 'NONE',  #6456 ) ;
#35170 = EDGE_LOOP ( 'NONE', ( #36423, #43032, #23194, #38296 ) ) ;
#35171 = CARTESIAN_POINT ( 'NONE',  ( 1.041132165474419446, 1.728185027159919951, -2.275356686326451161 ) ) ;
#35172 = ORIENTED_EDGE ( 'NONE', *, *, #24402, .T. ) ;
#35173 = ADVANCED_FACE ( 'NONE', ( #38303 ), #7300, .F. ) ;
#35174 = DIRECTION ( 'NONE',  ( -0.000000000000000000, 1.000000000000000000, -0.000000000000000000 ) ) ;
#35175 = CARTESIAN_POINT ( 'NONE',  ( 0.07982360342473591996, 1.709180471932028711, 0.000000000000000000 ) ) ;
#35176 = CARTESIAN_POINT ( 'NONE',  ( 1.091055626815042645, 0.000000000000000000, -0.9448818897637765168 ) ) ;
#35177 = AXIS2_PLACEMENT_3D ( 'NONE', #45867, #13644, #29385 ) ;
#35178 = EDGE_CURVE ( 'NONE', #47345, #903, #7049, .T. ) ;
#35179 = ORIENTED_EDGE ( 'NONE', *, *, #24499, .F. ) ;
#35180 = VERTEX_POINT ( 'NONE', #26406 ) ;
#35181 = EDGE_LOOP ( 'NONE', ( #30255, #28419, #17309, #9621 ) ) ;
#35182 = FACE_OUTER_BOUND ( 'NONE', #29689, .T. ) ;
#35183 = CIRCLE ( 'NONE', #30254, 2.165354330708661568 ) ;
#35184 = DIRECTION ( 'NONE',  ( 0.000000000000000000, 0.000000000000000000, -1.000000000000000000 ) ) ;
#35185 = AXIS2_PLACEMENT_3D ( 'NONE', #18715, #31091, #22334 ) ;
#35186 = ORIENTED_EDGE ( 'NONE', *, *, #18648, .F. ) ;
#35187 = ORIENTED_EDGE ( 'NONE', *, *, #49042, .F. ) ;
#35188 = LINE ( 'NONE', #34436, #21482 ) ;
#35189 = DIRECTION ( 'NONE',  ( 1.000000000000000000, -0.000000000000000000, 0.000000000000000000 ) ) ;
#35190 = DIRECTION ( 'NONE',  ( 1.734723475976806848E-16, -0.000000000000000000, 1.000000000000000000 ) ) ;
#35191 = EDGE_LOOP ( 'NONE', ( #5409, #18565, #31154, #1595 ) ) ;
#35192 = ORIENTED_EDGE ( 'NONE', *, *, #37532, .F. ) ;
#35193 = CARTESIAN_POINT ( 'NONE',  ( 0.8949303405208896001, 1.574803149606302854, -1.971765468592530102 ) ) ;
#35194 = CARTESIAN_POINT ( 'NONE',  ( -0.5756566573089004768, 1.527738838675063882, 2.896516654582634853 ) ) ;
#35195 = VECTOR ( 'NONE', #28974, 39.37007874015748143 ) ;
#35196 = DIRECTION ( 'NONE',  ( -3.986037398843765983E-20, -1.000000000000000000, -1.160734090543304660E-16 ) ) ;
#35197 = ORIENTED_EDGE ( 'NONE', *, *, #44665, .F. ) ;
#35198 = CARTESIAN_POINT ( 'NONE',  ( 1.363819533518803251, 3.346456692913386100, 0.1574803149606283648 ) ) ;
#35200 = VECTOR ( 'NONE', #37301, 39.37007874015748143 ) ;
#35199 = DIRECTION ( 'NONE',  ( -0.000000000000000000, 1.000000000000000000, -0.000000000000000000 ) ) ;
#35201 = ORIENTED_EDGE ( 'NONE', *, *, #44442, .T. ) ;
#35202 = CARTESIAN_POINT ( 'NONE',  ( -0.8942052331142547050, 0.000000000000000000, 0.4330708661417290162 ) ) ;
#35203 = ORIENTED_EDGE ( 'NONE', *, *, #37474, .F. ) ;
#35204 = EDGE_LOOP ( 'NONE', ( #17146, #50871, #11422, #46429 ) ) ;
#35205 = DIRECTION ( 'NONE',  ( 0.000000000000000000, 0.000000000000000000, 1.000000000000000000 ) ) ;
#35206 = CARTESIAN_POINT ( 'NONE',  ( 1.928178237245542492, 0.03859178796661346528, 0.5747578989280442974 ) ) ;
#35207 = CARTESIAN_POINT ( 'NONE',  ( 0.4161812636739331550, 0.000000000000000000, -1.692983086477933830 ) ) ;
#35208 = ADVANCED_FACE ( 'NONE', ( #38791 ), #30288, .T. ) ;
#35209 = DIRECTION ( 'NONE',  ( -3.469446951953613696E-16, 0.000000000000000000, -1.000000000000000000 ) ) ;
#35210 = CARTESIAN_POINT ( 'NONE',  ( -1.166969139818015755, 3.267716535433071279, 1.220472440944875281 ) ) ;
#35211 = EDGE_LOOP ( 'NONE', ( #5792, #7481, #38208, #36852, #12708, #37990 ) ) ;
#35212 = ORIENTED_EDGE ( 'NONE', *, *, #15432, .F. ) ;
#35213 = ORIENTED_EDGE ( 'NONE', *, *, #46050, .F. ) ;
#35214 = CARTESIAN_POINT ( 'NONE',  ( 0.7423782071083087075, 0.000000000000000000, -1.259842519685035134 ) ) ;
#35215 = EDGE_CURVE ( 'NONE', #8198, #47008, #46011, .T. ) ;
#35216 = LINE ( 'NONE', #38592, #39128 ) ;
#35217 = EDGE_CURVE ( 'NONE', #39696, #46790, #50109, .T. ) ;
#35218 = VECTOR ( 'NONE', #41616, 39.37007874015748143 ) ;
#35219 = ADVANCED_FACE ( 'NONE', ( #15044 ), #50900, .F. ) ;
#35220 = AXIS2_PLACEMENT_3D ( 'NONE', #32128, #44489, #27720 ) ;
#35221 = DIRECTION ( 'NONE',  ( -0.01601477604151182663, 0.9998717552508123996, -0.000000000000000000 ) ) ;
#35222 = CARTESIAN_POINT ( 'NONE',  ( 0.8182917201112819283, 3.346456692913386100, -1.102362204724405714 ) ) ;
#35223 = VECTOR ( 'NONE', #13322, 39.37007874015748143 ) ;
#35224 = EDGE_LOOP ( 'NONE', ( #50423, #16196, #9079, #24993 ) ) ;
#35225 = CARTESIAN_POINT ( 'NONE',  ( 1.091055626815042645, 3.346456692913386100, 0.1181102362204704270 ) ) ;
#35226 = EDGE_CURVE ( 'NONE', #34103, #48573, #42738, .T. ) ;
#35227 = LINE ( 'NONE', #39601, #13341 ) ;
#35228 = EDGE_CURVE ( 'NONE', #36716, #50620, #50353, .T. ) ;
#35229 = ORIENTED_EDGE ( 'NONE', *, *, #38504, .F. ) ;
#35230 = LINE ( 'NONE', #31356, #18284 ) ;
#35231 = CARTESIAN_POINT ( 'NONE',  ( 2.088192093915797631, 3.346456692913386100, 0.2755905511810994302 ) ) ;
#35232 = CARTESIAN_POINT ( 'NONE',  ( -1.363819533518803473, 3.346456692913386100, -0.3543307086614174151 ) ) ;
#35233 = ORIENTED_EDGE ( 'NONE', *, *, #41235, .T. ) ;
#35234 = DIRECTION ( 'NONE',  ( -0.01601477604151182663, 0.9998717552508123996, -0.000000000000000000 ) ) ;
#35235 = CARTESIAN_POINT ( 'NONE',  ( 0.07982360342473591996, 1.709180471932028711, 0.000000000000000000 ) ) ;
#35236 = FACE_OUTER_BOUND ( 'NONE', #10233, .T. ) ;
#35237 = ORIENTED_EDGE ( 'NONE', *, *, #36886, .F. ) ;
#35238 = CARTESIAN_POINT ( 'NONE',  ( -1.129409194730853105, 1.697742047597073034, -2.458665826403365173 ) ) ;
#35239 = ORIENTED_EDGE ( 'NONE', *, *, #15134, .T. ) ;
#35240 = AXIS2_PLACEMENT_3D ( 'NONE', #3027, #43006, #46609 ) ;
#35241 = FACE_OUTER_BOUND ( 'NONE', #4276, .T. ) ;
#35242 = EDGE_CURVE ( 'NONE', #30165, #23247, #4793, .T. ) ;
#35243 = DIRECTION ( 'NONE',  ( -1.000000000000000000, -0.000000000000000000, -0.000000000000000000 ) ) ;
#35244 = CARTESIAN_POINT ( 'NONE',  ( -0.2727639067037608278, 3.346456692913386100, 2.165354330708650465 ) ) ;
#35245 = EDGE_CURVE ( 'NONE', #4010, #49945, #26904, .T. ) ;
#35246 = ORIENTED_EDGE ( 'NONE', *, *, #34831, .F. ) ;
#35247 = ORIENTED_EDGE ( 'NONE', *, *, #9043, .T. ) ;
#35248 = CARTESIAN_POINT ( 'NONE',  ( 1.363819533518803029, 3.346456692913386100, -1.417322834645665219 ) ) ;
#35249 = EDGE_CURVE ( 'NONE', #22612, #35273, #11423, .T. ) ;
#35250 = DIRECTION ( 'NONE',  ( -0.9998717552508121775, -0.01601477604151182316, 0.000000000000000000 ) ) ;
#35251 = ORIENTED_EDGE ( 'NONE', *, *, #45368, .F. ) ;
#35252 = DIRECTION ( 'NONE',  ( 0.000000000000000000, 0.000000000000000000, 1.000000000000000000 ) ) ;
#35253 = DIRECTION ( 'NONE',  ( 0.000000000000000000, 1.000000000000000000, 0.000000000000000000 ) ) ;
#35254 = FACE_OUTER_BOUND ( 'NONE', #44464, .T. ) ;
#35255 = LINE ( 'NONE', #50934, #50320 ) ;
#35256 = ORIENTED_EDGE ( 'NONE', *, *, #31508, .F. ) ;
#35257 = ORIENTED_EDGE ( 'NONE', *, *, #12906, .T. ) ;
#35258 = LINE ( 'NONE', #50939, #48818 ) ;
#35259 = AXIS2_PLACEMENT_3D ( 'NONE', #7005, #14756, #22252 ) ;
#35260 = VECTOR ( 'NONE', #7541, 39.37007874015748143 ) ;
#35261 = ADVANCED_FACE ( 'NONE', ( #12431 ), #39292, .F. ) ;
#35262 = CARTESIAN_POINT ( 'NONE',  ( -0.2727639067037607723, 3.346456692913386100, 0.4724409448818869817 ) ) ;
#35263 = ORIENTED_EDGE ( 'NONE', *, *, #46061, .F. ) ;
#35264 = CARTESIAN_POINT ( 'NONE',  ( 1.046684505418381761, 0.4561333243160196060, -1.030376884852512331 ) ) ;
#35265 = ORIENTED_EDGE ( 'NONE', *, *, #12345, .F. ) ;
#35267 = EDGE_LOOP ( 'NONE', ( #27072, #39767, #5063, #36007 ) ) ;
#35266 = VECTOR ( 'NONE', #256, 39.37007874015748143 ) ;
#35268 = FACE_OUTER_BOUND ( 'NONE', #401, .T. ) ;
#35269 = ORIENTED_EDGE ( 'NONE', *, *, #12320, .F. ) ;
#35270 = EDGE_LOOP ( 'NONE', ( #15227, #5364, #40561, #18686 ) ) ;
#35271 = DIRECTION ( 'NONE',  ( 0.9362348706397418674, 1.288287287306305776E-16, -0.3513748240813305279 ) ) ;
#35272 = VECTOR ( 'NONE', #15203, 39.37007874015748143 ) ;
#35273 = VERTEX_POINT ( 'NONE', #8050 ) ;
#35275 = DIRECTION ( 'NONE',  ( 1.000000000000000000, -0.000000000000000000, 0.000000000000000000 ) ) ;
#35274 = AXIS2_PLACEMENT_3D ( 'NONE', #39089, #7099, #38595 ) ;
#35276 = CARTESIAN_POINT ( 'NONE',  ( -0.6214413264104945434, 3.267716535433071279, 2.156057715732901026E-16 ) ) ;
#35277 = CARTESIAN_POINT ( 'NONE',  ( 2.277014451362978420, 1.678755706740915343, -0.4692354975254571237 ) ) ;
#35278 = EDGE_CURVE ( 'NONE', #6017, #8712, #27407, .T. ) ;
#35279 = ADVANCED_FACE ( 'NONE', ( #19661 ), #46992, .F. ) ;
#35280 = LINE ( 'NONE', #43518, #7471 ) ;
#35281 = ADVANCED_FACE ( 'NONE', ( #43 ), #8305, .F. ) ;
#35282 = DIRECTION ( 'NONE',  ( -0.000000000000000000, 1.000000000000000000, -0.000000000000000000 ) ) ;
#35283 = CARTESIAN_POINT ( 'NONE',  ( 2.988781320759228421, 5.118110236220475784, -0.1748580315756567971 ) ) ;
#35284 = ORIENTED_EDGE ( 'NONE', *, *, #20631, .T. ) ;
#35285 = LINE ( 'NONE', #30904, #2739 ) ;
#35286 = CARTESIAN_POINT ( 'NONE',  ( -2.047355983664255863, 1.576684601009278319, 0.7169714724935087879 ) ) ;
#35287 = FACE_OUTER_BOUND ( 'NONE', #37218, .T. ) ;
#35288 = ORIENTED_EDGE ( 'NONE', *, *, #22253, .T. ) ;
#35289 = CARTESIAN_POINT ( 'NONE',  ( 1.015142113812069979, 0.000000000000000000, 1.417322834645662777 ) ) ;
#35290 = DIRECTION ( 'NONE',  ( -1.000000000000000000, 0.000000000000000000, -0.000000000000000000 ) ) ;
#35291 = ORIENTED_EDGE ( 'NONE', *, *, #1243, .T. ) ;
#35292 = CARTESIAN_POINT ( 'NONE',  ( -1.743145509346910149, 0.000000000000000000, 0.03054797143824310862 ) ) ;
#35293 = AXIS2_PLACEMENT_3D ( 'NONE', #13023, #5016, #17151 ) ;
#35294 = VECTOR ( 'NONE', #43983, 39.37007874015748143 ) ;
#35295 = CARTESIAN_POINT ( 'NONE',  ( -1.631260293787041071, 0.0006143858728471982261, -0.6437146846949991508 ) ) ;
#35296 = B_SPLINE_CURVE_WITH_KNOTS ( 'NONE', 3,
 ( #9266, #32520, #1521, #41276 ),
 .UNSPECIFIED., .F., .F.,
 ( 4, 4 ),
 ( 2.051447925150919731E-07, 0.002500220192228647109 ),
 .UNSPECIFIED. ) ;
#35297 = CIRCLE ( 'NONE', #45994, 2.165354330708661568 ) ;
#35298 = DIRECTION ( 'NONE',  ( 1.000000000000000000, -0.000000000000000000, 0.000000000000000000 ) ) ;
#35299 = ADVANCED_FACE ( 'NONE', ( #16052 ), #43917, .F. ) ;
#35300 = VERTEX_POINT ( 'NONE', #35936 ) ;
#35301 = DIRECTION ( 'NONE',  ( -1.000000000000000000, 0.000000000000000000, -1.156482317317869599E-17 ) ) ;
#35302 = FACE_OUTER_BOUND ( 'NONE', #28795, .T. ) ;
#35303 = VECTOR ( 'NONE', #46445, 39.37007874015748143 ) ;
#35304 = EDGE_CURVE ( 'NONE', #44668, #7558, #19908, .T. ) ;
#35305 = PLANE ( 'NONE',  #12752 ) ;
#35306 = FACE_OUTER_BOUND ( 'NONE', #16615, .T. ) ;
#35307 = EDGE_LOOP ( 'NONE', ( #8239, #48682, #28597, #46340 ) ) ;
#35308 = ADVANCED_FACE ( 'NONE', ( #31552 ), #35169, .F. ) ;
#35309 = VECTOR ( 'NONE', #10513, 39.37007874015748143 ) ;
#35310 = ORIENTED_EDGE ( 'NONE', *, *, #19778, .T. ) ;
#35311 = VERTEX_POINT ( 'NONE', #50849 ) ;
#35312 = CARTESIAN_POINT ( 'NONE',  ( 1.287350139463531828, 0.01584012156927684309, 1.548288944013793245 ) ) ;
#35313 = EDGE_CURVE ( 'NONE', #39732, #41937, #16312, .T. ) ;
#35314 = ORIENTED_EDGE ( 'NONE', *, *, #33872, .F. ) ;
#35315 = LINE ( 'NONE', #7935, #20526 ) ;
#35316 = VECTOR ( 'NONE', #27391, 39.37007874015748143 ) ;
#35317 = DIRECTION ( 'NONE',  ( 1.000000000000000000, 0.000000000000000000, 0.000000000000000000 ) ) ;
#35318 = VERTEX_POINT ( 'NONE', #817 ) ;
#35319 = PLANE ( 'NONE',  #47012 ) ;
#35320 = ORIENTED_EDGE ( 'NONE', *, *, #14546, .T. ) ;
#35321 = CARTESIAN_POINT ( 'NONE',  ( -1.091055626815042201, 3.346456692913386100, 1.259842519685033357 ) ) ;
#35322 = FACE_OUTER_BOUND ( 'NONE', #6986, .T. ) ;
#35323 = EDGE_LOOP ( 'NONE', ( #2694, #43083, #13996, #5975 ) ) ;
#35324 = VERTEX_POINT ( 'NONE', #24315 ) ;
#35325 = CARTESIAN_POINT ( 'NONE',  ( -1.779568955232873950, 5.905511811023623991, -1.233650562797313777 ) ) ;
#35326 = ORIENTED_EDGE ( 'NONE', *, *, #2347, .F. ) ;
#35327 = B_SPLINE_CURVE_WITH_KNOTS ( 'NONE', 3,
 ( #42386, #2651, #34157, #34907 ),
 .UNSPECIFIED., .F., .F.,
 ( 4, 4 ),
 ( 2.397468562700561163E-07, 0.01627520709194900037 ),
 .UNSPECIFIED. ) ;
#35328 = LINE ( 'NONE', #11821, #20478 ) ;
#35329 = VECTOR ( 'NONE', #34802, 39.37007874015748143 ) ;
#35330 = VERTEX_POINT ( 'NONE', #23798 ) ;
#35331 = ORIENTED_EDGE ( 'NONE', *, *, #31451, .T. ) ;
#35332 = DIRECTION ( 'NONE',  ( 0.7071067811865486830, 2.775557561562891351E-17, 0.7071067811865462405 ) ) ;
#35333 = FACE_OUTER_BOUND ( 'NONE', #8839, .T. ) ;
#35334 = ORIENTED_EDGE ( 'NONE', *, *, #28681, .T. ) ;
#35335 = AXIS2_PLACEMENT_3D ( 'NONE', #20205, #24347, #48051 ) ;
#35336 = LINE ( 'NONE', #11079, #29525 ) ;
#35337 = EDGE_LOOP ( 'NONE', ( #15339, #28332, #20709, #49553 ) ) ;
#35338 = CARTESIAN_POINT ( 'NONE',  ( 1.699531805983663935, 1.669506266544195761, -1.556832249051517181 ) ) ;
#35339 = CARTESIAN_POINT ( 'NONE',  ( -2.258024766633058622, 0.000000000000000000, -0.1574803149606298636 ) ) ;
#35340 = VECTOR ( 'NONE', #28517, 39.37007874015748143 ) ;
#35341 = VECTOR ( 'NONE', #185, 39.37007874015748143 ) ;
#35342 = CARTESIAN_POINT ( 'NONE',  ( 0.000000000000000000, 3.267716535433071279, -0.9842519685039344823 ) ) ;
#35343 = VECTOR ( 'NONE', #46853, 39.37007874015748143 ) ;
#35344 = EDGE_LOOP ( 'NONE', ( #5879, #12109, #26841, #19636 ) ) ;
#35345 = ORIENTED_EDGE ( 'NONE', *, *, #44190, .F. ) ;
#35346 = EDGE_CURVE ( 'NONE', #24696, #44472, #17314, .T. ) ;
#35347 = CARTESIAN_POINT ( 'NONE',  ( -0.5455278134075214336, 0.000000000000000000, -0.6299212598425175669 ) ) ;
#35348 = LINE ( 'NONE', #46421, #40184 ) ;
#35349 = EDGE_CURVE ( 'NONE', #24866, #47349, #12694, .T. ) ;
#35350 = CARTESIAN_POINT ( 'NONE',  ( -0.8329809839909436686, 1.533199950842965453, -2.833254665166566877 ) ) ;
#35351 = CIRCLE ( 'NONE', #19663, 2.106299212598425008 ) ;
#35352 = CARTESIAN_POINT ( 'NONE',  ( -2.182111253630085734, 0.000000000000000000, -1.141732283464563791 ) ) ;
#35353 = ADVANCED_FACE ( 'NONE', ( #7546 ), #48019, .F. ) ;
#35354 = CARTESIAN_POINT ( 'NONE',  ( -2.867773316779185677, 1.576133919414932638, -0.7050287376752426560 ) ) ;
#35355 = AXIS2_PLACEMENT_3D ( 'NONE', #6397, #2008, #33525 ) ;
#35356 = DIRECTION ( 'NONE',  ( -0.7071067811865466846, -0.000000000000000000, -0.7071067811865483499 ) ) ;
#35357 = ORIENTED_EDGE ( 'NONE', *, *, #20046, .F. ) ;
#35358 = CARTESIAN_POINT ( 'NONE',  ( -1.536664496436148184E-16, 3.267716535433071279, -1.771653543307081025 ) ) ;
#35359 = EDGE_LOOP ( 'NONE', ( #42152, #31269, #49829, #42697 ) ) ;
#35360 = CARTESIAN_POINT ( 'NONE',  ( -1.636583440222564301, 3.267716535433071279, 2.839019714148967077E-16 ) ) ;
#35361 = VERTEX_POINT ( 'NONE', #566 ) ;
#35362 = CARTESIAN_POINT ( 'NONE',  ( 0.6423598643315989731, 1.010863969785771754, -2.512522840280564385 ) ) ;
#35363 = PLANE ( 'NONE',  #41850 ) ;
#35364 = EDGE_CURVE ( 'NONE', #17362, #35848, #15550, .T. ) ;
#35365 = VECTOR ( 'NONE', #45258, 39.37007874015748143 ) ;
#35366 = ORIENTED_EDGE ( 'NONE', *, *, #18152, .F. ) ;
#35367 = CYLINDRICAL_SURFACE ( 'NONE', #39456, 2.165354330708661568 ) ;
#35368 = ADVANCED_FACE ( 'NONE', ( #20435 ), #16572, .F. ) ;
#35369 = ORIENTED_EDGE ( 'NONE', *, *, #35472, .F. ) ;
#35370 = CARTESIAN_POINT ( 'NONE',  ( 2.031248100867566908, 0.5222577735666947829, 1.037175626315068877 ) ) ;
#35371 = ORIENTED_EDGE ( 'NONE', *, *, #40455, .T. ) ;
#35372 = VECTOR ( 'NONE', #32346, 39.37007874015748143 ) ;
#35373 = VECTOR ( 'NONE', #33714, 39.37007874015748143 ) ;
#35374 = CARTESIAN_POINT ( 'NONE',  ( -0.6214413264104945434, 3.346456692913386100, -0.1574803149606301411 ) ) ;
#35375 = CARTESIAN_POINT ( 'NONE',  ( 1.287906020515829919, 3.267716535433071279, -1.666671669919371102 ) ) ;
#35376 = AXIS2_PLACEMENT_3D ( 'NONE', #25057, #36171, #1047 ) ;
#35377 = ORIENTED_EDGE ( 'NONE', *, *, #14474, .F. ) ;
#35378 = CARTESIAN_POINT ( 'NONE',  ( 0.1170985530868079300, 0.02979521312206013725, -1.850078377359382298 ) ) ;
#35379 = ORIENTED_EDGE ( 'NONE', *, *, #25425, .T. ) ;
#35380 = ORIENTED_EDGE ( 'NONE', *, *, #38783, .F. ) ;
#35381 = PLANE ( 'NONE',  #48229 ) ;
#35382 = CARTESIAN_POINT ( 'NONE',  ( 1.930249146414562578, 0.05883613814988478824, 0.3111320644955062886 ) ) ;
#35383 = DIRECTION ( 'NONE',  ( -0.6631698831091616952, 0.000000000000000000, 0.7484689079293679326 ) ) ;
#35384 = VECTOR ( 'NONE', #45745, 39.37007874015748143 ) ;
#35385 = ORIENTED_EDGE ( 'NONE', *, *, #25136, .F. ) ;
#35386 = DIRECTION ( 'NONE',  ( 0.000000000000000000, 0.000000000000000000, -1.000000000000000000 ) ) ;
#35387 = CARTESIAN_POINT ( 'NONE',  ( -1.472219874544909768, 1.696317054561777171, 2.560030851058948898 ) ) ;
#35388 = ORIENTED_EDGE ( 'NONE', *, *, #15489, .T. ) ;
#35389 = LINE ( 'NONE', #27369, #4298 ) ;
#35390 = ORIENTED_EDGE ( 'NONE', *, *, #22379, .F. ) ;
#35391 = VERTEX_POINT ( 'NONE', #3673 ) ;
#35392 = VERTEX_POINT ( 'NONE', #19404 ) ;
#35393 = CARTESIAN_POINT ( 'NONE',  ( -2.437180031585919782, 1.681273446161504426, -1.667735833703134718 ) ) ;
#35394 = CARTESIAN_POINT ( 'NONE',  ( 0.000000000000000000, 3.267716535433071279, -0.1574803149606301411 ) ) ;
#35395 = AXIS2_PLACEMENT_3D ( 'NONE', #1850, #16585, #29209 ) ;
#35396 = FACE_OUTER_BOUND ( 'NONE', #7447, .T. ) ;
#35397 = CARTESIAN_POINT ( 'NONE',  ( -1.166969139818015533, 3.267716535433071279, 4.048737525165544183E-16 ) ) ;
#35398 = ORIENTED_EDGE ( 'NONE', *, *, #33374, .F. ) ;
#35399 = ORIENTED_EDGE ( 'NONE', *, *, #37283, .T. ) ;
#35400 = ADVANCED_FACE ( 'NONE', ( #31300 ), #5200, .F. ) ;
#35401 = CARTESIAN_POINT ( 'NONE',  ( 0.000000000000000000, 3.267716535433071279, -0.8267716535433055070 ) ) ;
#35402 = ADVANCED_FACE ( 'NONE', ( #29199 ), #17845, .F. ) ;
#35403 = FACE_OUTER_BOUND ( 'NONE', #32935, .T. ) ;
#35404 = VERTEX_POINT ( 'NONE', #45183 ) ;
#35405 = CARTESIAN_POINT ( 'NONE',  ( 0.000000000000000000, 3.267716535433071279, -1.141732283464563791 ) ) ;
#35406 = LINE ( 'NONE', #544, #44095 ) ;
#35407 = EDGE_CURVE ( 'NONE', #39871, #2241, #5964, .T. ) ;
#35408 = LINE ( 'NONE', #18460, #24795 ) ;
#35409 = B_SPLINE_CURVE_WITH_KNOTS ( 'NONE', 3,
 ( #25803, #32806, #9808, #40792 ),
 .UNSPECIFIED., .F., .F.,
 ( 4, 4 ),
 ( 2.271749272631870541E-07, 0.002500337609477648517 ),
 .UNSPECIFIED. ) ;
#35410 = VECTOR ( 'NONE', #29071, 39.37007874015748143 ) ;
#35411 = CARTESIAN_POINT ( 'NONE',  ( 2.695799277629595370, 5.905511811023623991, -1.205759334241453429 ) ) ;
#35412 = DIRECTION ( 'NONE',  ( -0.000000000000000000, 0.000000000000000000, 1.000000000000000000 ) ) ;
#35413 = PLANE ( 'NONE',  #27849 ) ;
#35414 = VERTEX_POINT ( 'NONE', #41340 ) ;
#35415 = DIRECTION ( 'NONE',  ( -0.01601477604151182663, 0.9998717552508123996, -0.000000000000000000 ) ) ;
#35416 = CARTESIAN_POINT ( 'NONE',  ( 0.6235241006192031588, 5.905511811023623991, 2.074304693190358595 ) ) ;
#35417 = VECTOR ( 'NONE', #28422, 39.37007874015748143 ) ;
#35418 = ORIENTED_EDGE ( 'NONE', *, *, #3676, .F. ) ;
#35419 = ORIENTED_EDGE ( 'NONE', *, *, #22376, .F. ) ;
#35420 = LINE ( 'NONE', #15543, #1810 ) ;
#35421 = LINE ( 'NONE', #19903, #45111 ) ;
#35422 = EDGE_CURVE ( 'NONE', #15256, #11390, #29462, .T. ) ;
#35423 = CARTESIAN_POINT ( 'NONE',  ( -2.097080421798980687, 3.267716535433071279, -0.1968503937007880511 ) ) ;
#35424 = EDGE_LOOP ( 'NONE', ( #39735, #25432, #105, #27963 ) ) ;
#35425 = EDGE_CURVE ( 'NONE', #4986, #38194, #26535, .T. ) ;
#35426 = ORIENTED_EDGE ( 'NONE', *, *, #231, .T. ) ;
#35427 = DIRECTION ( 'NONE',  ( 1.000000000000000000, -0.000000000000000000, 0.000000000000000000 ) ) ;
#35428 = ORIENTED_EDGE ( 'NONE', *, *, #40176, .T. ) ;
#35429 = CARTESIAN_POINT ( 'NONE',  ( -1.091055626815042201, 3.267716535433071279, 0.1181102362204705658 ) ) ;
#35430 = VERTEX_POINT ( 'NONE', #44434 ) ;
#35431 = LINE ( 'NONE', #3934, #35891 ) ;
#35432 = FACE_OUTER_BOUND ( 'NONE', #34510, .T. ) ;
#35433 = DIRECTION ( 'NONE',  ( -3.469446951953613696E-16, 0.000000000000000000, -1.000000000000000000 ) ) ;
#35434 = CIRCLE ( 'NONE', #2466, 2.246510896728926010 ) ;
#35435 = ORIENTED_EDGE ( 'NONE', *, *, #18749, .F. ) ;
#35436 = ORIENTED_EDGE ( 'NONE', *, *, #14132, .T. ) ;
#35437 = ORIENTED_EDGE ( 'NONE', *, *, #33676, .T. ) ;
#35438 = LINE ( 'NONE', #27673, #8439 ) ;
#35439 = DIRECTION ( 'NONE',  ( 0.000000000000000000, 0.000000000000000000, 1.000000000000000000 ) ) ;
#35440 = ORIENTED_EDGE ( 'NONE', *, *, #735, .F. ) ;
#35441 = VERTEX_POINT ( 'NONE', #36707 ) ;
#35442 = LINE ( 'NONE', #60, #30549 ) ;
#35443 = DIRECTION ( 'NONE',  ( 1.000000000000000000, 0.000000000000000000, -3.469446951953613696E-16 ) ) ;
#35444 = CARTESIAN_POINT ( 'NONE',  ( 0.1067246931122726866, 0.02962905676920215767, 0.000000000000000000 ) ) ;
#35445 = EDGE_CURVE ( 'NONE', #50136, #14952, #37480, .T. ) ;
#35446 = AXIS2_PLACEMENT_3D ( 'NONE', #23712, #7967, #12606 ) ;
#35447 = VERTEX_POINT ( 'NONE', #44679 ) ;
#35448 = VERTEX_POINT ( 'NONE', #1330 ) ;
#35449 = DIRECTION ( 'NONE',  ( 0.000000000000000000, 0.000000000000000000, 1.000000000000000000 ) ) ;
#35450 = DIRECTION ( 'NONE',  ( -1.000000000000000000, 0.000000000000000000, 1.734723475976806848E-16 ) ) ;
#35451 = DIRECTION ( 'NONE',  ( 1.734723475976806848E-16, -0.000000000000000000, 1.000000000000000000 ) ) ;
#35452 = ORIENTED_EDGE ( 'NONE', *, *, #14272, .F. ) ;
#35453 = CARTESIAN_POINT ( 'NONE',  ( -1.439733046521776583, 3.346456692913386100, -0.9448818897637762948 ) ) ;
#35454 = CARTESIAN_POINT ( 'NONE',  ( -1.166969139818016199, 0.000000000000000000, 1.850393700787392293 ) ) ;
#35455 = ORIENTED_EDGE ( 'NONE', *, *, #9729, .T. ) ;
#35456 = CARTESIAN_POINT ( 'NONE',  ( 0.2727639067037604947, 0.000000000000000000, 0.7874015748031454320 ) ) ;
#35457 = EDGE_LOOP ( 'NONE', ( #6643, #45693, #42351, #22154 ) ) ;
#35458 = ORIENTED_EDGE ( 'NONE', *, *, #32880, .F. ) ;
#35459 = VECTOR ( 'NONE', #2101, 39.37007874015748143 ) ;
#35460 = DIRECTION ( 'NONE',  ( -3.469446951953613696E-16, 0.000000000000000000, -1.000000000000000000 ) ) ;
#35461 = DIRECTION ( 'NONE',  ( -0.1785568947986229116, 0.000000000000000000, -0.9839295885986321100 ) ) ;
#35462 = LINE ( 'NONE', #80, #14040 ) ;
#35463 = CARTESIAN_POINT ( 'NONE',  ( 0.1968503937007873017, 3.267716535433071279, -1.574803149606293529 ) ) ;
#35464 = DIRECTION ( 'NONE',  ( -1.000000000000000000, 0.000000000000000000, 1.734723475976806848E-16 ) ) ;
#35465 = VERTEX_POINT ( 'NONE', #25082 ) ;
#35466 = VERTEX_POINT ( 'NONE', #25587 ) ;
#35467 = ORIENTED_EDGE ( 'NONE', *, *, #47894, .F. ) ;
#35468 = CARTESIAN_POINT ( 'NONE',  ( 2.949046705395566459, 1.765204021194747286, -0.1488625692542399903 ) ) ;
#35469 = DIRECTION ( 'NONE',  ( -0.01601477604151182663, 0.9998717552508123996, -0.000000000000000000 ) ) ;
#35470 = ADVANCED_FACE ( 'NONE', ( #44178 ), #16830, .F. ) ;
#35471 = EDGE_CURVE ( 'NONE', #45101, #30940, #1839, .T. ) ;
#35472 = EDGE_CURVE ( 'NONE', #13662, #44152, #32847, .T. ) ;
#35473 = CARTESIAN_POINT ( 'NONE',  ( 1.363819533518803029, 0.000000000000000000, -1.417322834645665219 ) ) ;
#35474 = CARTESIAN_POINT ( 'NONE',  ( -1.709950266952966036, 0.000000000000000000, -0.3398067978735320183 ) ) ;
#35475 = EDGE_LOOP ( 'NONE', ( #1969, #9675, #48027, #7686 ) ) ;
#35476 = DIRECTION ( 'NONE',  ( 0.000000000000000000, 0.000000000000000000, 1.000000000000000000 ) ) ;
#35477 = LINE ( 'NONE', #19716, #14988 ) ;
#35478 = AXIS2_PLACEMENT_3D ( 'NONE', #19889, #35658, #41701 ) ;
#35479 = ORIENTED_EDGE ( 'NONE', *, *, #3239, .T. ) ;
#35480 = DIRECTION ( 'NONE',  ( -0.000000000000000000, -1.000000000000000000, -0.000000000000000000 ) ) ;
#35481 = AXIS2_PLACEMENT_3D ( 'NONE', #22506, #30002, #37761 ) ;
#35482 = CARTESIAN_POINT ( 'NONE',  ( -0.2727639067037608278, 3.346456692913386100, -0.6692913385826758654 ) ) ;
#35483 = EDGE_CURVE ( 'NONE', #1405, #46941, #36965, .T. ) ;
#35484 = CARTESIAN_POINT ( 'NONE',  ( -1.775400203342670347, 1.593155925640307835, -2.359903268218729089 ) ) ;
#35485 = ORIENTED_EDGE ( 'NONE', *, *, #10201, .F. ) ;
#35486 = CARTESIAN_POINT ( 'NONE',  ( -1.087426130748108788, 0.01050254589070086231, -1.412988192946641020 ) ) ;
#35487 = LINE ( 'NONE', #107, #34896 ) ;
#35488 = CARTESIAN_POINT ( 'NONE',  ( -2.362204724409449508, 1.172985819482486924, -0.9842519685039374799 ) ) ;
#35489 = ORIENTED_EDGE ( 'NONE', *, *, #10631, .T. ) ;
#35490 = PLANE ( 'NONE',  #29632 ) ;
#35491 = VECTOR ( 'NONE', #37169, 39.37007874015748143 ) ;
#35492 = ORIENTED_EDGE ( 'NONE', *, *, #15114, .T. ) ;
#35493 = CARTESIAN_POINT ( 'NONE',  ( -2.122484638469143814, 1.673906474958827939, -0.4339650761337435214 ) ) ;
#35494 = CARTESIAN_POINT ( 'NONE',  ( -1.152114531865843006, 1.205361022782829114E-17, 1.393499336327983729 ) ) ;
#35495 = DIRECTION ( 'NONE',  ( -3.986037398843765983E-20, -1.000000000000000000, -1.160734090543304660E-16 ) ) ;
#35496 = LINE ( 'NONE', #7370, #9517 ) ;
#35497 = ADVANCED_FACE ( 'NONE', ( #5461 ), #44937, .F. ) ;
#35498 = EDGE_LOOP ( 'NONE', ( #45806, #42889, #4397, #47507 ) ) ;
#35499 = ORIENTED_EDGE ( 'NONE', *, *, #5250, .T. ) ;
#35500 = DIRECTION ( 'NONE',  ( 0.000000000000000000, 0.000000000000000000, 1.000000000000000000 ) ) ;
#35501 = PLANE ( 'NONE',  #3192 ) ;
#35502 = VERTEX_POINT ( 'NONE', #8820 ) ;
#35503 = PLANE ( 'NONE',  #12673 ) ;
#35504 = LINE ( 'NONE', #44261, #16996 ) ;
#35505 = CARTESIAN_POINT ( 'NONE',  ( -2.808237744966007643, 0.000000000000000000, 0.9124517550441282321 ) ) ;
#35506 = EDGE_CURVE ( 'NONE', #39358, #10544, #13213, .T. ) ;
#35507 = CARTESIAN_POINT ( 'NONE',  ( 1.761347130804464367, 1.743135256392197796, 2.090822154292000690 ) ) ;
#35508 = ORIENTED_EDGE ( 'NONE', *, *, #18903, .T. ) ;
#35509 = VERTEX_POINT ( 'NONE', #9077 ) ;
#35510 = LINE ( 'NONE', #12523, #14257 ) ;
#35511 = FACE_OUTER_BOUND ( 'NONE', #20274, .T. ) ;
#35512 = CARTESIAN_POINT ( 'NONE',  ( 0.7423782071083085965, 3.267716535433071279, 0.7480314960629872445 ) ) ;
#35513 = ORIENTED_EDGE ( 'NONE', *, *, #26380, .F. ) ;
#35514 = EDGE_CURVE ( 'NONE', #33042, #26820, #37219, .T. ) ;
#35515 = LINE ( 'NONE', #20004, #3500 ) ;
#35516 = ORIENTED_EDGE ( 'NONE', *, *, #34231, .F. ) ;
#35517 = EDGE_LOOP ( 'NONE', ( #8734, #17918, #22759, #5085, #4396 ) ) ;
#35518 = CARTESIAN_POINT ( 'NONE',  ( -0.5304089168012655620, 0.01942419597810423823, -1.736909402037482675 ) ) ;
#35519 = B_SPLINE_CURVE_WITH_KNOTS ( 'NONE', 3,
 ( #24342, #21235, #1093, #17110 ),
 .UNSPECIFIED., .F., .F.,
 ( 4, 4 ),
 ( 0.002316997564876225116, 0.004817283094879090156 ),
 .UNSPECIFIED. ) ;
#35520 = ADVANCED_FACE ( 'NONE', ( #40574 ), #12956, .F. ) ;
#35521 = VECTOR ( 'NONE', #21390, 39.37007874015748143 ) ;
#35522 = VECTOR ( 'NONE', #3803, 39.37007874015748143 ) ;
#35523 = EDGE_LOOP ( 'NONE', ( #39557, #46649, #47080, #44563 ) ) ;
#35524 = ORIENTED_EDGE ( 'NONE', *, *, #38497, .F. ) ;
#35525 = LINE ( 'NONE', #15646, #1361 ) ;
#35526 = B_SPLINE_CURVE_WITH_KNOTS ( 'NONE', 3,
 ( #29283, #41921, #1410, #17924 ),
 .UNSPECIFIED., .F., .F.,
 ( 4, 4 ),
 ( 2.136451552133696225E-07, 0.002500479562036453732 ),
 .UNSPECIFIED. ) ;
#35527 = VERTEX_POINT ( 'NONE', #48277 ) ;
#35528 = CIRCLE ( 'NONE', #19844, 2.165354330708661568 ) ;
#35529 = DIRECTION ( 'NONE',  ( -1.000000000000000000, -0.000000000000000000, -0.000000000000000000 ) ) ;
#35530 = DIRECTION ( 'NONE',  ( 1.000000000000000000, 0.000000000000000000, 0.000000000000000000 ) ) ;
#35531 = LINE ( 'NONE', #48382, #38260 ) ;
#35532 = EDGE_CURVE ( 'NONE', #11836, #31518, #28688, .T. ) ;
#35533 = CARTESIAN_POINT ( 'NONE',  ( 1.287906020515830141, 3.267716535433071279, -4.468321617281355077E-16 ) ) ;
#35534 = EDGE_CURVE ( 'NONE', #14773, #26179, #10607, .T. ) ;
#35535 = EDGE_CURVE ( 'NONE', #41248, #40553, #50294, .T. ) ;
#35536 = LINE ( 'NONE', #16686, #4707 ) ;
#35537 = CARTESIAN_POINT ( 'NONE',  ( 2.100227814008711835, 1.653522055412836700, -2.076109931251913565 ) ) ;
#35538 = VERTEX_POINT ( 'NONE', #29972 ) ;
#35539 = DIRECTION ( 'NONE',  ( -0.9998717552508122886, -0.01601477604151182316, 0.000000000000000000 ) ) ;
#35540 = CARTESIAN_POINT ( 'NONE',  ( -2.258024766633058622, 3.346456692913386100, -0.1574803149606298636 ) ) ;
#35541 = LINE ( 'NONE', #20812, #7536 ) ;
#35542 = VERTEX_POINT ( 'NONE', #34612 ) ;
#35543 = CARTESIAN_POINT ( 'NONE',  ( -0.8182917201112819283, 3.346456692913386100, -1.299212598425193210 ) ) ;
#35544 = FACE_OUTER_BOUND ( 'NONE', #13439, .T. ) ;
#35545 = VERTEX_POINT ( 'NONE', #26845 ) ;
#35546 = LINE ( 'NONE', #9458, #14752 ) ;
#35548 = EDGE_CURVE ( 'NONE', #16254, #25553, #14985, .T. ) ;
#35547 = DIRECTION ( 'NONE',  ( 1.000000000000000000, 0.000000000000000000, 0.000000000000000000 ) ) ;
#35549 = DIRECTION ( 'NONE',  ( -0.01601477604151182663, 0.9998717552508123996, -0.000000000000000000 ) ) ;
#35550 = LINE ( 'NONE', #1203, #33196 ) ;
#35551 = VERTEX_POINT ( 'NONE', #30733 ) ;
#35552 = LINE ( 'NONE', #31679, #34678 ) ;
#35553 = PLANE ( 'NONE',  #30846 ) ;
#35554 = VECTOR ( 'NONE', #21735, 39.37007874015748143 ) ;
#35555 = LINE ( 'NONE', #24193, #6157 ) ;
#35556 = CARTESIAN_POINT ( 'NONE',  ( -1.166969139818015533, 0.000000000000000000, 1.417322834645662777 ) ) ;
#35557 = ORIENTED_EDGE ( 'NONE', *, *, #30384, .T. ) ;
#35558 = EDGE_CURVE ( 'NONE', #37873, #48466, #10853, .T. ) ;
#35559 = VERTEX_POINT ( 'NONE', #45434 ) ;
#35560 = ORIENTED_EDGE ( 'NONE', *, *, #31943, .F. ) ;
#35561 = CARTESIAN_POINT ( 'NONE',  ( -1.775400203342670569, 5.905511811023623991, -2.359903268218730421 ) ) ;
#35562 = EDGE_LOOP ( 'NONE', ( #25102, #20475, #28120, #8415 ) ) ;
#35563 = DIRECTION ( 'NONE',  ( 0.000000000000000000, 0.000000000000000000, 1.000000000000000000 ) ) ;
#35564 = B_SPLINE_CURVE_WITH_KNOTS ( 'NONE', 3,
 ( #12199, #43426, #31829, #12710 ),
 .UNSPECIFIED., .F., .F.,
 ( 4, 4 ),
 ( 2.219309651315323410E-07, 0.002500660338287432824 ),
 .UNSPECIFIED. ) ;
#35565 = DIRECTION ( 'NONE',  ( 1.000000000000000000, 0.000000000000000000, 0.000000000000000000 ) ) ;
#35566 = ORIENTED_EDGE ( 'NONE', *, *, #48840, .T. ) ;
#35567 = EDGE_CURVE ( 'NONE', #16203, #19475, #14479, .T. ) ;
#35568 = DIRECTION ( 'NONE',  ( -0.000000000000000000, 1.000000000000000000, -0.000000000000000000 ) ) ;
#35569 = AXIS2_PLACEMENT_3D ( 'NONE', #13136, #9256, #36887 ) ;
#35570 = EDGE_CURVE ( 'NONE', #2996, #3720, #7242, .T. ) ;
#35571 = ORIENTED_EDGE ( 'NONE', *, *, #8635, .F. ) ;
#35572 = PLANE ( 'NONE',  #32322 ) ;
#35573 = EDGE_CURVE ( 'NONE', #10030, #15453, #34109, .T. ) ;
#35574 = LINE ( 'NONE', #10620, #28948 ) ;
#35575 = B_SPLINE_CURVE_WITH_KNOTS ( 'NONE', 3,
 ( #45572, #30367, #49679, #41985 ),
 .UNSPECIFIED., .F., .F.,
 ( 4, 4 ),
 ( 3.456166342725411222E-07, 0.05034329717658189013 ),
 .UNSPECIFIED. ) ;
#35576 = ORIENTED_EDGE ( 'NONE', *, *, #21292, .T. ) ;
#35577 = VERTEX_POINT ( 'NONE', #3108 ) ;
#35578 = CARTESIAN_POINT ( 'NONE',  ( 0.000000000000000000, 3.267716535433071279, 0.7480314960629874665 ) ) ;
#35579 = ORIENTED_EDGE ( 'NONE', *, *, #22227, .T. ) ;
#35580 = LINE ( 'NONE', #8977, #25421 ) ;
#35581 = ORIENTED_EDGE ( 'NONE', *, *, #48394, .T. ) ;
#35582 = VERTEX_POINT ( 'NONE', #38489 ) ;
#35583 = CARTESIAN_POINT ( 'NONE',  ( 2.823445274216730638, 1.450545469922353892, 0.8656477926280681245 ) ) ;
#35584 = LINE ( 'NONE', #37068, #7263 ) ;
#35585 = ORIENTED_EDGE ( 'NONE', *, *, #263, .F. ) ;
#35586 = CARTESIAN_POINT ( 'NONE',  ( -1.901721518280075296, 3.346456692913386100, 0.9055118110236167750 ) ) ;
#35587 = ORIENTED_EDGE ( 'NONE', *, *, #4555, .T. ) ;
#35588 = DIRECTION ( 'NONE',  ( -0.01601477604151182663, 0.9998717552508123996, -0.000000000000000000 ) ) ;
#35589 = VECTOR ( 'NONE', #41898, 39.37007874015748143 ) ;
#35590 = EDGE_CURVE ( 'NONE', #46985, #15789, #6228, .T. ) ;
#35591 = DIRECTION ( 'NONE',  ( -0.9998717552508121775, -0.01601477604151182316, 0.000000000000000000 ) ) ;
#35593 = EDGE_CURVE ( 'NONE', #47342, #6449, #33861, .T. ) ;
#35592 = DIRECTION ( 'NONE',  ( -3.469446951953613696E-16, 0.000000000000000000, -1.000000000000000000 ) ) ;
#35594 = EDGE_CURVE ( 'NONE', #3086, #15117, #14220, .T. ) ;
#35595 = VERTEX_POINT ( 'NONE', #18610 ) ;
#35596 = ORIENTED_EDGE ( 'NONE', *, *, #30505, .F. ) ;
#35597 = AXIS2_PLACEMENT_3D ( 'NONE', #2546, #6166, #26036 ) ;
#35598 = LINE ( 'NONE', #26574, #31057 ) ;
#35599 = DIRECTION ( 'NONE',  ( -0.000000000000000000, 1.000000000000000000, -0.000000000000000000 ) ) ;
#35600 = EDGE_CURVE ( 'NONE', #3078, #25300, #45943, .T. ) ;
#35601 = CARTESIAN_POINT ( 'NONE',  ( 1.244991204790707684, 3.346456692913386100, -1.771653543307081691 ) ) ;
#35602 = CONICAL_SURFACE ( 'NONE', #22412, 1.850107469027523210, 0.6386652850508578450 ) ;
#35603 = CARTESIAN_POINT ( 'NONE',  ( 2.882374435144356095, 1.665690404301812588, -0.6410570582912683557 ) ) ;
#35604 = DIRECTION ( 'NONE',  ( -0.000000000000000000, 1.000000000000000000, -0.000000000000000000 ) ) ;
#35605 = VECTOR ( 'NONE', #25384, 39.37007874015748143 ) ;
#35606 = DIRECTION ( 'NONE',  ( -0.000000000000000000, 1.000000000000000000, -0.000000000000000000 ) ) ;
#35607 = ORIENTED_EDGE ( 'NONE', *, *, #22281, .F. ) ;
#35608 = CARTESIAN_POINT ( 'NONE',  ( 0.4696143004045479352, 0.000000000000000000, -1.102362204724405714 ) ) ;
#35609 = VERTEX_POINT ( 'NONE', #38736 ) ;
#35610 = CARTESIAN_POINT ( 'NONE',  ( 1.909347346926324018, 3.267716535433071279, -0.8893194486674360633 ) ) ;
#35611 = ORIENTED_EDGE ( 'NONE', *, *, #11894, .F. ) ;
#35612 = B_SPLINE_CURVE_WITH_KNOTS ( 'NONE', 3,
 ( #12712, #32604, #44195, #28444 ),
 .UNSPECIFIED., .F., .F.,
 ( 4, 4 ),
 ( 2.019292134928139459E-07, 0.01591357913266653809 ),
 .UNSPECIFIED. ) ;
#35613 = DIRECTION ( 'NONE',  ( -3.469446951953613696E-16, 0.000000000000000000, -1.000000000000000000 ) ) ;
#35614 = PLANE ( 'NONE',  #16269 ) ;
#35615 = CARTESIAN_POINT ( 'NONE',  ( 0.08139965876239094178, 1.610780518492231694, 0.000000000000000000 ) ) ;
#35616 = VERTEX_POINT ( 'NONE', #6732 ) ;
#35617 = DIRECTION ( 'NONE',  ( -0.000000000000000000, 1.000000000000000000, -0.000000000000000000 ) ) ;
#35618 = ORIENTED_EDGE ( 'NONE', *, *, #17627, .F. ) ;
#35619 = DIRECTION ( 'NONE',  ( -3.469446951953613696E-16, 0.000000000000000000, -1.000000000000000000 ) ) ;
#35620 = ORIENTED_EDGE ( 'NONE', *, *, #46976, .T. ) ;
#35621 = DIRECTION ( 'NONE',  ( -0.9465353838348410376, 0.000000000000000000, -0.3226000110797114240 ) ) ;
#35622 = FACE_OUTER_BOUND ( 'NONE', #20981, .T. ) ;
#35623 = EDGE_CURVE ( 'NONE', #22491, #8748, #14735, .T. ) ;
#35624 =( BOUNDED_CURVE ( )  B_SPLINE_CURVE ( 3, ( #18340, #46184, #50285, #42588 ),
 .UNSPECIFIED., .F., .F. ) 
 B_SPLINE_CURVE_WITH_KNOTS ( ( 4, 4 ),
 ( 3.435438260284853662, 3.898473228037360627 ),
 .UNSPECIFIED. ) 
 CURVE ( )  GEOMETRIC_REPRESENTATION_ITEM ( )  RATIONAL_B_SPLINE_CURVE ( ( 1.000000000000000000, 0.9822128812423629451, 0.9822128812423629451, 1.000000000000000000 ) ) 
 REPRESENTATION_ITEM ( '' )  );
#35625 = ORIENTED_EDGE ( 'NONE', *, *, #14707, .T. ) ;
#35626 = EDGE_CURVE ( 'NONE', #12397, #27247, #22234, .T. ) ;
#35627 = VECTOR ( 'NONE', #31311, 39.37007874015748143 ) ;
#35628 = CARTESIAN_POINT ( 'NONE',  ( 0.04921259842519667277, 1.712470432967292622, 2.480735887547718121 ) ) ;
#35629 = VERTEX_POINT ( 'NONE', #42343 ) ;
#35630 = ORIENTED_EDGE ( 'NONE', *, *, #33754, .F. ) ;
#35631 = PLANE ( 'NONE',  #22698 ) ;
#35632 = DIRECTION ( 'NONE',  ( -3.469446951953613696E-16, 0.000000000000000000, -1.000000000000000000 ) ) ;
#35633 = CARTESIAN_POINT ( 'NONE',  ( -2.437180031585919782, 1.582844051365913662, -1.667735833703134718 ) ) ;
#35634 = AXIS2_PLACEMENT_3D ( 'NONE', #47241, #23792, #4172 ) ;
#35635 = EDGE_LOOP ( 'NONE', ( #48410, #26656, #26559, #20610 ) ) ;
#35636 = CARTESIAN_POINT ( 'NONE',  ( -1.377952755905512472, 0.000000000000000000, -2.845674993400276405E-16 ) ) ;
#35637 = CARTESIAN_POINT ( 'NONE',  ( -1.091055626815042645, 3.267716535433071279, 1.870389530743259199 ) ) ;
#35638 = EDGE_LOOP ( 'NONE', ( #46146, #13879, #12130, #40799 ) ) ;
#35639 = DIRECTION ( 'NONE',  ( 0.000000000000000000, -1.000000000000000000, -0.000000000000000000 ) ) ;
#35640 = ORIENTED_EDGE ( 'NONE', *, *, #18005, .T. ) ;
#35641 = EDGE_LOOP ( 'NONE', ( #41119, #29255, #15964, #2858 ) ) ;
#35642 = EDGE_CURVE ( 'NONE', #45218, #25764, #19098, .T. ) ;
#35643 = APPLICATION_PROTOCOL_DEFINITION ( 'draft international standard', 'automotive_design', 1998, #9120 ) ;
#35644 = VERTEX_POINT ( 'NONE', #6987 ) ;
#35645 = CARTESIAN_POINT ( 'NONE',  ( 0.1968503937007873017, 0.000000000000000000, -0.9448818897637765168 ) ) ;
#35646 = LINE ( 'NONE', #22762, #38199 ) ;
#35647 = EDGE_CURVE ( 'NONE', #23969, #34396, #2603, .T. ) ;
#35648 = CARTESIAN_POINT ( 'NONE',  ( 0.5455278134075212115, 0.000000000000000000, 0.9448818897637746295 ) ) ;
#35649 = DIRECTION ( 'NONE',  ( 0.000000000000000000, -1.000000000000000000, 0.000000000000000000 ) ) ;
#35650 = EDGE_CURVE ( 'NONE', #38168, #39348, #29720, .T. ) ;
#35651 = ORIENTED_EDGE ( 'NONE', *, *, #6839, .T. ) ;
#35652 = VERTEX_POINT ( 'NONE', #10098 ) ;
#35653 = CARTESIAN_POINT ( 'NONE',  ( 0.7423782071083084855, 0.000000000000000000, -1.574803149606293529 ) ) ;
#35654 = EDGE_CURVE ( 'NONE', #43157, #30486, #43539, .T. ) ;
#35655 = DIRECTION ( 'NONE',  ( -3.469446951953613696E-16, 0.000000000000000000, -1.000000000000000000 ) ) ;
#35656 = EDGE_LOOP ( 'NONE', ( #15442, #16973, #42425, #43359 ) ) ;
#35657 = DIRECTION ( 'NONE',  ( 0.9998717552508121775, 0.01601477604151182663, 0.000000000000000000 ) ) ;
#35658 = DIRECTION ( 'NONE',  ( 0.000000000000000000, 0.000000000000000000, -1.000000000000000000 ) ) ;
#35659 = VECTOR ( 'NONE', #48744, 39.37007874015748143 ) ;
#35660 = CARTESIAN_POINT ( 'NONE',  ( -1.198202975868768005, 3.346456692913386100, 1.732283464566920950 ) ) ;
#35661 = CARTESIAN_POINT ( 'NONE',  ( 2.158170387640339527, 6.692913385826772199, 0.2426819907294805456 ) ) ;
#35663 = LINE ( 'NONE', #23521, #16331 ) ;
#35662 = VECTOR ( 'NONE', #5859, 39.37007874015748143 ) ;
#35664 = ORIENTED_EDGE ( 'NONE', *, *, #37179, .F. ) ;
#35665 = CARTESIAN_POINT ( 'NONE',  ( 0.08119777152254364916, 1.623385212329073957, 0.000000000000000000 ) ) ;
#35666 = CARTESIAN_POINT ( 'NONE',  ( 1.091055626815042645, 3.346456692913386100, 0.9448818897637746295 ) ) ;
#35667 = AXIS2_PLACEMENT_3D ( 'NONE', #26938, #15580, #10947 ) ;
#35668 = VERTEX_POINT ( 'NONE', #47189 ) ;
#35669 = VECTOR ( 'NONE', #47938, 39.37007874015748143 ) ;
#35670 = ORIENTED_EDGE ( 'NONE', *, *, #19626, .T. ) ;
#35671 = CIRCLE ( 'NONE', #13422, 1.743387098533651480 ) ;
#35672 = DIRECTION ( 'NONE',  ( -3.469446951953613696E-16, 0.000000000000000000, -1.000000000000000000 ) ) ;
#35673 = CARTESIAN_POINT ( 'NONE',  ( -1.195183497228115035E-16, 3.346456692913386100, 0.6299212598425161236 ) ) ;
#35674 = LINE ( 'NONE', #23794, #49389 ) ;
#35675 = ORIENTED_EDGE ( 'NONE', *, *, #48117, .F. ) ;
#35676 = ORIENTED_EDGE ( 'NONE', *, *, #3130, .F. ) ;
#35677 = CARTESIAN_POINT ( 'NONE',  ( -2.576863348864732117, 1.205361022782829114E-17, 1.442554885838412071 ) ) ;
#35678 = ORIENTED_EDGE ( 'NONE', *, *, #36140, .T. ) ;
#35679 = DIRECTION ( 'NONE',  ( 0.9998717552508121775, 0.01601477604151182663, 0.000000000000000000 ) ) ;
#35680 = VERTEX_POINT ( 'NONE', #24260 ) ;
#35681 = CARTESIAN_POINT ( 'NONE',  ( 0.4696143004045479352, 0.000000000000000000, -0.4724409448818886470 ) ) ;
#35682 = DIRECTION ( 'NONE',  ( 0.5773502691896252870, 0.5773502691896266192, 0.5773502691896251759 ) ) ;
#35683 = DIRECTION ( 'NONE',  ( 0.000000000000000000, 0.000000000000000000, -1.000000000000000000 ) ) ;
#35684 = VERTEX_POINT ( 'NONE', #7489 ) ;
#35685 = EDGE_CURVE ( 'NONE', #15117, #35815, #8508, .T. ) ;
#35686 = ORIENTED_EDGE ( 'NONE', *, *, #37283, .F. ) ;
#35687 = ORIENTED_EDGE ( 'NONE', *, *, #27422, .T. ) ;
#35688 = PLANE ( 'NONE',  #44677 ) ;
#35689 = FACE_OUTER_BOUND ( 'NONE', #14929, .T. ) ;
#35690 = EDGE_CURVE ( 'NONE', #11338, #681, #27858, .T. ) ;
#35691 = ORIENTED_EDGE ( 'NONE', *, *, #6101, .F. ) ;
#35692 = VERTEX_POINT ( 'NONE', #38977 ) ;
#35693 = LINE ( 'NONE', #40591, #10788 ) ;
#35694 = CARTESIAN_POINT ( 'NONE',  ( 0.000000000000000000, 1.574803149606302854, 0.000000000000000000 ) ) ;
#35695 = CARTESIAN_POINT ( 'NONE',  ( -1.091055626815042645, 3.346456692913386100, -0.5118110236220467790 ) ) ;
#35696 = EDGE_CURVE ( 'NONE', #28109, #18363, #8252, .T. ) ;
#35697 = EDGE_LOOP ( 'NONE', ( #27857, #4585, #37670, #23997 ) ) ;
#35698 = CARTESIAN_POINT ( 'NONE',  ( 1.930898218216747120, 1.205361022782829114E-17, -0.8788249315385436855 ) ) ;
#35699 = CARTESIAN_POINT ( 'NONE',  ( -0.8067290215918264673, 1.574803149606302854, 2.009464521518170343 ) ) ;
#35700 = CARTESIAN_POINT ( 'NONE',  ( 0.002207914879453961969, 5.905511811023623991, 0.04916304461325442243 ) ) ;
#35701 = ORIENTED_EDGE ( 'NONE', *, *, #4316, .F. ) ;
#35702 = CARTESIAN_POINT ( 'NONE',  ( 0.2727639067037604947, 0.000000000000000000, 0.4724409448818868706 ) ) ;
#35703 = VECTOR ( 'NONE', #33440, 39.37007874015748143 ) ;
#35704 = DIRECTION ( 'NONE',  ( -0.000000000000000000, 0.000000000000000000, 1.000000000000000000 ) ) ;
#35705 = ORIENTED_EDGE ( 'NONE', *, *, #16294, .F. ) ;
#35706 = LINE ( 'NONE', #22825, #38156 ) ;
#35707 = EDGE_LOOP ( 'NONE', ( #22864, #15035, #7993, #33013, #12121, #2051, #8434, #41639, #45782, #15387, #46246, #22753, #28449 ) ) ;
#35708 = EDGE_LOOP ( 'NONE', ( #9690, #831, #40342, #10429 ) ) ;
#35709 = CARTESIAN_POINT ( 'NONE',  ( 1.560669927219590303, 3.346456692913386100, -1.102362204724405714 ) ) ;
#35710 = VECTOR ( 'NONE', #46964, 39.37007874015748143 ) ;
#35711 = VECTOR ( 'NONE', #22964, 39.37007874015748143 ) ;
#35712 = CARTESIAN_POINT ( 'NONE',  ( 4.268512490100411402E-16, 3.267716535433071279, 1.889763779527550369 ) ) ;
#35713 = EDGE_CURVE ( 'NONE', #12116, #12736, #4315, .T. ) ;
#35714 = FACE_OUTER_BOUND ( 'NONE', #25782, .T. ) ;
#35715 = CARTESIAN_POINT ( 'NONE',  ( 0.2727639067037604947, 3.267716535433071279, 0.1574803149606283648 ) ) ;
#35716 = VERTEX_POINT ( 'NONE', #3616 ) ;
#35717 = VERTEX_POINT ( 'NONE', #11611 ) ;
#35718 = CONICAL_SURFACE ( 'NONE', #10143, 2.165354330708661568, 0.2617993877991570129 ) ;
#35719 = EDGE_CURVE ( 'NONE', #30154, #216, #15733, .T. ) ;
#35720 = ORIENTED_EDGE ( 'NONE', *, *, #18396, .F. ) ;
#35721 = CARTESIAN_POINT ( 'NONE',  ( -1.091055626815042645, 3.267716535433071279, 1.892679809432644389E-16 ) ) ;
#35722 = FACE_OUTER_BOUND ( 'NONE', #34478, .T. ) ;
#35723 = DIRECTION ( 'NONE',  ( -3.469446951953613696E-16, 0.000000000000000000, -1.000000000000000000 ) ) ;
#35724 = LINE ( 'NONE', #36499, #43472 ) ;
#35725 = EDGE_LOOP ( 'NONE', ( #44580, #34559, #9862, #47920 ) ) ;
#35726 = CARTESIAN_POINT ( 'NONE',  ( 1.287906020515830141, 0.000000000000000000, -8.878505979408855953E-16 ) ) ;
#35727 = ADVANCED_FACE ( 'NONE', ( #19347 ), #506, .F. ) ;
#35728 = CARTESIAN_POINT ( 'NONE',  ( 2.164658444855302122, 5.905511811023623991, -0.04795272066889885720 ) ) ;
#35729 = ORIENTED_EDGE ( 'NONE', *, *, #15757, .T. ) ;
#35730 = CARTESIAN_POINT ( 'NONE',  ( -2.100227814008681637, 1.686526752338742385, -2.076109931251943763 ) ) ;
#35731 = CARTESIAN_POINT ( 'NONE',  ( 0.1067246931122726866, 0.02962905676920215767, 0.000000000000000000 ) ) ;
#35732 = CARTESIAN_POINT ( 'NONE',  ( -0.5455270741695672498, 1.205361022782829114E-17, -1.791688814994948808 ) ) ;
#35733 = ORIENTED_EDGE ( 'NONE', *, *, #30172, .F. ) ;
#35734 = DIRECTION ( 'NONE',  ( -1.000000000000000000, 0.000000000000000000, 0.000000000000000000 ) ) ;
#35735 = DIRECTION ( 'NONE',  ( 1.734723475976806848E-16, -0.000000000000000000, 1.000000000000000000 ) ) ;
#35736 = CARTESIAN_POINT ( 'NONE',  ( 1.015142113812069313, 0.000000000000000000, -0.03937007874015881204 ) ) ;
#35737 = VECTOR ( 'NONE', #49255, 39.37007874015748143 ) ;
#35738 = ORIENTED_EDGE ( 'NONE', *, *, #17875, .T. ) ;
#35739 = VECTOR ( 'NONE', #42466, 39.37007874015748143 ) ;
#35740 = DIRECTION ( 'NONE',  ( -0.000000000000000000, 1.000000000000000000, -0.000000000000000000 ) ) ;
#35741 = CARTESIAN_POINT ( 'NONE',  ( 0.000000000000000000, 1.574803149606302854, 0.000000000000000000 ) ) ;
#35742 = EDGE_LOOP ( 'NONE', ( #36760, #49135, #4076, #38486 ) ) ;
#35743 = CARTESIAN_POINT ( 'NONE',  ( -2.889674983507169337, 1.674218314264582785, -0.6090712660038034576 ) ) ;
#35744 = CIRCLE ( 'NONE', #280, 2.165354330708661568 ) ;
#35745 = PLANE ( 'NONE',  #39167 ) ;
#35746 = FACE_OUTER_BOUND ( 'NONE', #31314, .T. ) ;
#35747 = DIRECTION ( 'NONE',  ( 1.000000000000000000, 0.000000000000000000, 0.000000000000000000 ) ) ;
#35748 = VERTEX_POINT ( 'NONE', #4128 ) ;
#35749 = ORIENTED_EDGE ( 'NONE', *, *, #46965, .T. ) ;
#35750 = CARTESIAN_POINT ( 'NONE',  ( -2.803169890850663037, 1.572684734721109923, 0.9280490062237302107 ) ) ;
#35751 = AXIS2_PLACEMENT_3D ( 'NONE', #35726, #8363, #4488 ) ;
#35752 = LINE ( 'NONE', #15866, #28761 ) ;
#35753 = ADVANCED_FACE ( 'NONE', ( #43089 ), #7738, .F. ) ;
#35754 = EDGE_LOOP ( 'NONE', ( #27121, #3810, #37544, #12727 ) ) ;
#35755 = CARTESIAN_POINT ( 'NONE',  ( -2.254603722160883006, 1.577541803200882553, -0.9101444522137277504 ) ) ;
#35756 = CARTESIAN_POINT ( 'NONE',  ( -1.166969139818015977, 3.346456692913386100, -0.1574803149606300023 ) ) ;
#35757 = CARTESIAN_POINT ( 'NONE',  ( 2.378961647330872786, 0.000000000000000000, 0.4330708661417287386 ) ) ;
#35758 = EDGE_CURVE ( 'NONE', #51008, #17239, #19851, .T. ) ;
#35759 = CARTESIAN_POINT ( 'NONE',  ( -1.712529581123628741, 0.0001683915352326838515, -0.3403955095013877497 ) ) ;
#35760 = ORIENTED_EDGE ( 'NONE', *, *, #31290, .T. ) ;
#35761 = ORIENTED_EDGE ( 'NONE', *, *, #1120, .T. ) ;
#35762 = EDGE_CURVE ( 'NONE', #35318, #33053, #40280, .T. ) ;
#35763 = DIRECTION ( 'NONE',  ( -0.000000000000000000, 1.000000000000000000, -0.000000000000000000 ) ) ;
#35764 = DIRECTION ( 'NONE',  ( -0.000000000000000000, 1.000000000000000000, -0.000000000000000000 ) ) ;
#35765 = LINE ( 'NONE', #47851, #46098 ) ;
#35766 = ADVANCED_FACE ( 'NONE', ( #28113 ), #39231, .F. ) ;
#35767 = DIRECTION ( 'NONE',  ( 1.000000000000000000, 0.000000000000000000, 0.000000000000000000 ) ) ;
#35768 = FACE_BOUND ( 'NONE', #45229, .T. ) ;
#35769 = ORIENTED_EDGE ( 'NONE', *, *, #20569, .F. ) ;
#35770 = DIRECTION ( 'NONE',  ( -1.000000000000000000, 0.000000000000000000, -0.000000000000000000 ) ) ;
#35771 = ORIENTED_EDGE ( 'NONE', *, *, #21433, .F. ) ;
#35772 = EDGE_LOOP ( 'NONE', ( #43423, #39506, #39862, #31482, #21424 ) ) ;
#35773 = DIRECTION ( 'NONE',  ( -0.8345732537213079727, 0.000000000000000000, 0.5508969814520945363 ) ) ;
#35774 = EDGE_CURVE ( 'NONE', #14656, #7588, #17221, .T. ) ;
#35775 = ORIENTED_EDGE ( 'NONE', *, *, #3418, .F. ) ;
#35776 = VERTEX_POINT ( 'NONE', #36135 ) ;
#35777 = DIRECTION ( 'NONE',  ( 0.000000000000000000, 0.000000000000000000, 1.000000000000000000 ) ) ;
#35778 = ORIENTED_EDGE ( 'NONE', *, *, #766, .F. ) ;
#35779 = AXIS2_PLACEMENT_3D ( 'NONE', #47861, #28021, #12533 ) ;
#35780 = AXIS2_PLACEMENT_3D ( 'NONE', #45289, #6070, #45796 ) ;
#35781 = ADVANCED_FACE ( 'NONE', ( #51047 ), #47448, .F. ) ;
#35782 = AXIS2_PLACEMENT_3D ( 'NONE', #13395, #25011, #16506 ) ;
#35783 = CARTESIAN_POINT ( 'NONE',  ( 2.134236802639954522, 0.000000000000000000, -2.040539317874581204 ) ) ;
#35784 = LINE ( 'NONE', #16425, #50746 ) ;
#35785 = LINE ( 'NONE', #36047, #11052 ) ;
#35786 = VECTOR ( 'NONE', #2416, 39.37007874015748143 ) ;
#35787 = VECTOR ( 'NONE', #6720, 39.37007874015748143 ) ;
#35788 = EDGE_CURVE ( 'NONE', #30730, #14887, #23736, .T. ) ;
#35789 = DIRECTION ( 'NONE',  ( -1.000000000000000000, 0.000000000000000000, 1.734723475976806848E-16 ) ) ;
#35790 = LINE ( 'NONE', #16166, #14631 ) ;
#35791 = CARTESIAN_POINT ( 'NONE',  ( 1.287906020515830141, 3.267716535433071279, -0.6299212598425181220 ) ) ;
#35792 = VECTOR ( 'NONE', #45171, 39.37007874015748143 ) ;
#35793 = ORIENTED_EDGE ( 'NONE', *, *, #26415, .T. ) ;
#35794 = DIRECTION ( 'NONE',  ( 0.000000000000000000, 0.000000000000000000, 1.000000000000000000 ) ) ;
#35795 = FACE_OUTER_BOUND ( 'NONE', #3802, .T. ) ;
#35796 = ADVANCED_FACE ( 'NONE', ( #12125 ), #30985, .F. ) ;
#35797 = CARTESIAN_POINT ( 'NONE',  ( 0.04921259842519689481, 1.205361022782829114E-17, 1.934165248549660987 ) ) ;
#35798 = ORIENTED_EDGE ( 'NONE', *, *, #30590, .T. ) ;
#35799 = PLANE ( 'NONE',  #19880 ) ;
#35800 = CARTESIAN_POINT ( 'NONE',  ( -1.734268221780295827, 0.000000000000000000, 0.1852605408175444779 ) ) ;
#35801 = ORIENTED_EDGE ( 'NONE', *, *, #30368, .T. ) ;
#35802 = LINE ( 'NONE', #38909, #13100 ) ;
#35803 = CARTESIAN_POINT ( 'NONE',  ( 1.214996082262586485, 1.694553939843470358, 1.937611079607071130 ) ) ;
#35804 = PLANE ( 'NONE',  #23488 ) ;
#35805 = ADVANCED_FACE ( 'NONE', ( #1781 ), #32062, .F. ) ;
#35806 = CARTESIAN_POINT ( 'NONE',  ( -0.01649396867657461699, 0.000000000000000000, 1.928239385118262650 ) ) ;
#35807 = ORIENTED_EDGE ( 'NONE', *, *, #39377, .F. ) ;
#35808 = CARTESIAN_POINT ( 'NONE',  ( -2.182111253630085290, 3.346456692913386100, 0.7480314960629874665 ) ) ;
#35809 = EDGE_CURVE ( 'NONE', #26431, #36543, #17532, .T. ) ;
#35810 = DIRECTION ( 'NONE',  ( 1.000000000000000000, 0.000000000000000000, -3.469446951953613696E-16 ) ) ;
#35811 = FACE_OUTER_BOUND ( 'NONE', #23811, .T. ) ;
#35812 = CARTESIAN_POINT ( 'NONE',  ( 1.636583440222563857, 3.267716535433071279, -2.839019714148966584E-16 ) ) ;
#35813 = ORIENTED_EDGE ( 'NONE', *, *, #26829, .F. ) ;
#35814 = PRODUCT_DEFINITION_FORMATION_WITH_SPECIFIED_SOURCE ( 'ANY', '', #28122, .NOT_KNOWN. ) ;
#35815 = VERTEX_POINT ( 'NONE', #33294 ) ;
#35816 = ORIENTED_EDGE ( 'NONE', *, *, #9955, .F. ) ;
#35817 = AXIS2_PLACEMENT_3D ( 'NONE', #10204, #41200, #37071 ) ;
#35818 = LINE ( 'NONE', #705, #45179 ) ;
#35819 = EDGE_LOOP ( 'NONE', ( #19601, #31642, #27118, #32675 ) ) ;
#35820 = DIRECTION ( 'NONE',  ( 1.734723475976806848E-16, 0.000000000000000000, 1.000000000000000000 ) ) ;
#35821 = ORIENTED_EDGE ( 'NONE', *, *, #48945, .T. ) ;
#35822 = AXIS2_PLACEMENT_3D ( 'NONE', #44615, #16765, #40769 ) ;
#35823 = EDGE_CURVE ( 'NONE', #49048, #19022, #36651, .T. ) ;
#35824 = CIRCLE ( 'NONE', #23426, 1.743387098533651480 ) ;
#35825 = CARTESIAN_POINT ( 'NONE',  ( -2.122091976112999490, 1.205361022782829114E-17, 0.4338754535132819390 ) ) ;
#35826 = ORIENTED_EDGE ( 'NONE', *, *, #17426, .F. ) ;
#35827 = FACE_OUTER_BOUND ( 'NONE', #49723, .T. ) ;
#35828 = ADVANCED_FACE ( 'NONE', ( #5910 ), #25462, .T. ) ;
#35829 = CARTESIAN_POINT ( 'NONE',  ( -0.3857230305054721864, 0.000000000000000000, 1.849896105471422025 ) ) ;
#35830 = AXIS2_PLACEMENT_3D ( 'NONE', #625, #36258, #879 ) ;
#35831 = B_SPLINE_CURVE_WITH_KNOTS ( 'NONE', 3,
 ( #28244, #8892, #40404, #16389 ),
 .UNSPECIFIED., .F., .F.,
 ( 4, 4 ),
 ( 0.001738546130514813902, 0.004792765071277856927 ),
 .UNSPECIFIED. ) ;
#35832 = ORIENTED_EDGE ( 'NONE', *, *, #33582, .F. ) ;
#35833 = DIRECTION ( 'NONE',  ( -0.01601477604151182663, 0.9998717552508123996, -0.000000000000000000 ) ) ;
#35834 = ORIENTED_EDGE ( 'NONE', *, *, #4316, .T. ) ;
#35835 = LINE ( 'NONE', #28075, #9764 ) ;
#35836 = VERTEX_POINT ( 'NONE', #40522 ) ;
#35837 = ORIENTED_EDGE ( 'NONE', *, *, #28530, .T. ) ;
#35838 = CARTESIAN_POINT ( 'NONE',  ( -1.171400696859933532, 1.590714628027123823, 1.864644694871980590 ) ) ;
#35839 = CARTESIAN_POINT ( 'NONE',  ( 2.126910391174609671, 1.205361022782829114E-17, 0.2384475364948296372 ) ) ;
#35840 = ORIENTED_EDGE ( 'NONE', *, *, #6894, .F. ) ;
#35841 = CARTESIAN_POINT ( 'NONE',  ( 1.636583440222563857, 3.346456692913386100, -0.6299212598425181220 ) ) ;
#35842 = ORIENTED_EDGE ( 'NONE', *, *, #28751, .T. ) ;
#35843 = DIRECTION ( 'NONE',  ( -3.469446951953613696E-16, 0.000000000000000000, -1.000000000000000000 ) ) ;
#35844 = DIRECTION ( 'NONE',  ( -0.000000000000000000, 1.000000000000000000, -0.000000000000000000 ) ) ;
#35845 = EDGE_CURVE ( 'NONE', #34706, #13220, #9793, .T. ) ;
#35846 = DIRECTION ( 'NONE',  ( -0.01601477604151182663, 0.9998717552508123996, -0.000000000000000000 ) ) ;
#35847 = ORIENTED_EDGE ( 'NONE', *, *, #12508, .F. ) ;
#35848 = VERTEX_POINT ( 'NONE', #36909 ) ;
#35849 = DIRECTION ( 'NONE',  ( 0.000000000000000000, 0.000000000000000000, 1.000000000000000000 ) ) ;
#35850 = CARTESIAN_POINT ( 'NONE',  ( -1.205050450470247725, 0.008618577144216254052, 1.304493073717302165 ) ) ;
#35851 = AXIS2_PLACEMENT_3D ( 'NONE', #22965, #38717, #41573 ) ;
#35852 = LINE ( 'NONE', #743, #4379 ) ;
#35853 = AXIS2_PLACEMENT_3D ( 'NONE', #11398, #7279, #26878 ) ;
#35854 = PLANE ( 'NONE',  #25206 ) ;
#35855 = EDGE_CURVE ( 'NONE', #27411, #46657, #20892, .T. ) ;
#35856 = VECTOR ( 'NONE', #19480, 39.37007874015748143 ) ;
#35857 = CARTESIAN_POINT ( 'NONE',  ( 0.000000000000000000, 3.267716535433071279, -0.6299212598425177889 ) ) ;
#35858 = EDGE_CURVE ( 'NONE', #16446, #42094, #9806, .T. ) ;
#35859 = LINE ( 'NONE', #27588, #11968 ) ;
#35860 = VERTEX_POINT ( 'NONE', #28633 ) ;
#35861 = ADVANCED_FACE ( 'NONE', ( #24515 ), #48221, .F. ) ;
#35862 = CARTESIAN_POINT ( 'NONE',  ( 0.1968503937007873017, 3.267716535433071279, -6.829619984160653116E-17 ) ) ;
#35863 = AXIS2_PLACEMENT_3D ( 'NONE', #47728, #5169, #40031 ) ;
#35864 = VERTEX_POINT ( 'NONE', #41287 ) ;
#35865 = DIRECTION ( 'NONE',  ( -3.469446951953613696E-16, 0.000000000000000000, -1.000000000000000000 ) ) ;
#35866 = EDGE_CURVE ( 'NONE', #39604, #12011, #36330, .T. ) ;
#35867 = ORIENTED_EDGE ( 'NONE', *, *, #45329, .T. ) ;
#35868 = DIRECTION ( 'NONE',  ( 0.2660368455666826115, 0.000000000000000000, -0.9639628606958511314 ) ) ;
#35869 = LINE ( 'NONE', #43849, #15463 ) ;
#35870 = DIRECTION ( 'NONE',  ( 1.734723475976806848E-16, -0.000000000000000000, 1.000000000000000000 ) ) ;
#35871 = ORIENTED_EDGE ( 'NONE', *, *, #30071, .T. ) ;
#35872 = CARTESIAN_POINT ( 'NONE',  ( 0.000000000000000000, 3.267716535433071279, 0.6299212598425164567 ) ) ;
#35873 = VERTEX_POINT ( 'NONE', #17033 ) ;
#35874 = CARTESIAN_POINT ( 'NONE',  ( -2.165460538733998241, 5.905511811023623991, 0.04798874274652838168 ) ) ;
#35875 = EDGE_LOOP ( 'NONE', ( #12132, #38215, #8877, #20361 ) ) ;
#35876 = ADVANCED_FACE ( 'NONE', ( #40267 ), #44622, .F. ) ;
#35877 = CARTESIAN_POINT ( 'NONE',  ( 1.091055626815043311, 3.267716535433071279, 1.574803149606291974 ) ) ;
#35878 = FACE_OUTER_BOUND ( 'NONE', #28344, .T. ) ;
#35879 = EDGE_CURVE ( 'NONE', #36555, #3078, #18497, .T. ) ;
#35880 = CARTESIAN_POINT ( 'NONE',  ( -1.062992125984250968, 0.5905511811023621549, 1.181102362204724088 ) ) ;
#35881 = VECTOR ( 'NONE', #47627, 39.37007874015748143 ) ;
#35882 = EDGE_CURVE ( 'NONE', #21553, #11117, #3667, .T. ) ;
#35883 = ORIENTED_EDGE ( 'NONE', *, *, #40550, .T. ) ;
#35884 = ORIENTED_EDGE ( 'NONE', *, *, #14312, .F. ) ;
#35885 = VECTOR ( 'NONE', #5671, 39.37007874015748143 ) ;
#35886 = VECTOR ( 'NONE', #4617, 39.37007874015748143 ) ;
#35887 = DIRECTION ( 'NONE',  ( 0.000000000000000000, 0.000000000000000000, -1.000000000000000000 ) ) ;
#35888 = PLANE ( 'NONE',  #2585 ) ;
#35889 = FACE_BOUND ( 'NONE', #18389, .T. ) ;
#35890 = B_SPLINE_CURVE_WITH_KNOTS ( 'NONE', 3,
 ( #11827, #43053, #31457, #12344 ),
 .UNSPECIFIED., .F., .F.,
 ( 4, 4 ),
 ( 0.0001309346361729752512, 0.002631017890005541739 ),
 .UNSPECIFIED. ) ;
#35891 = VECTOR ( 'NONE', #15555, 39.37007874015748143 ) ;
#35892 = ORIENTED_EDGE ( 'NONE', *, *, #14847, .F. ) ;
#35893 = CARTESIAN_POINT ( 'NONE',  ( -1.536664496436148184E-16, 0.000000000000000000, 0.1181102362204701633 ) ) ;
#35894 = LINE ( 'NONE', #520, #1092 ) ;
#35895 = EDGE_LOOP ( 'NONE', ( #33534, #33908, #24699, #5482 ) ) ;
#35896 = DIRECTION ( 'NONE',  ( -0.000000000000000000, 1.000000000000000000, -0.000000000000000000 ) ) ;
#35897 = CIRCLE ( 'NONE', #15293, 2.106299212598425008 ) ;
#35898 = ORIENTED_EDGE ( 'NONE', *, *, #27335, .F. ) ;
#35899 = VERTEX_POINT ( 'NONE', #32268 ) ;
#35900 = APPLICATION_PROTOCOL_DEFINITION ( 'draft international standard', 'automotive_design', 1998, #20352 ) ;
#35901 = ORIENTED_EDGE ( 'NONE', *, *, #3873, .T. ) ;
#35902 = CARTESIAN_POINT ( 'NONE',  ( 2.203200495056982788, 1.648162179384485837, 1.241478329866867458 ) ) ;
#35903 = LINE ( 'NONE', #28913, #31587 ) ;
#35904 = DIRECTION ( 'NONE',  ( 0.000000000000000000, 0.000000000000000000, -1.000000000000000000 ) ) ;
#35905 = LINE ( 'NONE', #8535, #22229 ) ;
#35906 = ORIENTED_EDGE ( 'NONE', *, *, #18833, .T. ) ;
#35907 = VERTEX_POINT ( 'NONE', #765 ) ;
#35908 = LINE ( 'NONE', #796, #29895 ) ;
#35909 = CARTESIAN_POINT ( 'NONE',  ( -0.2483447016818748909, 1.616937350427616327, -2.942339451681899032 ) ) ;
#35910 = B_SPLINE_CURVE_WITH_KNOTS ( 'NONE', 3,
 ( #48057, #8345, #27959, #39840 ),
 .UNSPECIFIED., .F., .F.,
 ( 4, 4 ),
 ( 0.0008018406558999754529, 0.003302116852321945566 ),
 .UNSPECIFIED. ) ;
#35911 = CARTESIAN_POINT ( 'NONE',  ( 0.000000000000000000, 1.574803149606302854, 0.000000000000000000 ) ) ;
#35912 = ORIENTED_EDGE ( 'NONE', *, *, #23246, .T. ) ;
#35913 = LINE ( 'NONE', #12161, #6993 ) ;
#35914 = CARTESIAN_POINT ( 'NONE',  ( -1.091055626815042201, 0.000000000000000000, 0.9448818897637749625 ) ) ;
#35915 = EDGE_CURVE ( 'NONE', #20856, #21785, #31383, .T. ) ;
#35916 = CARTESIAN_POINT ( 'NONE',  ( 0.000000000000000000, 2.755905511811027164, 0.000000000000000000 ) ) ;
#35917 = EDGE_CURVE ( 'NONE', #50600, #38070, #47961, .T. ) ;
#35918 = DIRECTION ( 'NONE',  ( -0.000000000000000000, 1.000000000000000000, -0.000000000000000000 ) ) ;
#35919 = EDGE_CURVE ( 'NONE', #8873, #8748, #29142, .T. ) ;
#35920 = FACE_OUTER_BOUND ( 'NONE', #8509, .T. ) ;
#35921 = ORIENTED_EDGE ( 'NONE', *, *, #8749, .F. ) ;
#35922 = VECTOR ( 'NONE', #47877, 39.37007874015748143 ) ;
#35923 = DIRECTION ( 'NONE',  ( 1.734723475976806848E-16, -0.000000000000000000, 1.000000000000000000 ) ) ;
#35924 = VECTOR ( 'NONE', #21951, 39.37007874015748143 ) ;
#35925 = ORIENTED_EDGE ( 'NONE', *, *, #46859, .T. ) ;
#35926 = VECTOR ( 'NONE', #34745, 39.37007874015748143 ) ;
#35927 = VERTEX_POINT ( 'NONE', #36392 ) ;
#35928 = LINE ( 'NONE', #16304, #15003 ) ;
#35929 = PLANE ( 'NONE',  #30325 ) ;
#35930 = FACE_OUTER_BOUND ( 'NONE', #5142, .T. ) ;
#35931 = CONICAL_SURFACE ( 'NONE', #38411, 3.483074324928249421, 1.244861948955335196 ) ;
#35932 = ORIENTED_EDGE ( 'NONE', *, *, #30211, .T. ) ;
#35933 = B_SPLINE_CURVE_WITH_KNOTS ( 'NONE', 3,
 ( #40961, #49663, #45060, #45808 ),
 .UNSPECIFIED., .F., .F.,
 ( 4, 4 ),
 ( 6.144603567270442506E-07, 0.001441218741676510108 ),
 .UNSPECIFIED. ) ;
#35934 = CIRCLE ( 'NONE', #3765, 2.443628662382284489 ) ;
#35935 = ORIENTED_EDGE ( 'NONE', *, *, #50886, .T. ) ;
#35936 = CARTESIAN_POINT ( 'NONE',  ( 1.472219874544873131, 1.742205712729733014, 2.560030851058970214 ) ) ;
#35938 = EDGE_LOOP ( 'NONE', ( #9134, #39499, #21616, #4577 ) ) ;
#35937 = EDGE_CURVE ( 'NONE', #40469, #39732, #42544, .T. ) ;
#35939 = CARTESIAN_POINT ( 'NONE',  ( 0.08119777152254364916, 1.623385212329073957, 0.000000000000000000 ) ) ;
#35940 = ORIENTED_EDGE ( 'NONE', *, *, #35249, .T. ) ;
#35941 = CARTESIAN_POINT ( 'NONE',  ( 1.983174097826134075, 0.5219917536725240392, 1.123077076632367888 ) ) ;
#35942 = EDGE_CURVE ( 'NONE', #21463, #22677, #29915, .T. ) ;
#35943 = CARTESIAN_POINT ( 'NONE',  ( -2.574515777086982204, 1.675047042282418852, 0.7847656960372165758 ) ) ;
#35944 = FACE_OUTER_BOUND ( 'NONE', #41845, .T. ) ;
#35945 = EDGE_CURVE ( 'NONE', #37143, #50043, #3205, .T. ) ;
#35946 = EDGE_LOOP ( 'NONE', ( #7641, #25514, #15393, #23749 ) ) ;
#35947 = VERTEX_POINT ( 'NONE', #34310 ) ;
#35948 = EDGE_LOOP ( 'NONE', ( #25778, #26862, #43297, #4425 ) ) ;
#35949 = CARTESIAN_POINT ( 'NONE',  ( -1.166969139818015533, 0.000000000000000000, 0.4724409448818871482 ) ) ;
#35950 = CARTESIAN_POINT ( 'NONE',  ( 2.182111253630085290, 0.000000000000000000, 0.4330708661417287386 ) ) ;
#35952 = VERTEX_POINT ( 'NONE', #7187 ) ;
#35951 = EDGE_CURVE ( 'NONE', #44591, #38140, #20956, .T. ) ;
#35953 = ORIENTED_EDGE ( 'NONE', *, *, #3682, .F. ) ;
#35954 = CARTESIAN_POINT ( 'NONE',  ( -1.826696687228679616, 0.5248816248417013108, -1.146824545754332680 ) ) ;
#35955 = CARTESIAN_POINT ( 'NONE',  ( 1.015142113812069091, 3.346456692913386100, -1.845530509571139399 ) ) ;
#35956 = DIRECTION ( 'NONE',  ( 0.000000000000000000, -1.000000000000000000, 0.000000000000000000 ) ) ;
#35957 = ORIENTED_EDGE ( 'NONE', *, *, #36990, .T. ) ;
#35958 = LINE ( 'NONE', #43936, #31246 ) ;
#35959 = CARTESIAN_POINT ( 'NONE',  ( -1.299212598425207865, 3.346456692913386100, 1.732283464566920950 ) ) ;
#35960 = LINE ( 'NONE', #43682, #33613 ) ;
#35961 = AXIS2_PLACEMENT_3D ( 'NONE', #43454, #28478, #44229 ) ;
#35962 = VERTEX_POINT ( 'NONE', #33807 ) ;
#35963 = LINE ( 'NONE', #24341, #10058 ) ;
#35964 = DIRECTION ( 'NONE',  ( -3.981026654148454344E-17, 1.000000000000000000, -1.225234019452869602E-16 ) ) ;
#35965 = AXIS2_PLACEMENT_3D ( 'NONE', #38643, #10760, #30129 ) ;
#35966 = EDGE_LOOP ( 'NONE', ( #38970, #14222, #47210, #14274 ) ) ;
#35967 = VECTOR ( 'NONE', #210, 39.37007874015748143 ) ;
#35968 = DIRECTION ( 'NONE',  ( 0.000000000000000000, 0.000000000000000000, 1.000000000000000000 ) ) ;
#35969 = EDGE_LOOP ( 'NONE', ( #38109, #24044, #12471, #33000 ) ) ;
#35970 = ORIENTED_EDGE ( 'NONE', *, *, #43608, .T. ) ;
#35971 = DIRECTION ( 'NONE',  ( -0.4338837391175656699, -1.045612331811453550E-16, 0.9009688679024154823 ) ) ;
#35972 = VECTOR ( 'NONE', #49374, 39.37007874015748143 ) ;
#35973 = CARTESIAN_POINT ( 'NONE',  ( 1.068075307999459822, 6.692913385826772199, 1.883606783264653028 ) ) ;
#35974 = VECTOR ( 'NONE', #9870, 39.37007874015748143 ) ;
#35975 = DIRECTION ( 'NONE',  ( -0.04486483035050446017, 1.288287287306305283E-16, -0.9989930665413151445 ) ) ;
#35976 = CARTESIAN_POINT ( 'NONE',  ( 2.919426793319799707, 1.666276233232717896, 0.4451252810446822417 ) ) ;
#35977 = EDGE_LOOP ( 'NONE', ( #36987, #10745, #6421, #3988 ) ) ;
#35978 = ORIENTED_EDGE ( 'NONE', *, *, #22942, .T. ) ;
#35979 = VECTOR ( 'NONE', #16976, 39.37007874015748143 ) ;
#35980 = PRODUCT ( 'Back Cover', 'Back Cover', '', ( #20399 ) ) ;
#35981 = ORIENTED_EDGE ( 'NONE', *, *, #38739, .T. ) ;
#35982 = FACE_OUTER_BOUND ( 'NONE', #32857, .T. ) ;
#35983 = LINE ( 'NONE', #43959, #21000 ) ;
#35984 = DIRECTION ( 'NONE',  ( 0.6234898018587319291, 1.288287287306305283E-16, 0.7818314824680311359 ) ) ;
#35985 = EDGE_CURVE ( 'NONE', #26538, #6620, #45631, .T. ) ;
#35986 = PLANE ( 'NONE',  #49914 ) ;
#35987 = DIRECTION ( 'NONE',  ( 0.7526474967735860000, 0.000000000000000000, -0.6584236824419781309 ) ) ;
#35988 = EDGE_LOOP ( 'NONE', ( #26678, #5533, #31700, #49531 ) ) ;
#35989 = EDGE_CURVE ( 'NONE', #19986, #45868, #38186, .T. ) ;
#35990 = DIRECTION ( 'NONE',  ( 0.9909497617679331460, -1.562041240006052286E-17, 0.1342332658176667026 ) ) ;
#35991 = CARTESIAN_POINT ( 'NONE',  ( 2.308557526972506047, 0.000000000000000000, 1.841013194464792724 ) ) ;
#35992 = EDGE_CURVE ( 'NONE', #8114, #20465, #3058, .T. ) ;
#35993 = VERTEX_POINT ( 'NONE', #18805 ) ;
#35994 = DIRECTION ( 'NONE',  ( -0.000000000000000000, 1.000000000000000000, -0.000000000000000000 ) ) ;
#35995 = CARTESIAN_POINT ( 'NONE',  ( 2.252332422952718183, 1.743977176619643910, -0.5645583697864726691 ) ) ;
#35996 = LINE ( 'NONE', #623, #744 ) ;
#35997 = ORIENTED_EDGE ( 'NONE', *, *, #23616, .T. ) ;
#35998 = AXIS2_PLACEMENT_3D ( 'NONE', #22404, #30406, #49465 ) ;
#35999 = PLANE ( 'NONE',  #19301 ) ;
#36000 = CARTESIAN_POINT ( 'NONE',  ( 2.277873973731426638, 1.463603380278871713, 1.879489153247667632 ) ) ;
#36001 = CARTESIAN_POINT ( 'NONE',  ( 1.363819533518803251, 3.267716535433071279, 1.102362204724403938 ) ) ;
#36002 = AXIS2_PLACEMENT_3D ( 'NONE', #47166, #7223, #23204 ) ;
#36003 = VECTOR ( 'NONE', #25436, 39.37007874015748143 ) ;
#36004 = ORIENTED_EDGE ( 'NONE', *, *, #19366, .T. ) ;
#36005 = DIRECTION ( 'NONE',  ( -1.000000000000000000, -0.000000000000000000, -0.000000000000000000 ) ) ;
#36006 = CARTESIAN_POINT ( 'NONE',  ( -0.04921259842519706829, 1.516406576848131849, 2.952755905511811108 ) ) ;
#36007 = ORIENTED_EDGE ( 'NONE', *, *, #19059, .F. ) ;
#36008 = CARTESIAN_POINT ( 'NONE',  ( 0.000000000000000000, 0.000000000000000000, 0.000000000000000000 ) ) ;
#36009 = CARTESIAN_POINT ( 'NONE',  ( 0.9959141370152501116, 1.049866565877818125, 1.762829326744137948 ) ) ;
#36010 = EDGE_CURVE ( 'NONE', #48217, #47654, #26041, .T. ) ;
#36011 = CARTESIAN_POINT ( 'NONE',  ( 0.2727639067037604392, 0.000000000000000000, 0.5905511811023579360 ) ) ;
#36012 = DIRECTION ( 'NONE',  ( -0.000000000000000000, 1.000000000000000000, -0.000000000000000000 ) ) ;
#36013 = AXIS2_PLACEMENT_3D ( 'NONE', #43760, #47865, #8417 ) ;
#36014 = CONICAL_SURFACE ( 'NONE', #13758, 2.244934639244524632, 1.554780866114618743 ) ;
#36015 = VERTEX_POINT ( 'NONE', #14166 ) ;
#36016 = VERTEX_POINT ( 'NONE', #45383 ) ;
#36017 = CARTESIAN_POINT ( 'NONE',  ( 0.000000000000000000, 3.267716535433071279, 0.000000000000000000 ) ) ;
#36018 = DIRECTION ( 'NONE',  ( 0.000000000000000000, -1.000000000000000000, 0.000000000000000000 ) ) ;
#36019 = B_SPLINE_CURVE_WITH_KNOTS ( 'NONE', 3,
 ( #3151, #15027, #30776, #15278 ),
 .UNSPECIFIED., .F., .F.,
 ( 4, 4 ),
 ( 2.330000277661172139E-07, 0.002500456362147902671 ),
 .UNSPECIFIED. ) ;
#36020 = EDGE_CURVE ( 'NONE', #48211, #47774, #10043, .T. ) ;
#36021 = ORIENTED_EDGE ( 'NONE', *, *, #45651, .F. ) ;
#36022 = DIRECTION ( 'NONE',  ( 1.734723475976806848E-16, 0.000000000000000000, 1.000000000000000000 ) ) ;
#36023 = DIRECTION ( 'NONE',  ( -0.9909497617679332571, 0.000000000000000000, -0.1342332658176667304 ) ) ;
#36024 = CARTESIAN_POINT ( 'NONE',  ( -1.252182360577274611, 1.655037561631665266, -1.807206635494494451 ) ) ;
#36025 = CARTESIAN_POINT ( 'NONE',  ( -0.3136974817027962104, 5.905511811023624880, -2.936457595020223632 ) ) ;
#36026 = ORIENTED_EDGE ( 'NONE', *, *, #5703, .F. ) ;
#36027 = ORIENTED_EDGE ( 'NONE', *, *, #40368, .F. ) ;
#36028 = DIRECTION ( 'NONE',  ( -3.469446951953613696E-16, 0.000000000000000000, -1.000000000000000000 ) ) ;
#36029 = DIRECTION ( 'NONE',  ( -0.9998717552508122886, -0.01601477604151182316, 0.000000000000000000 ) ) ;
#36030 = LINE ( 'NONE', #16407, #7394 ) ;
#36031 = CARTESIAN_POINT ( 'NONE',  ( -2.139229417893219853, 1.205361022782829114E-17, -0.3394403656973710159 ) ) ;
#36032 = FACE_BOUND ( 'NONE', #10636, .T. ) ;
#36033 = VERTEX_POINT ( 'NONE', #30429 ) ;
#36034 = DIRECTION ( 'NONE',  ( -0.000000000000000000, 1.000000000000000000, -0.000000000000000000 ) ) ;
#36035 = VERTEX_POINT ( 'NONE', #50241 ) ;
#36036 = ORIENTED_EDGE ( 'NONE', *, *, #9729, .F. ) ;
#36037 = CARTESIAN_POINT ( 'NONE',  ( 0.000000000000000000, 0.000000000000000000, 0.000000000000000000 ) ) ;
#36038 = AXIS2_PLACEMENT_3D ( 'NONE', #20229, #20497, #5005 ) ;
#36039 = ORIENTED_EDGE ( 'NONE', *, *, #34668, .T. ) ;
#36040 = ORIENTED_EDGE ( 'NONE', *, *, #25325, .F. ) ;
#36041 = FACE_OUTER_BOUND ( 'NONE', #2463, .T. ) ;
#36042 = B_SPLINE_CURVE_WITH_KNOTS ( 'NONE', 3,
 ( #39807, #32853, #48535, #5970 ),
 .UNSPECIFIED., .F., .F.,
 ( 4, 4 ),
 ( 0.1211775127643062444, 0.1625894504277921315 ),
 .UNSPECIFIED. ) ;
#36043 = ORIENTED_EDGE ( 'NONE', *, *, #8400, .T. ) ;
#36044 = AXIS2_PLACEMENT_3D ( 'NONE', #11021, #10767, #30392 ) ;
#36045 = LINE ( 'NONE', #15897, #32032 ) ;
#36046 = DIRECTION ( 'NONE',  ( -0.000000000000000000, 1.000000000000000000, -0.000000000000000000 ) ) ;
#36047 = CARTESIAN_POINT ( 'NONE',  ( 1.287906020515830141, 0.000000000000000000, 0.6299212598425161236 ) ) ;
#36048 = CARTESIAN_POINT ( 'NONE',  ( 0.2727639067037610499, 0.000000000000000000, 1.102362204724404160 ) ) ;
#36049 = EDGE_CURVE ( 'NONE', #4521, #1056, #14680, .T. ) ;
#36050 = DIRECTION ( 'NONE',  ( 0.000000000000000000, 0.000000000000000000, -1.000000000000000000 ) ) ;
#36051 = DIRECTION ( 'NONE',  ( 1.734723475976806848E-16, 0.000000000000000000, 1.000000000000000000 ) ) ;
#36052 = VERTEX_POINT ( 'NONE', #14930 ) ;
#36053 = EDGE_CURVE ( 'NONE', #5972, #47752, #11055, .T. ) ;
#36054 = DIRECTION ( 'NONE',  ( -0.000000000000000000, 1.000000000000000000, -0.000000000000000000 ) ) ;
#36055 = FACE_OUTER_BOUND ( 'NONE', #22324, .T. ) ;
#36056 = DIRECTION ( 'NONE',  ( -1.000000000000000000, 0.000000000000000000, -0.000000000000000000 ) ) ;
#36057 = EDGE_CURVE ( 'NONE', #24438, #10605, #10295, .T. ) ;
#36058 = ORIENTED_EDGE ( 'NONE', *, *, #14496, .F. ) ;
#36059 = LINE ( 'NONE', #35543, #38849 ) ;
#36060 = DIRECTION ( 'NONE',  ( -3.469446951953613696E-16, 0.000000000000000000, -1.000000000000000000 ) ) ;
#36061 = ORIENTED_EDGE ( 'NONE', *, *, #31488, .T. ) ;
#36062 = CARTESIAN_POINT ( 'NONE',  ( 1.530693736245519299, 5.905511811023623991, -1.531579597454042929 ) ) ;
#36063 = ADVANCED_FACE ( 'NONE', ( #26795 ), #37420, .F. ) ;
#36064 = DIRECTION ( 'NONE',  ( -1.000000000000000000, 0.000000000000000000, 0.000000000000000000 ) ) ;
#36065 = DIRECTION ( 'NONE',  ( -0.000000000000000000, 1.000000000000000000, -0.000000000000000000 ) ) ;
#36066 = EDGE_LOOP ( 'NONE', ( #25907, #26729, #22984, #12932, #18943, #41964, #16512, #41015, #8079, #1242, #49422, #37883, #25939 ) ) ;
#36067 = FACE_OUTER_BOUND ( 'NONE', #9792, .T. ) ;
#36068 = ORIENTED_EDGE ( 'NONE', *, *, #32631, .T. ) ;
#36069 = LINE ( 'NONE', #27173, #19005 ) ;
#36070 = DIRECTION ( 'NONE',  ( -0.07365742419378766559, 0.000000000000000000, 0.9972836025229415702 ) ) ;
#36071 = LINE ( 'NONE', #24454, #21827 ) ;
#36072 = EDGE_CURVE ( 'NONE', #7052, #28425, #33554, .T. ) ;
#36073 = DIRECTION ( 'NONE',  ( 1.734723475976806848E-16, -0.000000000000000000, 1.000000000000000000 ) ) ;
#36074 = AXIS2_PLACEMENT_3D ( 'NONE', #27684, #47786, #4719 ) ;
#36075 = VECTOR ( 'NONE', #8501, 39.37007874015748143 ) ;
#36076 = ORIENTED_EDGE ( 'NONE', *, *, #45268, .F. ) ;
#36077 = ORIENTED_EDGE ( 'NONE', *, *, #50594, .F. ) ;
#36078 = CARTESIAN_POINT ( 'NONE',  ( 1.854041947016408010, 0.000000000000000000, 1.016381156669627694 ) ) ;
#36079 = ORIENTED_EDGE ( 'NONE', *, *, #27108, .F. ) ;
#36080 = ADVANCED_FACE ( 'NONE', ( #34053 ), #49239, .F. ) ;
#36081 = CARTESIAN_POINT ( 'NONE',  ( 0.000000000000000000, 3.267716535433071279, -6.146657985744592735E-16 ) ) ;
#36082 = ORIENTED_EDGE ( 'NONE', *, *, #46291, .F. ) ;
#36083 = CARTESIAN_POINT ( 'NONE',  ( 1.909347346926324684, 3.267716535433071279, 0.1574803149606280872 ) ) ;
#36084 = EDGE_LOOP ( 'NONE', ( #28114, #44358, #40599, #41595 ) ) ;
#36085 = EDGE_CURVE ( 'NONE', #2922, #42532, #21922, .T. ) ;
#36086 = FACE_OUTER_BOUND ( 'NONE', #18555, .T. ) ;
#36087 = CARTESIAN_POINT ( 'NONE',  ( -1.091055626815042645, 0.000000000000000000, -1.259842519685034690 ) ) ;
#36088 = ORIENTED_EDGE ( 'NONE', *, *, #49323, .T. ) ;
#36089 = PRODUCT_DEFINITION_CONTEXT ( 'detailed design', #7464, 'design' ) ;
#36090 = DIRECTION ( 'NONE',  ( -0.000000000000000000, 0.000000000000000000, 1.000000000000000000 ) ) ;
#36091 = EDGE_LOOP ( 'NONE', ( #9682, #5345, #21776, #31919, #35691, #18763 ) ) ;
#36092 = AXIS2_PLACEMENT_3D ( 'NONE', #5825, #18210, #2211 ) ;
#36093 = EDGE_CURVE ( 'NONE', #48706, #21112, #14426, .T. ) ;
#36094 = LINE ( 'NONE', #28329, #36147 ) ;
#36095 = VERTEX_POINT ( 'NONE', #50484 ) ;
#36096 = VERTEX_POINT ( 'NONE', #42792 ) ;
#36097 = CARTESIAN_POINT ( 'NONE',  ( -2.161044708975090156, 0.000000000000000000, 0.1463148319730351032 ) ) ;
#36098 = CARTESIAN_POINT ( 'NONE',  ( 2.005112362574620111, 0.03937352102360182349, 0.2219488725060905498 ) ) ;
#36099 = EDGE_LOOP ( 'NONE', ( #1554, #36280, #3633, #1069 ) ) ;
#36100 = CARTESIAN_POINT ( 'NONE',  ( 0.1525302393087137887, 1.710345001767278994, -2.243756654240526505 ) ) ;
#36101 = ORIENTED_EDGE ( 'NONE', *, *, #37803, .F. ) ;
#36102 = DIRECTION ( 'NONE',  ( -0.000000000000000000, 1.000000000000000000, -0.000000000000000000 ) ) ;
#36103 = LINE ( 'NONE', #36361, #32484 ) ;
#36104 = VECTOR ( 'NONE', #19978, 39.37007874015748143 ) ;
#36105 = VECTOR ( 'NONE', #15988, 39.37007874015748143 ) ;
#36106 = LINE ( 'NONE', #27833, #36303 ) ;
#36107 = VERTEX_POINT ( 'NONE', #30933 ) ;
#36108 = VERTEX_POINT ( 'NONE', #50735 ) ;
#36109 = FACE_OUTER_BOUND ( 'NONE', #1871, .T. ) ;
#36110 = LINE ( 'NONE', #16231, #4844 ) ;
#36111 = CARTESIAN_POINT ( 'NONE',  ( 0.08119777152254364916, 1.623385212329073957, 0.000000000000000000 ) ) ;
#36112 = AXIS2_PLACEMENT_3D ( 'NONE', #29159, #44893, #18310 ) ;
#36113 = CARTESIAN_POINT ( 'NONE',  ( -2.164823134740036181, 5.905511811023623991, -0.04796011690018279344 ) ) ;
#36114 = CARTESIAN_POINT ( 'NONE',  ( -2.867773316779185677, 1.674559808355669199, -0.7050287376752426560 ) ) ;
#36115 = EDGE_CURVE ( 'NONE', #13057, #47970, #15440, .T. ) ;
#36116 = DIRECTION ( 'NONE',  ( 1.000000000000000000, 0.000000000000000000, 0.000000000000000000 ) ) ;
#36117 = EDGE_CURVE ( 'NONE', #16479, #44707, #35315, .T. ) ;
#36118 = ORIENTED_EDGE ( 'NONE', *, *, #47172, .T. ) ;
#36119 = EDGE_CURVE ( 'NONE', #49090, #27844, #12272, .T. ) ;
#36120 = CARTESIAN_POINT ( 'NONE',  ( 0.08139965876239094178, 1.610780518492231694, 0.000000000000000000 ) ) ;
#36121 = VECTOR ( 'NONE', #19313, 39.37007874015748143 ) ;
#36122 = EDGE_LOOP ( 'NONE', ( #37389, #7301, #21602, #48009 ) ) ;
#36123 = CARTESIAN_POINT ( 'NONE',  ( 1.909347346926324462, 0.000000000000000000, -1.299212598425194320 ) ) ;
#36124 = VECTOR ( 'NONE', #1760, 39.37007874015748143 ) ;
#36125 = ORIENTED_EDGE ( 'NONE', *, *, #8343, .F. ) ;
#36126 = CARTESIAN_POINT ( 'NONE',  ( -0.8942052331142547050, 3.267716535433071279, 0.9448818897637749625 ) ) ;
#36127 = B_SPLINE_CURVE_WITH_KNOTS ( 'NONE', 3,
 ( #45955, #30998, #10621, #11372 ),
 .UNSPECIFIED., .F., .F.,
 ( 4, 4 ),
 ( 6.128883314497806983E-05, 0.002561329735754209504 ),
 .UNSPECIFIED. ) ;
#36128 = CARTESIAN_POINT ( 'NONE',  ( -1.882988517681398966, 1.574803149606302854, 1.069164917025789530 ) ) ;
#36129 = CARTESIAN_POINT ( 'NONE',  ( 0.5455278134075212115, 3.346456692913386100, 0.6299212598425161236 ) ) ;
#36130 = DIRECTION ( 'NONE',  ( 0.000000000000000000, 1.000000000000000000, 0.000000000000000000 ) ) ;
#36131 = ORIENTED_EDGE ( 'NONE', *, *, #15710, .T. ) ;
#36132 = LINE ( 'NONE', #762, #33224 ) ;
#36133 = FACE_BOUND ( 'NONE', #41269, .T. ) ;
#36134 = ORIENTED_EDGE ( 'NONE', *, *, #11167, .T. ) ;
#36135 = CARTESIAN_POINT ( 'NONE',  ( 1.833433833923351353, 3.267716535433071279, 1.574803149606291974 ) ) ;
#36136 = VERTEX_POINT ( 'NONE', #28763 ) ;
#36137 = DIRECTION ( 'NONE',  ( 1.000000000000000000, 0.000000000000000000, 0.000000000000000000 ) ) ;
#36138 = CARTESIAN_POINT ( 'NONE',  ( 2.823445274216730638, 1.763256531483745837, 0.8656477926280683466 ) ) ;
#36139 = CONICAL_SURFACE ( 'NONE', #24606, 3.033577403570480779, 1.554780866114618743 ) ;
#36140 = EDGE_CURVE ( 'NONE', #2179, #33261, #3559, .T. ) ;
#36141 = DIRECTION ( 'NONE',  ( 0.1785568947986370669, 0.000000000000000000, -0.9839295885986296675 ) ) ;
#36142 = ORIENTED_EDGE ( 'NONE', *, *, #5327, .F. ) ;
#36143 = ORIENTED_EDGE ( 'NONE', *, *, #50400, .F. ) ;
#36144 = LINE ( 'NONE', #776, #29295 ) ;
#36145 = CARTESIAN_POINT ( 'NONE',  ( 2.051629384040484005, 0.01961290521451679661, 0.3275741348515084916 ) ) ;
#36146 = DIRECTION ( 'NONE',  ( 1.734723475976806848E-16, 0.000000000000000000, 1.000000000000000000 ) ) ;
#36147 = VECTOR ( 'NONE', #973, 39.37007874015748143 ) ;
#36148 = EDGE_CURVE ( 'NONE', #34660, #18225, #11806, .T. ) ;
#36149 = VECTOR ( 'NONE', #26349, 39.37007874015748143 ) ;
#36150 = DIRECTION ( 'NONE',  ( 0.000000000000000000, 0.000000000000000000, -1.000000000000000000 ) ) ;
#36151 = CARTESIAN_POINT ( 'NONE',  ( -1.712496953225537855, 3.267716535433071279, -1.226315847645294221 ) ) ;
#36152 = ADVANCED_FACE ( 'NONE', ( #31185 ), #11310, .T. ) ;
#36153 = VERTEX_POINT ( 'NONE', #44505 ) ;
#36154 = VECTOR ( 'NONE', #35275, 39.37007874015748143 ) ;
#36155 = CARTESIAN_POINT ( 'NONE',  ( -2.623503965249869729, 1.579940539283962053, 1.355882097269835107 ) ) ;
#36156 = EDGE_CURVE ( 'NONE', #5661, #34145, #18020, .T. ) ;
#36157 = VERTEX_POINT ( 'NONE', #32661 ) ;
#36158 = ORIENTED_EDGE ( 'NONE', *, *, #45054, .T. ) ;
#36159 = APPLICATION_PROTOCOL_DEFINITION ( 'draft international standard', 'automotive_design', 1998, #49646 ) ;
#36160 = AXIS2_PLACEMENT_3D ( 'NONE', #15162, #11292, #27787 ) ;
#36162 = EDGE_CURVE ( 'NONE', #15505, #10535, #46885, .T. ) ;
#36161 = ORIENTED_EDGE ( 'NONE', *, *, #5684, .T. ) ;
#36163 = DIRECTION ( 'NONE',  ( 0.000000000000000000, 1.000000000000000000, 0.000000000000000000 ) ) ;
#36164 = DIRECTION ( 'NONE',  ( -3.469446951953613696E-16, 0.000000000000000000, -1.000000000000000000 ) ) ;
#36165 = VECTOR ( 'NONE', #49456, 39.37007874015748143 ) ;
#36166 = DIRECTION ( 'NONE',  ( -3.469446951953613696E-16, 0.000000000000000000, -1.000000000000000000 ) ) ;
#36167 = CARTESIAN_POINT ( 'NONE',  ( 1.091055626815043311, 3.346456692913386100, 1.377952755905504256 ) ) ;
#36168 = ORIENTED_EDGE ( 'NONE', *, *, #22634, .T. ) ;
#36169 = ORIENTED_EDGE ( 'NONE', *, *, #47032, .T. ) ;
#36170 = LINE ( 'NONE', #17067, #34030 ) ;
#36171 = DIRECTION ( 'NONE',  ( 1.000000000000000000, 0.000000000000000000, -3.469446951953613696E-16 ) ) ;
#36172 = FACE_OUTER_BOUND ( 'NONE', #9139, .T. ) ;
#36173 = LINE ( 'NONE', #8800, #50640 ) ;
#36174 = LINE ( 'NONE', #801, #42902 ) ;
#36175 = EDGE_CURVE ( 'NONE', #11955, #35311, #11558, .T. ) ;
#36176 = CARTESIAN_POINT ( 'NONE',  ( -0.4788131938641533303, 1.711801685632677428, 2.914091152102185944 ) ) ;
#36177 = VECTOR ( 'NONE', #27741, 39.37007874015748143 ) ;
#36178 = EDGE_CURVE ( 'NONE', #36611, #47661, #38787, .T. ) ;
#36179 = EDGE_CURVE ( 'NONE', #10330, #13544, #12067, .T. ) ;
#36180 = DIRECTION ( 'NONE',  ( -0.8439299085898971375, 0.000000000000000000, 0.5364534550056020423 ) ) ;
#36181 = DIRECTION ( 'NONE',  ( 1.000000000000000000, 0.000000000000000000, -3.469446951953613696E-16 ) ) ;
#36182 = VERTEX_POINT ( 'NONE', #50991 ) ;
#36183 = DIRECTION ( 'NONE',  ( 1.734723475976806848E-16, -0.000000000000000000, 1.000000000000000000 ) ) ;
#36184 = LINE ( 'NONE', #32313, #30178 ) ;
#36185 = EDGE_LOOP ( 'NONE', ( #40211, #43559, #36027, #24665 ) ) ;
#36186 = VERTEX_POINT ( 'NONE', #20766 ) ;
#36187 = VECTOR ( 'NONE', #46773, 39.37007874015748143 ) ;
#36189 = PLANE ( 'NONE',  #1843 ) ;
#36188 = VECTOR ( 'NONE', #32788, 39.37007874015748143 ) ;
#36190 = CARTESIAN_POINT ( 'NONE',  ( 0.8182917201112819283, 3.267716535433071279, 0.7874015748031454320 ) ) ;
#36191 = CARTESIAN_POINT ( 'NONE',  ( 1.847133430398848697, 0.5249316497054296038, -0.3711179597262244112 ) ) ;
#36192 = VERTEX_POINT ( 'NONE', #4077 ) ;
#36193 = VECTOR ( 'NONE', #15020, 39.37007874015748143 ) ;
#36194 = ORIENTED_EDGE ( 'NONE', *, *, #29400, .F. ) ;
#36195 = DIRECTION ( 'NONE',  ( 0.000000000000000000, 1.000000000000000000, -0.000000000000000000 ) ) ;
#36196 = EDGE_LOOP ( 'NONE', ( #20783, #46969, #10644, #26995 ) ) ;
#36197 = AXIS2_PLACEMENT_3D ( 'NONE', #41396, #10409, #41650 ) ;
#36198 = DIRECTION ( 'NONE',  ( 0.000000000000000000, 0.000000000000000000, 1.000000000000000000 ) ) ;
#36199 = ORIENTED_EDGE ( 'NONE', *, *, #45555, .T. ) ;
#36200 = LINE ( 'NONE', #35681, #13641 ) ;
#36201 = CARTESIAN_POINT ( 'NONE',  ( 1.979793062125284830, 1.470624965921384364, 2.191257344206569257 ) ) ;
#36202 = DIRECTION ( 'NONE',  ( 0.000000000000000000, 0.000000000000000000, 1.000000000000000000 ) ) ;
#36203 = EDGE_CURVE ( 'NONE', #6756, #1365, #27804, .T. ) ;
#36204 = ORIENTED_EDGE ( 'NONE', *, *, #38413, .F. ) ;
#36205 = ORIENTED_EDGE ( 'NONE', *, *, #46796, .F. ) ;
#36206 = ORIENTED_EDGE ( 'NONE', *, *, #20900, .T. ) ;
#36207 = CARTESIAN_POINT ( 'NONE',  ( -1.091055626815042645, 3.267716535433071279, 2.186531193194249045 ) ) ;
#36208 = ORIENTED_EDGE ( 'NONE', *, *, #23929, .F. ) ;
#36209 = VERTEX_POINT ( 'NONE', #39690 ) ;
#36210 = CARTESIAN_POINT ( 'NONE',  ( -1.087426130748108788, 0.01050254589070086231, -1.412988192946641020 ) ) ;
#36211 = DIRECTION ( 'NONE',  ( -3.469446951953613696E-16, 0.000000000000000000, -1.000000000000000000 ) ) ;
#36212 = CARTESIAN_POINT ( 'NONE',  ( -1.363819533518803473, 3.346456692913386100, -1.417322834645664109 ) ) ;
#36213 = EDGE_CURVE ( 'NONE', #34811, #37003, #3574, .T. ) ;
#36214 = ORIENTED_EDGE ( 'NONE', *, *, #20502, .F. ) ;
#36215 = EDGE_CURVE ( 'NONE', #25499, #24416, #19045, .T. ) ;
#36216 = CARTESIAN_POINT ( 'NONE',  ( 0.000000000000000000, 2.755905511811023612, 0.000000000000000000 ) ) ;
#36217 = CARTESIAN_POINT ( 'NONE',  ( -0.9259623415327485896, 0.000000000000000000, 1.581646091660971143 ) ) ;
#36218 = VECTOR ( 'NONE', #6562, 39.37007874015748143 ) ;
#36219 = CARTESIAN_POINT ( 'NONE',  ( 0.5455278134075213226, 3.267716535433071279, -9.463399047163224412E-17 ) ) ;
#36220 = EDGE_CURVE ( 'NONE', #36221, #44686, #4017, .T. ) ;
#36221 = VERTEX_POINT ( 'NONE', #34804 ) ;
#36222 = DIRECTION ( 'NONE',  ( -0.000000000000000000, 1.000000000000000000, -0.000000000000000000 ) ) ;
#36223 = LINE ( 'NONE', #32099, #39236 ) ;
#36224 = ORIENTED_EDGE ( 'NONE', *, *, #5556, .T. ) ;
#36225 = CARTESIAN_POINT ( 'NONE',  ( 1.083598637574782142, 1.491270273546293046, 2.747180975113346246 ) ) ;
#36226 = ORIENTED_EDGE ( 'NONE', *, *, #22834, .F. ) ;
#36227 = EDGE_LOOP ( 'NONE', ( #603, #8352, #5468, #45792 ) ) ;
#36228 = LINE ( 'NONE', #853, #44351 ) ;
#36229 = DIRECTION ( 'NONE',  ( 1.000000000000000000, 0.000000000000000000, 0.000000000000000000 ) ) ;
#36230 = VECTOR ( 'NONE', #36776, 39.37007874015748143 ) ;
#36231 = CARTESIAN_POINT ( 'NONE',  ( 1.775400203342704986, 1.648464234653929106, -2.359903268218703332 ) ) ;
#36232 = CARTESIAN_POINT ( 'NONE',  ( -0.3452076480189834040, 0.5241083961098278454, 2.177863912564995008 ) ) ;
#36234 = VECTOR ( 'NONE', #21018, 39.37007874015748143 ) ;
#36233 = LINE ( 'NONE', #36485, #4052 ) ;
#36235 = ORIENTED_EDGE ( 'NONE', *, *, #25184, .T. ) ;
#36236 = ORIENTED_EDGE ( 'NONE', *, *, #2481, .T. ) ;
#36237 = CARTESIAN_POINT ( 'NONE',  ( 2.074656761899007495, 1.205361022782829114E-17, -0.6223516566630619140 ) ) ;
#36238 = ADVANCED_FACE ( 'NONE', ( #15180 ), #17664, .T. ) ;
#36239 = AXIS2_PLACEMENT_3D ( 'NONE', #39035, #7542, #19655 ) ;
#36240 = ORIENTED_EDGE ( 'NONE', *, *, #34608, .T. ) ;
#36241 = LINE ( 'NONE', #12227, #18685 ) ;
#36242 = CARTESIAN_POINT ( 'NONE',  ( -1.439733046521776139, 3.346456692913386100, 1.259842519685033357 ) ) ;
#36243 = EDGE_CURVE ( 'NONE', #33537, #22117, #13793, .T. ) ;
#36244 = DIRECTION ( 'NONE',  ( -0.01601477604151182663, 0.9998717552508123996, -0.000000000000000000 ) ) ;
#36245 = LINE ( 'NONE', #1114, #499 ) ;
#36246 = CARTESIAN_POINT ( 'NONE',  ( 2.016369045219287948, 1.641772594434526278, 1.140940039539855677 ) ) ;
#36247 = ORIENTED_EDGE ( 'NONE', *, *, #25570, .T. ) ;
#36248 = EDGE_CURVE ( 'NONE', #39521, #40227, #23791, .T. ) ;
#36249 = CARTESIAN_POINT ( 'NONE',  ( 0.08139965876239094178, 1.610780518492231694, 0.000000000000000000 ) ) ;
#36250 = EDGE_CURVE ( 'NONE', #36296, #12695, #1654, .T. ) ;
#36251 = FACE_OUTER_BOUND ( 'NONE', #33145, .T. ) ;
#36252 = EDGE_LOOP ( 'NONE', ( #10070, #31103, #34108, #5612 ) ) ;
#36253 = CARTESIAN_POINT ( 'NONE',  ( -2.338262049203568171, 2.755905511811027164, -0.7080022065394829811 ) ) ;
#36254 = CARTESIAN_POINT ( 'NONE',  ( -1.068402561569948617, 1.205361022782829114E-17, -1.884154513482188431 ) ) ;
#36255 = DIRECTION ( 'NONE',  ( -0.000000000000000000, -1.000000000000000000, -0.000000000000000000 ) ) ;
#36256 = VECTOR ( 'NONE', #48478, 39.37007874015748143 ) ;
#36257 = EDGE_LOOP ( 'NONE', ( #46575, #12180, #19316, #20203 ) ) ;
#36258 = DIRECTION ( 'NONE',  ( -1.000000000000000000, 0.000000000000000000, 1.734723475976806848E-16 ) ) ;
#36259 = DIRECTION ( 'NONE',  ( -1.000000000000000000, 0.000000000000000000, 1.734723475976806848E-16 ) ) ;
#36260 = CARTESIAN_POINT ( 'NONE',  ( -1.299212598425207865, 3.346456692913386100, 1.732283464566920950 ) ) ;
#36261 = ORIENTED_EDGE ( 'NONE', *, *, #27076, .T. ) ;
#36262 = LINE ( 'NONE', #39869, #24703 ) ;
#36263 = DIRECTION ( 'NONE',  ( 1.734723475976806848E-16, 0.000000000000000000, 1.000000000000000000 ) ) ;
#36264 = ORIENTED_EDGE ( 'NONE', *, *, #20695, .F. ) ;
#36265 = FACE_OUTER_BOUND ( 'NONE', #25248, .T. ) ;
#36266 = VECTOR ( 'NONE', #29750, 39.37007874015748143 ) ;
#36267 = DIRECTION ( 'NONE',  ( -1.000000000000000000, 0.000000000000000000, -0.000000000000000000 ) ) ;
#36268 = PLANE ( 'NONE',  #24707 ) ;
#36269 = DIRECTION ( 'NONE',  ( 0.2660368455666826115, 0.000000000000000000, -0.9639628606958511314 ) ) ;
#36270 = ORIENTED_EDGE ( 'NONE', *, *, #20764, .F. ) ;
#36271 = VERTEX_POINT ( 'NONE', #33169 ) ;
#36272 = DIRECTION ( 'NONE',  ( -1.105928667600727183E-16, 1.000000000000000000, 6.607616187506045307E-17 ) ) ;
#36273 = PLANE ( 'NONE',  #36999 ) ;
#36274 = EDGE_LOOP ( 'NONE', ( #47934, #5236, #37121, #24450 ) ) ;
#36275 = CARTESIAN_POINT ( 'NONE',  ( -1.091055626815042645, 3.346456692913386100, 1.889763779527550147 ) ) ;
#36276 = CARTESIAN_POINT ( 'NONE',  ( 1.062992125984252079, 0.4235180831842795257, 1.014069264286641792 ) ) ;
#36277 = VECTOR ( 'NONE', #43665, 39.37007874015748143 ) ;
#36278 = PLANE ( 'NONE',  #15408 ) ;
#36279 = PLANE ( 'NONE',  #47903 ) ;
#36280 = ORIENTED_EDGE ( 'NONE', *, *, #26840, .F. ) ;
#36281 = ORIENTED_EDGE ( 'NONE', *, *, #12383, .F. ) ;
#36282 = ADVANCED_FACE ( 'NONE', ( #25658 ), #21793, .F. ) ;
#36283 = CARTESIAN_POINT ( 'NONE',  ( 0.5455278134075208785, 3.267716535433071279, -1.889763779527552812 ) ) ;
#36284 = CARTESIAN_POINT ( 'NONE',  ( 1.636583440222563635, 0.000000000000000000, -1.456692913385823296 ) ) ;
#36285 = DIRECTION ( 'NONE',  ( 1.156482317317871478E-16, 0.000000000000000000, 1.000000000000000000 ) ) ;
#36286 = CARTESIAN_POINT ( 'NONE',  ( -0.2727639067037608278, 0.000000000000000000, 2.165354330708650465 ) ) ;
#36287 = EDGE_CURVE ( 'NONE', #7564, #41617, #48602, .T. ) ;
#36288 = FACE_BOUND ( 'NONE', #25487, .T. ) ;
#36289 = ORIENTED_EDGE ( 'NONE', *, *, #14272, .T. ) ;
#36290 = EDGE_CURVE ( 'NONE', #4750, #42832, #6034, .T. ) ;
#36291 = DIRECTION ( 'NONE',  ( 0.000000000000000000, 0.000000000000000000, -1.000000000000000000 ) ) ;
#36292 = VERTEX_POINT ( 'NONE', #29276 ) ;
#36293 = ORIENTED_EDGE ( 'NONE', *, *, #36794, .F. ) ;
#36294 = PLANE ( 'NONE',  #44022 ) ;
#36295 = ORIENTED_EDGE ( 'NONE', *, *, #34545, .T. ) ;
#36296 = VERTEX_POINT ( 'NONE', #37293 ) ;
#36297 = DIRECTION ( 'NONE',  ( -0.01601477604151182663, 0.9998717552508123996, -0.000000000000000000 ) ) ;
#36298 = ORIENTED_EDGE ( 'NONE', *, *, #18064, .T. ) ;
#36299 = EDGE_CURVE ( 'NONE', #15323, #8660, #5532, .T. ) ;
#36300 = DIRECTION ( 'NONE',  ( 1.000000000000000000, 0.000000000000000000, 0.000000000000000000 ) ) ;
#36301 = CARTESIAN_POINT ( 'NONE',  ( 1.636583440222563857, 3.346456692913386100, 1.259842519685033135 ) ) ;
#36302 = FACE_OUTER_BOUND ( 'NONE', #15752, .T. ) ;
#36303 = VECTOR ( 'NONE', #40490, 39.37007874015748143 ) ;
#36304 = EDGE_CURVE ( 'NONE', #30628, #25553, #2396, .T. ) ;
#36305 = CIRCLE ( 'NONE', #3309, 1.850107469027523432 ) ;
#36306 = CARTESIAN_POINT ( 'NONE',  ( -2.150518151785907772, 1.673457466938482296, -0.2530435858860717313 ) ) ;
#36307 = CARTESIAN_POINT ( 'NONE',  ( 1.833433833923351353, 3.346456692913386100, 1.152076279655074087 ) ) ;
#36308 = LINE ( 'NONE', #8425, #41038 ) ;
#36309 = VERTEX_POINT ( 'NONE', #49111 ) ;
#36310 = LINE ( 'NONE', #5064, #33264 ) ;
#36311 = EDGE_CURVE ( 'NONE', #42995, #47754, #40904, .T. ) ;
#36312 = VECTOR ( 'NONE', #40270, 39.37007874015748143 ) ;
#36314 = EDGE_CURVE ( 'NONE', #25804, #29354, #29538, .T. ) ;
#36313 = DIRECTION ( 'NONE',  ( 1.000000000000000000, 0.000000000000000000, 0.000000000000000000 ) ) ;
#36315 = LINE ( 'NONE', #28550, #46245 ) ;
#36316 = EDGE_LOOP ( 'NONE', ( #41923, #44706, #1738, #840 ) ) ;
#36317 = LINE ( 'NONE', #16178, #7516 ) ;
#36318 = CARTESIAN_POINT ( 'NONE',  ( 0.8182917201112819283, 3.267716535433071279, -1.102362204724405714 ) ) ;
#36319 = ORIENTED_EDGE ( 'NONE', *, *, #36702, .T. ) ;
#36320 = CARTESIAN_POINT ( 'NONE',  ( -0.3486774197067339376, 0.000000000000000000, 0.3149606299212577287 ) ) ;
#36321 = DIRECTION ( 'NONE',  ( 1.734723475976806848E-16, -0.000000000000000000, 1.000000000000000000 ) ) ;
#36322 = CARTESIAN_POINT ( 'NONE',  ( -1.748857564167104472, 1.593560878921895352, -2.379187624385278532 ) ) ;
#36323 = ORIENTED_EDGE ( 'NONE', *, *, #21854, .T. ) ;
#36324 = CARTESIAN_POINT ( 'NONE',  ( -0.6214413264104939882, 0.000000000000000000, 0.5905511811023582691 ) ) ;
#36325 = ORIENTED_EDGE ( 'NONE', *, *, #13860, .T. ) ;
#36326 = FACE_BOUND ( 'NONE', #49259, .T. ) ;
#36327 = CARTESIAN_POINT ( 'NONE',  ( 1.571584482197274202, 0.9990897620696875814, -2.079374994526344000 ) ) ;
#36328 = CARTESIAN_POINT ( 'NONE',  ( -0.9916727432047125479, 0.5239746995928241668, -1.945806201603022645 ) ) ;
#36329 = DIRECTION ( 'NONE',  ( -0.8268442224656336048, 0.000000000000000000, -0.5624310017906212211 ) ) ;
#36330 = B_SPLINE_CURVE_WITH_KNOTS ( 'NONE', 3,
 ( #48471, #44879, #25280, #13157 ),
 .UNSPECIFIED., .F., .F.,
 ( 4, 4 ),
 ( 7.902280897695455319E-07, 0.002031616469162080257 ),
 .UNSPECIFIED. ) ;
#36331 = VERTEX_POINT ( 'NONE', #17406 ) ;
#36332 = ORIENTED_EDGE ( 'NONE', *, *, #1783, .F. ) ;
#36333 = DIRECTION ( 'NONE',  ( -3.469446951953613696E-16, 0.000000000000000000, -1.000000000000000000 ) ) ;
#36334 = ORIENTED_EDGE ( 'NONE', *, *, #47386, .F. ) ;
#36335 = PLANE ( 'NONE',  #26062 ) ;
#36336 = VERTEX_POINT ( 'NONE', #48851 ) ;
#36337 = AXIS2_PLACEMENT_3D ( 'NONE', #20415, #8801, #28409 ) ;
#36338 = CARTESIAN_POINT ( 'NONE',  ( 1.236813753895252166, 1.487789312410982445, -2.681693691597563767 ) ) ;
#36339 = AXIS2_PLACEMENT_3D ( 'NONE', #8578, #20703, #19924 ) ;
#36340 = ORIENTED_EDGE ( 'NONE', *, *, #46694, .F. ) ;
#36341 = CARTESIAN_POINT ( 'NONE',  ( -0.2727639067037602172, 3.267716535433071279, 1.732283464566921172 ) ) ;
#36342 = DIRECTION ( 'NONE',  ( 1.734723475976806848E-16, 0.000000000000000000, 1.000000000000000000 ) ) ;
#36343 = EDGE_CURVE ( 'NONE', #41040, #21385, #25915, .T. ) ;
#36344 = EDGE_LOOP ( 'NONE', ( #15088, #27105, #2674 ) ) ;
#36345 = ADVANCED_FACE ( 'NONE', ( #45009 ), #49367, .F. ) ;
#36346 = CARTESIAN_POINT ( 'NONE',  ( -0.5455278134075214336, 3.346456692913386100, -2.034427629037601104 ) ) ;
#36347 = ORIENTED_EDGE ( 'NONE', *, *, #37981, .T. ) ;
#36348 = AXIS2_PLACEMENT_3D ( 'NONE', #5603, #21357, #24203 ) ;
#36349 = B_SPLINE_CURVE_WITH_KNOTS ( 'NONE', 3,
 ( #28346, #44348, #5629, #48442 ),
 .UNSPECIFIED., .F., .F.,
 ( 4, 4 ),
 ( 0.01475822760527119651, 0.03075144468528176467 ),
 .UNSPECIFIED. ) ;
#36350 = EDGE_CURVE ( 'NONE', #48914, #15499, #40648, .T. ) ;
#36351 = EDGE_CURVE ( 'NONE', #7776, #31368, #22575, .T. ) ;
#36352 = CARTESIAN_POINT ( 'NONE',  ( 1.560669927219590303, 3.240767787252049281, -1.896658215779326362 ) ) ;
#36354 = ORIENTED_EDGE ( 'NONE', *, *, #47007, .T. ) ;
#36353 = EDGE_CURVE ( 'NONE', #30078, #36589, #37578, .T. ) ;
#36355 = ORIENTED_EDGE ( 'NONE', *, *, #46908, .T. ) ;
#36356 = CARTESIAN_POINT ( 'NONE',  ( 1.566245445154855531, 1.172985819482486924, -0.9842519685039369248 ) ) ;
#36357 = EDGE_LOOP ( 'NONE', ( #15576, #38490, #46759, #15868 ) ) ;
#36358 = CARTESIAN_POINT ( 'NONE',  ( -1.363819533518803029, 0.000000000000000000, 0.1574803149606287811 ) ) ;
#36359 = ORIENTED_EDGE ( 'NONE', *, *, #35713, .T. ) ;
#36360 = CARTESIAN_POINT ( 'NONE',  ( 2.755905511811024056, 2.913385826771657250, -1.023622047244094224 ) ) ;
#36361 = CARTESIAN_POINT ( 'NONE',  ( 1.636583440222563857, 0.000000000000000000, -0.5118110236220471121 ) ) ;
#36362 = EDGE_CURVE ( 'NONE', #16605, #19346, #45791, .T. ) ;
#36363 = PLANE ( 'NONE',  #35446 ) ;
#36364 = ORIENTED_EDGE ( 'NONE', *, *, #11911, .T. ) ;
#36365 = CARTESIAN_POINT ( 'NONE',  ( 0.000000000000000000, 3.267716535433071279, 0.000000000000000000 ) ) ;
#36366 = CARTESIAN_POINT ( 'NONE',  ( 0.000000000000000000, 6.692913385826772199, 0.000000000000000000 ) ) ;
#36367 = CARTESIAN_POINT ( 'NONE',  ( -1.198202975868765119, 3.267716535433071279, -1.732283464566922726 ) ) ;
#36368 = CARTESIAN_POINT ( 'NONE',  ( 0.2727639067037610499, 3.346456692913386100, 1.732283464566921172 ) ) ;
#36369 = EDGE_CURVE ( 'NONE', #40420, #47614, #29819, .T. ) ;
#36370 = DIRECTION ( 'NONE',  ( -0.9998717552508122886, -0.01601477604151181275, 0.000000000000000000 ) ) ;
#36371 = DIRECTION ( 'NONE',  ( 0.9639628606958549062, 0.000000000000000000, -0.2660368455666687892 ) ) ;
#36372 = VECTOR ( 'NONE', #29120, 39.37007874015748143 ) ;
#36373 = VECTOR ( 'NONE', #29215, 39.37007874015748143 ) ;
#36374 = CARTESIAN_POINT ( 'NONE',  ( 0.000000000000000000, 3.346456692913386100, 0.000000000000000000 ) ) ;
#36375 = ORIENTED_EDGE ( 'NONE', *, *, #46822, .T. ) ;
#36376 = CARTESIAN_POINT ( 'NONE',  ( 0.7423782071083085965, 3.267716535433071279, -1.141732283464564013 ) ) ;
#36377 = VERTEX_POINT ( 'NONE', #25688 ) ;
#36378 = FACE_OUTER_BOUND ( 'NONE', #10571, .T. ) ;
#36379 = VECTOR ( 'NONE', #2620, 39.37007874015748143 ) ;
#36380 = ORIENTED_EDGE ( 'NONE', *, *, #27564, .F. ) ;
#36381 = ADVANCED_FACE ( 'NONE', ( #38336 ), #41441, .F. ) ;
#36382 = CARTESIAN_POINT ( 'NONE',  ( -1.091055626815042645, 0.000000000000000000, -0.6299212598425177889 ) ) ;
#36383 = LINE ( 'NONE', #5136, #13854 ) ;
#36384 = DIRECTION ( 'NONE',  ( 1.734723475976806848E-16, -0.000000000000000000, 1.000000000000000000 ) ) ;
#36385 = SHAPE_REPRESENTATION ( 'Stator', ( #26741 ), #13567 ) ;
#36386 = LINE ( 'NONE', #4629, #27700 ) ;
#36387 = EDGE_LOOP ( 'NONE', ( #22467, #4318, #2572, #19123 ) ) ;
#36388 = CARTESIAN_POINT ( 'NONE',  ( 1.775400203342704986, 1.648464234653929106, -2.359903268218703332 ) ) ;
#36389 = B_SPLINE_CURVE_WITH_KNOTS ( 'NONE', 3,
 ( #16180, #8940, #40190, #939 ),
 .UNSPECIFIED., .F., .F.,
 ( 4, 4 ),
 ( 0.01369329263415524495, 0.03074394281915088928 ),
 .UNSPECIFIED. ) ;
#36390 = FACE_BOUND ( 'NONE', #7756, .T. ) ;
#36391 = ORIENTED_EDGE ( 'NONE', *, *, #40257, .F. ) ;
#36392 = CARTESIAN_POINT ( 'NONE',  ( 1.560669927219590747, 3.346456692913386100, -0.4724409448818889246 ) ) ;
#36393 = ORIENTED_EDGE ( 'NONE', *, *, #22295, .T. ) ;
#36394 = LINE ( 'NONE', #5664, #31801 ) ;
#36395 = LINE ( 'NONE', #4642, #35491 ) ;
#36396 = LINE ( 'NONE', #8771, #28838 ) ;
#36397 = ORIENTED_EDGE ( 'NONE', *, *, #46467, .T. ) ;
#36399 = EDGE_CURVE ( 'NONE', #2009, #29934, #25945, .T. ) ;
#36398 = VERTEX_POINT ( 'NONE', #34209 ) ;
#36400 = FACE_OUTER_BOUND ( 'NONE', #3142, .T. ) ;
#36401 = CARTESIAN_POINT ( 'NONE',  ( 2.150824344285287459, 1.742351338968239238, -0.8657870173518766865 ) ) ;
#36402 = FACE_BOUND ( 'NONE', #39225, .T. ) ;
#36403 = EDGE_CURVE ( 'NONE', #22175, #13982, #2703, .T. ) ;
#36404 = CIRCLE ( 'NONE', #10823, 2.165354330708661568 ) ;
#36405 = AXIS2_PLACEMENT_3D ( 'NONE', #36031, #1420, #24667 ) ;
#36406 = CARTESIAN_POINT ( 'NONE',  ( 2.793030215715258446, 5.118110236220475784, 0.9592557174602684977 ) ) ;
#36407 = FACE_OUTER_BOUND ( 'NONE', #33321, .T. ) ;
#36408 = EDGE_CURVE ( 'NONE', #14441, #41776, #5816, .T. ) ;
#36409 = ADVANCED_FACE ( 'NONE', ( #14071 ), #49895, .F. ) ;
#36410 = ORIENTED_EDGE ( 'NONE', *, *, #26403, .F. ) ;
#36411 = CARTESIAN_POINT ( 'NONE',  ( -2.576863348864732117, 1.580667355030889620, 1.442554885838411849 ) ) ;
#36412 = VECTOR ( 'NONE', #23620, 39.37007874015748143 ) ;
#36413 = EDGE_LOOP ( 'NONE', ( #6260, #4502, #6285, #24801 ) ) ;
#36414 = ORIENTED_EDGE ( 'NONE', *, *, #11461, .F. ) ;
#36415 = VECTOR ( 'NONE', #46897, 39.37007874015748143 ) ;
#36416 = ORIENTED_EDGE ( 'NONE', *, *, #617, .T. ) ;
#36417 = DIRECTION ( 'NONE',  ( 0.3513748240813304724, 0.000000000000000000, 0.9362348706397417564 ) ) ;
#36418 = AXIS2_PLACEMENT_3D ( 'NONE', #30536, #42647, #38039 ) ;
#36419 = CARTESIAN_POINT ( 'NONE',  ( 0.000000000000000000, 3.267716535433071279, 0.000000000000000000 ) ) ;
#36420 = EDGE_CURVE ( 'NONE', #49288, #46953, #9947, .T. ) ;
#36421 = CARTESIAN_POINT ( 'NONE',  ( 0.07982360342473591996, 1.709180471932028711, 0.000000000000000000 ) ) ;
#36422 = DIRECTION ( 'NONE',  ( -0.8805955318567321166, 5.503865196449042635E-17, -0.4738686624730094055 ) ) ;
#36423 = ORIENTED_EDGE ( 'NONE', *, *, #11354, .T. ) ;
#36424 = ORIENTED_EDGE ( 'NONE', *, *, #35879, .T. ) ;
#36425 = LINE ( 'NONE', #40554, #28257 ) ;
#36426 = FACE_OUTER_BOUND ( 'NONE', #59, .T. ) ;
#36427 = PLANE ( 'NONE',  #15876 ) ;
#36428 = EDGE_CURVE ( 'NONE', #20741, #34340, #45039, .T. ) ;
#36429 = DIRECTION ( 'NONE',  ( 1.000000000000000000, 0.000000000000000000, -3.469446951953613696E-16 ) ) ;
#36430 = LINE ( 'NONE', #5181, #45408 ) ;
#36431 = B_SPLINE_CURVE_WITH_KNOTS ( 'NONE', 3,
 ( #22983, #27345, #43599, #19096 ),
 .UNSPECIFIED., .F., .F.,
 ( 4, 4 ),
 ( 0.1211775127643062999, 0.1625894504277921315 ),
 .UNSPECIFIED. ) ;
#36432 = DIRECTION ( 'NONE',  ( 1.000000000000000000, 0.000000000000000000, 0.000000000000000000 ) ) ;
#36433 = ADVANCED_FACE ( 'NONE', ( #26197 ), #33956, .F. ) ;
#36434 = DIRECTION ( 'NONE',  ( -1.000000000000000000, 0.000000000000000000, -0.000000000000000000 ) ) ;
#36435 = CARTESIAN_POINT ( 'NONE',  ( 0.000000000000000000, 3.267716535433071279, 0.000000000000000000 ) ) ;
#36436 = ORIENTED_EDGE ( 'NONE', *, *, #38847, .T. ) ;
#36437 = DIRECTION ( 'NONE',  ( -0.000000000000000000, 1.000000000000000000, -0.000000000000000000 ) ) ;
#36438 = DIRECTION ( 'NONE',  ( 4.336808689942019585E-17, 5.168407336632174847E-17, 1.000000000000000000 ) ) ;
#36439 = EDGE_LOOP ( 'NONE', ( #20678, #15951, #30561, #23234, #45950, #17407 ) ) ;
#36440 = ADVANCED_FACE ( 'NONE', ( #41695 ), #29308, .F. ) ;
#36441 = VERTEX_POINT ( 'NONE', #6330 ) ;
#36442 = DIRECTION ( 'NONE',  ( -1.000000000000000000, 0.000000000000000000, 0.000000000000000000 ) ) ;
#36443 = AXIS2_PLACEMENT_3D ( 'NONE', #5483, #21234, #36988 ) ;
#36444 = PLANE ( 'NONE',  #38543 ) ;
#36445 = CARTESIAN_POINT ( 'NONE',  ( 1.984304711592181691, 1.049866565877818125, -0.4024264095323374368 ) ) ;
#36446 = ORIENTED_EDGE ( 'NONE', *, *, #2788, .T. ) ;
#36447 = AXIS2_PLACEMENT_3D ( 'NONE', #7060, #50365, #7313 ) ;
#36448 = EDGE_CURVE ( 'NONE', #44346, #15612, #14324, .T. ) ;
#36449 = ORIENTED_EDGE ( 'NONE', *, *, #38743, .F. ) ;
#36450 = CARTESIAN_POINT ( 'NONE',  ( -1.091055626815042645, 0.000000000000000000, -7.512581982576723358E-16 ) ) ;
#36451 = VECTOR ( 'NONE', #3767, 39.37007874015748854 ) ;
#36452 = ORIENTED_EDGE ( 'NONE', *, *, #32699, .F. ) ;
#36453 = ORIENTED_EDGE ( 'NONE', *, *, #16002, .T. ) ;
#36454 = EDGE_CURVE ( 'NONE', #3395, #16985, #6531, .T. ) ;
#36455 = AXIS2_PLACEMENT_3D ( 'NONE', #23157, #11296, #50724 ) ;
#36456 = PLANE ( 'NONE',  #43314 ) ;
#36457 = LINE ( 'NONE', #13218, #17331 ) ;
#36458 = DIRECTION ( 'NONE',  ( -0.000000000000000000, 0.000000000000000000, 1.000000000000000000 ) ) ;
#36459 = ORIENTED_EDGE ( 'NONE', *, *, #7780, .T. ) ;
#36460 = VERTEX_POINT ( 'NONE', #17948 ) ;
#36461 = ORIENTED_EDGE ( 'NONE', *, *, #47745, .F. ) ;
#36462 = CARTESIAN_POINT ( 'NONE',  ( -1.738885967245169306, 1.688171000478772887, 2.065113283993135429 ) ) ;
#36463 = ORIENTED_EDGE ( 'NONE', *, *, #24850, .F. ) ;
#36464 = EDGE_LOOP ( 'NONE', ( #10130, #32692, #24330, #31935 ) ) ;
#36465 = CARTESIAN_POINT ( 'NONE',  ( -1.105178190331685961, 1.205361022782829114E-17, -1.437421806808603542 ) ) ;
#36466 = DIRECTION ( 'NONE',  ( -2.891205793294678326E-16, 0.000000000000000000, 1.000000000000000000 ) ) ;
#36467 = DIRECTION ( 'NONE',  ( -0.9909497617679331460, 0.000000000000000000, -0.1342332658176667026 ) ) ;
#36468 = EDGE_CURVE ( 'NONE', #11950, #14008, #22078, .T. ) ;
#36469 = ORIENTED_EDGE ( 'NONE', *, *, #30395, .T. ) ;
#36470 = FACE_OUTER_BOUND ( 'NONE', #20180, .T. ) ;
#36471 = CARTESIAN_POINT ( 'NONE',  ( -2.160407304981126320, 1.574879494900809584, -0.1462862061266896330 ) ) ;
#36472 = CARTESIAN_POINT ( 'NONE',  ( 1.287906020515829919, 0.000000000000000000, -1.889763779527552368 ) ) ;
#36473 = EDGE_CURVE ( 'NONE', #4073, #33562, #37838, .T. ) ;
#36474 = EDGE_LOOP ( 'NONE', ( #32512, #14942, #9374, #47864, #3230, #43553, #43419, #45344, #15137, #27172, #24008 ) ) ;
#36475 = DIRECTION ( 'NONE',  ( -0.000000000000000000, 1.000000000000000000, -0.000000000000000000 ) ) ;
#36476 = LINE ( 'NONE', #33125, #29372 ) ;
#36477 = CARTESIAN_POINT ( 'NONE',  ( -1.909347346926324462, 3.346456692913386100, 0.4724409448818871482 ) ) ;
#36478 = ORIENTED_EDGE ( 'NONE', *, *, #1265, .T. ) ;
#36479 = EDGE_LOOP ( 'NONE', ( #29565, #32364, #30541, #35778 ) ) ;
#36480 = DIRECTION ( 'NONE',  ( -0.000000000000000000, 1.000000000000000000, -0.000000000000000000 ) ) ;
#36481 = CARTESIAN_POINT ( 'NONE',  ( -0.9971138720282235468, 1.601380608780962778, 2.516743141396816430 ) ) ;
#36483 = VECTOR ( 'NONE', #23438, 39.37007874015748143 ) ;
#36482 = DIRECTION ( 'NONE',  ( -1.000000000000000000, 0.000000000000000000, 1.734723475976806848E-16 ) ) ;
#36484 = CARTESIAN_POINT ( 'NONE',  ( -0.3486774197067339376, 3.267716535433071279, 1.209717811016579078E-16 ) ) ;
#36485 = CARTESIAN_POINT ( 'NONE',  ( 0.000000000000000000, 3.267716535433071279, -0.8267716535433052849 ) ) ;
#36486 = ORIENTED_EDGE ( 'NONE', *, *, #10047, .F. ) ;
#36487 = ORIENTED_EDGE ( 'NONE', *, *, #4062, .T. ) ;
#36488 = AXIS2_PLACEMENT_3D ( 'NONE', #8399, #23890, #43746 ) ;
#36489 = CARTESIAN_POINT ( 'NONE',  ( 2.193564619503452828, 1.644610705845120258, 0.7644775380370429918 ) ) ;
#36490 = AXIS2_PLACEMENT_3D ( 'NONE', #7333, #19938, #19436 ) ;
#36491 = VERTEX_POINT ( 'NONE', #38084 ) ;
#36492 = CARTESIAN_POINT ( 'NONE',  ( 0.000000000000000000, 0.000000000000000000, 0.000000000000000000 ) ) ;
#36493 = LINE ( 'NONE', #47805, #2026 ) ;
#36494 = VECTOR ( 'NONE', #49077, 39.37007874015748143 ) ;
#36495 = VECTOR ( 'NONE', #2078, 39.37007874015748143 ) ;
#36496 = EDGE_CURVE ( 'NONE', #12681, #28527, #44428, .T. ) ;
#36497 = CARTESIAN_POINT ( 'NONE',  ( 2.437180031585944207, 1.757239404341893518, -1.667735833703099191 ) ) ;
#36498 = FACE_OUTER_BOUND ( 'NONE', #27256, .T. ) ;
#36499 = CARTESIAN_POINT ( 'NONE',  ( 3.927031490892378253E-16, 3.346456692913386100, 1.062992125984246083 ) ) ;
#36500 = ORIENTED_EDGE ( 'NONE', *, *, #32965, .T. ) ;
#36501 = PLANE ( 'NONE',  #11023 ) ;
#36502 = CARTESIAN_POINT ( 'NONE',  ( -1.743145509346916588, 0.000000000000000000, 0.000000000000000000 ) ) ;
#36503 = EDGE_CURVE ( 'NONE', #47345, #10658, #8091, .T. ) ;
#36504 = ORIENTED_EDGE ( 'NONE', *, *, #6118, .T. ) ;
#36505 = CARTESIAN_POINT ( 'NONE',  ( -0.07591351300297294324, 3.267716535433071279, 2.633779063002555273E-17 ) ) ;
#36506 = ADVANCED_FACE ( 'NONE', ( #22835 ), #42936, .F. ) ;
#36507 = CARTESIAN_POINT ( 'NONE',  ( -1.064142702668968932, 0.000000000000000000, -1.380941303491921346 ) ) ;
#36508 = CARTESIAN_POINT ( 'NONE',  ( 1.833433833923351353, 3.267716535433071279, -0.3149606299212596716 ) ) ;
#36510 = EDGE_CURVE ( 'NONE', #14009, #8562, #42443, .T. ) ;
#36509 = ORIENTED_EDGE ( 'NONE', *, *, #31370, .T. ) ;
#36511 = DIRECTION ( 'NONE',  ( -0.8660254037844362651, 0.000000000000000000, 0.5000000000000041078 ) ) ;
#36512 = CARTESIAN_POINT ( 'NONE',  ( 0.2727639067037602172, 3.346456692913386100, -1.732283464566922726 ) ) ;
#36513 = CARTESIAN_POINT ( 'NONE',  ( -1.010509689441836390, 0.01173450346422093109, -1.474572740271697047 ) ) ;
#36514 = ORIENTED_EDGE ( 'NONE', *, *, #28750, .T. ) ;
#36515 = CARTESIAN_POINT ( 'NONE',  ( 1.333043869570198714, 0.03249744100148316966, 1.450993329683806676 ) ) ;
#36516 = CARTESIAN_POINT ( 'NONE',  ( 1.560669927219590525, 3.267716535433071279, -5.414661521997676285E-16 ) ) ;
#36517 = VERTEX_POINT ( 'NONE', #19949 ) ;
#36518 = DIRECTION ( 'NONE',  ( 0.000000000000000000, 0.000000000000000000, -1.000000000000000000 ) ) ;
#36519 = CARTESIAN_POINT ( 'NONE',  ( 1.091055626815042423, 3.346456692913386100, -1.889763779527552368 ) ) ;
#36520 = CARTESIAN_POINT ( 'NONE',  ( 0.7423782071083084855, 3.267716535433071279, -1.574803149606293529 ) ) ;
#36521 = CARTESIAN_POINT ( 'NONE',  ( 0.5455278134075211005, 0.000000000000000000, -0.8267716535433055070 ) ) ;
#36522 = EDGE_CURVE ( 'NONE', #26498, #48342, #41978, .T. ) ;
#36523 = DIRECTION ( 'NONE',  ( -0.000000000000000000, 1.000000000000000000, -0.000000000000000000 ) ) ;
#36524 = AXIS2_PLACEMENT_3D ( 'NONE', #1417, #29029, #44768 ) ;
#36525 = VERTEX_POINT ( 'NONE', #35715 ) ;
#36526 = VERTEX_POINT ( 'NONE', #11213 ) ;
#36527 = CARTESIAN_POINT ( 'NONE',  ( 0.000000000000000000, 3.267716535433071279, 1.259842519685033135 ) ) ;
#36528 = DIRECTION ( 'NONE',  ( 0.000000000000000000, 0.000000000000000000, -1.000000000000000000 ) ) ;
#36529 = ORIENTED_EDGE ( 'NONE', *, *, #50437, .F. ) ;
#36530 = PLANE ( 'NONE',  #45634 ) ;
#36531 = LINE ( 'NONE', #385, #50710 ) ;
#36532 = DIRECTION ( 'NONE',  ( -0.01601477604151182663, 0.9998717552508123996, -0.000000000000000000 ) ) ;
#36533 = VECTOR ( 'NONE', #49269, 39.37007874015748143 ) ;
#36534 = EDGE_CURVE ( 'NONE', #46444, #47197, #15087, .T. ) ;
#36535 = DIRECTION ( 'NONE',  ( -0.000000000000000000, 1.000000000000000000, -0.000000000000000000 ) ) ;
#36536 = AXIS2_PLACEMENT_3D ( 'NONE', #32304, #24545, #44916 ) ;
#36537 = VERTEX_POINT ( 'NONE', #7837 ) ;
#36538 = VERTEX_POINT ( 'NONE', #11962 ) ;
#36539 = DIRECTION ( 'NONE',  ( -1.000000000000000000, 0.000000000000000000, 0.000000000000000000 ) ) ;
#36540 = DIRECTION ( 'NONE',  ( -1.000000000000000000, 0.000000000000000000, 0.000000000000000000 ) ) ;
#36541 = CARTESIAN_POINT ( 'NONE',  ( -0.04921259842519689481, 0.009044826170997494544, 1.897191039754219988 ) ) ;
#36542 = EDGE_CURVE ( 'NONE', #40300, #5052, #15335, .T. ) ;
#36543 = VERTEX_POINT ( 'NONE', #31341 ) ;
#36544 = CARTESIAN_POINT ( 'NONE',  ( 1.636583440222563635, 3.267716535433071279, -1.141732283464564013 ) ) ;
#36545 = FACE_BOUND ( 'NONE', #32606, .T. ) ;
#36546 = VECTOR ( 'NONE', #28546, 39.37007874015748143 ) ;
#36547 = VERTEX_POINT ( 'NONE', #50391 ) ;
#36548 = CARTESIAN_POINT ( 'NONE',  ( 0.000000000000000000, 3.267716535433071279, 0.4724409448818872592 ) ) ;
#36549 = ORIENTED_EDGE ( 'NONE', *, *, #19319, .T. ) ;
#36550 = EDGE_LOOP ( 'NONE', ( #42807, #41746, #42502, #44335 ) ) ;
#36551 = CARTESIAN_POINT ( 'NONE',  ( -0.5455278134075214336, 3.346456692913386100, 2.034427629037600660 ) ) ;
#36552 = ORIENTED_EDGE ( 'NONE', *, *, #27629, .F. ) ;
#36553 = VERTEX_POINT ( 'NONE', #26945 ) ;
#36554 = CARTESIAN_POINT ( 'NONE',  ( 0.07982360342473591996, 1.709180471932028711, 0.000000000000000000 ) ) ;
#36555 = VERTEX_POINT ( 'NONE', #23838 ) ;
#36556 = DIRECTION ( 'NONE',  ( -0.000000000000000000, 1.000000000000000000, -0.000000000000000000 ) ) ;
#36557 = CARTESIAN_POINT ( 'NONE',  ( 0.7697289541298216742, 1.632794381801279116, -2.850711116225059794 ) ) ;
#36558 = CARTESIAN_POINT ( 'NONE',  ( 2.138597145901430352, 6.692913385826772199, 0.3393547186367261159 ) ) ;
#36559 = CARTESIAN_POINT ( 'NONE',  ( 2.823445274216730638, 1.664781993127344872, 0.8656477926280681245 ) ) ;
#36560 = AXIS2_PLACEMENT_3D ( 'NONE', #3127, #18881, #43873 ) ;
#36561 = DIRECTION ( 'NONE',  ( -0.9839295885986295565, 2.076492729081308301E-17, -0.1785568947986370392 ) ) ;
#36562 = LINE ( 'NONE', #20021, #30343 ) ;
#36563 = ORIENTED_EDGE ( 'NONE', *, *, #20107, .F. ) ;
#36564 = DIRECTION ( 'NONE',  ( -1.000000000000000000, 0.000000000000000000, 0.000000000000000000 ) ) ;
#36565 = VECTOR ( 'NONE', #42717, 39.37007874015748143 ) ;
#36566 = LINE ( 'NONE', #5066, #33101 ) ;
#36567 = AXIS2_PLACEMENT_3D ( 'NONE', #47072, #11749, #7877 ) ;
#36568 = VECTOR ( 'NONE', #50335, 39.37007874015748143 ) ;
#36569 = EDGE_LOOP ( 'NONE', ( #8665, #24075, #36978, #39593 ) ) ;
#36570 = DIRECTION ( 'NONE',  ( -0.000000000000000000, 1.000000000000000000, -0.000000000000000000 ) ) ;
#36571 = ADVANCED_FACE ( 'NONE', ( #15589 ), #18955, .F. ) ;
#36572 = DIRECTION ( 'NONE',  ( -1.000000000000000000, -0.000000000000000000, -0.000000000000000000 ) ) ;
#36573 = ORIENTED_EDGE ( 'NONE', *, *, #2535, .F. ) ;
#36574 = DIRECTION ( 'NONE',  ( 0.000000000000000000, -1.000000000000000000, 0.000000000000000000 ) ) ;
#36575 = EDGE_CURVE ( 'NONE', #26074, #27975, #27449, .T. ) ;
#36576 = DIRECTION ( 'NONE',  ( -0.3090169943749447312, 0.000000000000000000, -0.9510565162951544194 ) ) ;
#36577 = EDGE_CURVE ( 'NONE', #1678, #24825, #49176, .T. ) ;
#36578 = CARTESIAN_POINT ( 'NONE',  ( -1.363819533518803473, 3.346456692913386100, -0.3543307086614174151 ) ) ;
#36579 = VECTOR ( 'NONE', #44484, 39.37007874015748143 ) ;
#36580 = ORIENTED_EDGE ( 'NONE', *, *, #27647, .F. ) ;
#36581 = DIRECTION ( 'NONE',  ( 0.000000000000000000, 0.000000000000000000, -1.000000000000000000 ) ) ;
#36582 = ORIENTED_EDGE ( 'NONE', *, *, #30629, .T. ) ;
#36583 = FACE_BOUND ( 'NONE', #27043, .T. ) ;
#36584 = CARTESIAN_POINT ( 'NONE',  ( 0.3303541855028670482, 0.3937007874015748254, -0.7480314960629920185 ) ) ;
#36585 = EDGE_CURVE ( 'NONE', #35962, #15224, #43188, .T. ) ;
#36586 = CARTESIAN_POINT ( 'NONE',  ( 0.000000000000000000, 3.267716535433071279, -0.7874015748031470974 ) ) ;
#36587 = CARTESIAN_POINT ( 'NONE',  ( 2.059921668671832240, 5.905511811023623991, 0.7210543110491621777 ) ) ;
#36588 = ORIENTED_EDGE ( 'NONE', *, *, #46550, .T. ) ;
#36589 = VERTEX_POINT ( 'NONE', #4215 ) ;
#36590 = CARTESIAN_POINT ( 'NONE',  ( -1.088226697794229869, 1.657663611856292185, 1.917334528692921758 ) ) ;
#36591 = VERTEX_POINT ( 'NONE', #30580 ) ;
#36592 = EDGE_CURVE ( 'NONE', #33511, #10224, #23083, .T. ) ;
#36593 = CARTESIAN_POINT ( 'NONE',  ( 0.08119777152254364916, 1.623385212329073957, 0.000000000000000000 ) ) ;
#36594 = VERTEX_POINT ( 'NONE', #3460 ) ;
#36595 = DIRECTION ( 'NONE',  ( 0.01601477604151182663, -0.9998717552508123996, 0.000000000000000000 ) ) ;
#36596 = EDGE_CURVE ( 'NONE', #18552, #25411, #34961, .T. ) ;
#36597 = ORIENTED_EDGE ( 'NONE', *, *, #44732, .F. ) ;
#36598 = CARTESIAN_POINT ( 'NONE',  ( 0.000000000000000000, 3.346456692913386100, 0.000000000000000000 ) ) ;
#36599 = ADVANCED_FACE ( 'NONE', ( #39079 ), #18062, .T. ) ;
#36600 = AXIS2_PLACEMENT_3D ( 'NONE', #13058, #23898, #32949 ) ;
#36601 = CARTESIAN_POINT ( 'NONE',  ( 1.232995795418176055, 1.205361022782829114E-17, 1.780798594093568221 ) ) ;
#36602 = ORIENTED_EDGE ( 'NONE', *, *, #46960, .F. ) ;
#36603 = EDGE_CURVE ( 'NONE', #23957, #1644, #46789, .T. ) ;
#36604 = CARTESIAN_POINT ( 'NONE',  ( 0.000000000000000000, 6.692913385826772199, 0.000000000000000000 ) ) ;
#36605 = VECTOR ( 'NONE', #10283, 39.37007874015748143 ) ;
#36606 = VERTEX_POINT ( 'NONE', #35210 ) ;
#36607 = EDGE_CURVE ( 'NONE', #13403, #28656, #1363, .T. ) ;
#36608 = AXIS2_PLACEMENT_3D ( 'NONE', #5111, #47674, #12351 ) ;
#36609 = VECTOR ( 'NONE', #16240, 39.37007874015748143 ) ;
#36610 = ORIENTED_EDGE ( 'NONE', *, *, #4993, .F. ) ;
#36611 = VERTEX_POINT ( 'NONE', #44712 ) ;
#36612 = CARTESIAN_POINT ( 'NONE',  ( 0.000000000000000000, 3.267716535433071279, 0.000000000000000000 ) ) ;
#36613 = AXIS2_PLACEMENT_3D ( 'NONE', #36955, #48516, #9320 ) ;
#36614 = VERTEX_POINT ( 'NONE', #27960 ) ;
#36615 = CARTESIAN_POINT ( 'NONE',  ( -0.8942052331142552601, 3.346456692913386100, -0.9448818897637760728 ) ) ;
#36616 = EDGE_LOOP ( 'NONE', ( #20211, #5471, #40586, #38771 ) ) ;
#36617 = DIRECTION ( 'NONE',  ( 1.000000000000000000, -0.000000000000000000, 0.000000000000000000 ) ) ;
#36618 = LINE ( 'NONE', #8226, #28030 ) ;
#36619 = ORIENTED_EDGE ( 'NONE', *, *, #40489, .F. ) ;
#36620 = DIRECTION ( 'NONE',  ( -0.6579387259397027066, 8.743779800425989470E-17, -0.7530714660036196273 ) ) ;
#36621 = CARTESIAN_POINT ( 'NONE',  ( -0.3486774197067334935, 0.000000000000000000, 0.7480314960629874665 ) ) ;
#36622 = CARTESIAN_POINT ( 'NONE',  ( -0.2727639067037602727, 3.346456692913386100, 0.9055118110236167750 ) ) ;
#36623 = DIRECTION ( 'NONE',  ( 1.000000000000000000, 0.000000000000000000, 0.000000000000000000 ) ) ;
#36624 = CARTESIAN_POINT ( 'NONE',  ( 0.07982360342473591996, 1.709180471932028711, 0.000000000000000000 ) ) ;
#36625 = CARTESIAN_POINT ( 'NONE',  ( -2.101347671104863313, 1.674245022174266406, -0.5300970854448181502 ) ) ;
#36626 = LINE ( 'NONE', #7976, #44936 ) ;
#36627 = ORIENTED_EDGE ( 'NONE', *, *, #33276, .F. ) ;
#36628 = DIRECTION ( 'NONE',  ( -0.9998717552508121775, -0.01601477604151182316, 0.000000000000000000 ) ) ;
#36629 = CARTESIAN_POINT ( 'NONE',  ( 0.000000000000000000, 3.346456692913386100, 0.000000000000000000 ) ) ;
#36630 = PRODUCT_DEFINITION_FORMATION_WITH_SPECIFIED_SOURCE ( 'ANY', '', #50723, .NOT_KNOWN. ) ;
#36631 = EDGE_CURVE ( 'NONE', #49445, #12012, #43695, .T. ) ;
#36632 = ORIENTED_EDGE ( 'NONE', *, *, #6288, .F. ) ;
#36633 = CARTESIAN_POINT ( 'NONE',  ( -0.8515791614234526907, 0.000000000000000000, 1.521253268579204398 ) ) ;
#36634 = VECTOR ( 'NONE', #7518, 39.37007874015748143 ) ;
#36635 = EDGE_CURVE ( 'NONE', #26202, #50880, #4984, .T. ) ;
#36636 = VECTOR ( 'NONE', #5500, 39.37007874015748143 ) ;
#36637 = ORIENTED_EDGE ( 'NONE', *, *, #224, .T. ) ;
#36638 = CARTESIAN_POINT ( 'NONE',  ( 0.000000000000000000, 2.755905511811023612, 0.000000000000000000 ) ) ;
#36639 = EDGE_CURVE ( 'NONE', #187, #32403, #36233, .T. ) ;
#36640 = AXIS2_PLACEMENT_3D ( 'NONE', #37281, #33417, #13781 ) ;
#36642 = CIRCLE ( 'NONE', #2844, 2.244934639244525076 ) ;
#36641 = DIRECTION ( 'NONE',  ( 1.734723475976806848E-16, 0.000000000000000000, 1.000000000000000000 ) ) ;
#36643 = CARTESIAN_POINT ( 'NONE',  ( 1.833433833923351353, 3.267716535433071279, -1.161035397307311917E-15 ) ) ;
#36644 = DIRECTION ( 'NONE',  ( 1.000000000000000000, 0.000000000000000000, 0.000000000000000000 ) ) ;
#36645 = CARTESIAN_POINT ( 'NONE',  ( 1.833433833923351353, 3.267716535433071279, -1.036830145017913596 ) ) ;
#36646 = ORIENTED_EDGE ( 'NONE', *, *, #18071, .T. ) ;
#36647 = LINE ( 'NONE', #1269, #4342 ) ;
#36648 = VECTOR ( 'NONE', #20366, 39.37007874015748143 ) ;
#36649 = FACE_OUTER_BOUND ( 'NONE', #39509, .T. ) ;
#36650 = ORIENTED_EDGE ( 'NONE', *, *, #48426, .T. ) ;
#36651 = LINE ( 'NONE', #9532, #47675 ) ;
#36652 = ORIENTED_EDGE ( 'NONE', *, *, #45684, .F. ) ;
#36653 = CARTESIAN_POINT ( 'NONE',  ( -1.091055626815042645, 3.346456692913386100, -0.3149606299212593941 ) ) ;
#36654 = DIRECTION ( 'NONE',  ( 1.734723475976806848E-16, -0.000000000000000000, 1.000000000000000000 ) ) ;
#36655 = EDGE_CURVE ( 'NONE', #47504, #1038, #32111, .T. ) ;
#36656 = FACE_OUTER_BOUND ( 'NONE', #7115, .T. ) ;
#36657 = ADVANCED_FACE ( 'NONE', ( #16869 ), #39842, .F. ) ;
#36658 = EDGE_LOOP ( 'NONE', ( #10226, #16997, #39800, #46152 ) ) ;
#36659 = ORIENTED_EDGE ( 'NONE', *, *, #4619, .F. ) ;
#36660 = EDGE_CURVE ( 'NONE', #22006, #21605, #25116, .T. ) ;
#36661 = DIRECTION ( 'NONE',  ( -3.469446951953613696E-16, 0.000000000000000000, -1.000000000000000000 ) ) ;
#36662 = DIRECTION ( 'NONE',  ( -0.000000000000000000, 1.000000000000000000, -0.000000000000000000 ) ) ;
#36663 = CARTESIAN_POINT ( 'NONE',  ( 0.5455278134075217666, 0.000000000000000000, 1.259842519685033357 ) ) ;
#36664 = ORIENTED_EDGE ( 'NONE', *, *, #7895, .T. ) ;
#36665 = LINE ( 'NONE', #47465, #17136 ) ;
#36666 = CARTESIAN_POINT ( 'NONE',  ( 0.4161812636739331550, 0.000000000000000000, -1.692983086477933830 ) ) ;
#36667 = ORIENTED_EDGE ( 'NONE', *, *, #42530, .F. ) ;
#36668 = LINE ( 'NONE', #8782, #46356 ) ;
#36669 = VECTOR ( 'NONE', #22272, 39.37007874015748143 ) ;
#36670 = DIRECTION ( 'NONE',  ( 0.000000000000000000, 0.000000000000000000, 1.000000000000000000 ) ) ;
#36671 = ORIENTED_EDGE ( 'NONE', *, *, #26693, .T. ) ;
#36672 = VECTOR ( 'NONE', #2133, 39.37007874015748143 ) ;
#36673 = ORIENTED_EDGE ( 'NONE', *, *, #43425, .T. ) ;
#36674 = VECTOR ( 'NONE', #17779, 39.37007874015748143 ) ;
#36675 = VERTEX_POINT ( 'NONE', #40364 ) ;
#36676 = CARTESIAN_POINT ( 'NONE',  ( 0.7423782071083087075, 3.346456692913386100, 0.6299212598425161236 ) ) ;
#36677 = CONICAL_SURFACE ( 'NONE', #4413, 2.165354330708661568, 0.2617993877991570129 ) ;
#36678 = CARTESIAN_POINT ( 'NONE',  ( 2.164823134740036625, 5.118110236220475784, -0.04796011690015051371 ) ) ;
#36679 = DIRECTION ( 'NONE',  ( 0.000000000000000000, 0.000000000000000000, 1.000000000000000000 ) ) ;
#36680 = DIRECTION ( 'NONE',  ( 1.734723475976806848E-16, -0.000000000000000000, 1.000000000000000000 ) ) ;
#36681 = ORIENTED_EDGE ( 'NONE', *, *, #38802, .F. ) ;
#36682 = ORIENTED_EDGE ( 'NONE', *, *, #15115, .F. ) ;
#36683 = VECTOR ( 'NONE', #36844, 39.37007874015748143 ) ;
#36684 = DIRECTION ( 'NONE',  ( 0.9998717552508121775, 0.01601477604151182663, 0.000000000000000000 ) ) ;
#36685 = FILL_AREA_STYLE_COLOUR ( '', #19659 ) ;
#36686 = CARTESIAN_POINT ( 'NONE',  ( 0.000000000000000000, 0.000000000000000000, 0.000000000000000000 ) ) ;
#36687 = DIRECTION ( 'NONE',  ( -1.000000000000000000, -0.000000000000000000, -0.000000000000000000 ) ) ;
#36688 = DIRECTION ( 'NONE',  ( -0.000000000000000000, 1.000000000000000000, -0.000000000000000000 ) ) ;
#36689 = CARTESIAN_POINT ( 'NONE',  ( 0.6551740444401462637, 0.000000000000000000, 1.885762267972743711 ) ) ;
#36690 = PLANE ( 'NONE',  #11061 ) ;
#36691 = EDGE_CURVE ( 'NONE', #40889, #31073, #8990, .T. ) ;
#36692 = ORIENTED_EDGE ( 'NONE', *, *, #46326, .T. ) ;
#36693 = FACE_OUTER_BOUND ( 'NONE', #7721, .T. ) ;
#36694 = CARTESIAN_POINT ( 'NONE',  ( 0.000000000000000000, 3.267716535433071279, 1.574803149606291530 ) ) ;
#36695 = EDGE_CURVE ( 'NONE', #37948, #16316, #20862, .T. ) ;
#36696 = ORIENTED_EDGE ( 'NONE', *, *, #617, .F. ) ;
#36697 = EDGE_CURVE ( 'NONE', #40266, #16563, #40612, .T. ) ;
#36698 = EDGE_LOOP ( 'NONE', ( #45094, #2598, #24968, #34679, #46638, #10091, #26558, #31201, #9324, #22449, #26299, #45654, #40736 ) ) ;
#36699 = CARTESIAN_POINT ( 'NONE',  ( 2.274988110810610031, 1.744340048923221920, -0.4687729985174870495 ) ) ;
#36700 = DIRECTION ( 'NONE',  ( 1.000000000000000000, 0.000000000000000000, -3.469446951953613696E-16 ) ) ;
#36701 = ORIENTED_EDGE ( 'NONE', *, *, #8999, .T. ) ;
#36702 = EDGE_CURVE ( 'NONE', #20337, #10224, #8601, .T. ) ;
#36703 = AXIS2_PLACEMENT_3D ( 'NONE', #9313, #22216, #30716 ) ;
#36704 = CONICAL_SURFACE ( 'NONE', #14447, 3.033577403570480779, 1.554780866114618743 ) ;
#36705 = ORIENTED_EDGE ( 'NONE', *, *, #44830, .F. ) ;
#36706 = VECTOR ( 'NONE', #20617, 39.37007874015748143 ) ;
#36707 = CARTESIAN_POINT ( 'NONE',  ( -0.5455278134075208785, 3.267716535433071279, 1.574803149606291974 ) ) ;
#36708 = ORIENTED_EDGE ( 'NONE', *, *, #25284, .F. ) ;
#36709 = VECTOR ( 'NONE', #26972, 39.37007874015748143 ) ;
#36710 = ORIENTED_EDGE ( 'NONE', *, *, #12033, .T. ) ;
#36711 = CARTESIAN_POINT ( 'NONE',  ( 1.427293369312940152, 0.000000000000000000, -1.001115484471646111 ) ) ;
#36712 = CARTESIAN_POINT ( 'NONE',  ( -1.712496953225537633, 0.000000000000000000, 1.417322834645662333 ) ) ;
#36713 = ADVANCED_FACE ( 'NONE', ( #28975 ), #32619, .F. ) ;
#36714 = ORIENTED_EDGE ( 'NONE', *, *, #3228, .T. ) ;
#36715 = DIMENSIONAL_EXPONENTS ( 1.000000000000000000, 0.000000000000000000, 0.000000000000000000, 0.000000000000000000, 0.000000000000000000, 0.000000000000000000, 0.000000000000000000 ) ;
#36716 = VERTEX_POINT ( 'NONE', #48314 ) ;
#36717 = VERTEX_POINT ( 'NONE', #48058 ) ;
#36718 = VECTOR ( 'NONE', #15618, 39.37007874015748143 ) ;
#36719 = DIRECTION ( 'NONE',  ( 1.734723475976806848E-16, -0.000000000000000000, 1.000000000000000000 ) ) ;
#36720 = VERTEX_POINT ( 'NONE', #4475 ) ;
#36721 = VERTEX_POINT ( 'NONE', #35976 ) ;
#36722 = EDGE_CURVE ( 'NONE', #43398, #1008, #12731, .T. ) ;
#36723 = CARTESIAN_POINT ( 'NONE',  ( -0.2727639067037604392, 3.267716535433071279, 4.731699523581607892E-17 ) ) ;
#36724 = DIRECTION ( 'NONE',  ( 1.734723475976806848E-16, 0.000000000000000000, 1.000000000000000000 ) ) ;
#36725 = CARTESIAN_POINT ( 'NONE',  ( 2.422542647548854511, 1.750080673592185665, 0.7353866329521624445 ) ) ;
#36726 = VERTEX_POINT ( 'NONE', #12992 ) ;
#36727 = CARTESIAN_POINT ( 'NONE',  ( -0.04921259842519708910, 1.718497255264965551, 2.952755905511811108 ) ) ;
#36728 = DIRECTION ( 'NONE',  ( -0.000000000000000000, 1.000000000000000000, -0.000000000000000000 ) ) ;
#36729 = EDGE_CURVE ( 'NONE', #33278, #46567, #12469, .T. ) ;
#36730 = LINE ( 'NONE', #844, #7216 ) ;
#36731 = VERTEX_POINT ( 'NONE', #43952 ) ;
#36732 = CARTESIAN_POINT ( 'NONE',  ( 1.363819533518803695, 3.346456692913386100, 1.732283464566921172 ) ) ;
#36733 = CARTESIAN_POINT ( 'NONE',  ( 0.5455278134075211005, 3.346456692913386100, -1.141732283464564013 ) ) ;
#36734 = DIRECTION ( 'NONE',  ( 1.000000000000000000, 0.000000000000000000, -3.469446951953613696E-16 ) ) ;
#36735 = ORIENTED_EDGE ( 'NONE', *, *, #17510, .F. ) ;
#36736 = ORIENTED_EDGE ( 'NONE', *, *, #29260, .F. ) ;
#36737 = LINE ( 'NONE', #16347, #8094 ) ;
#36738 = EDGE_CURVE ( 'NONE', #23605, #40028, #9162, .T. ) ;
#36739 = CARTESIAN_POINT ( 'NONE',  ( 1.015142113812069313, 0.000000000000000000, -0.9842519685039348154 ) ) ;
#36740 = CARTESIAN_POINT ( 'NONE',  ( 1.091055626815042423, 3.267716535433071279, -2.086614173228339641 ) ) ;
#36741 = DIRECTION ( 'NONE',  ( -5.782411586589357392E-17, 0.000000000000000000, -1.000000000000000000 ) ) ;
#36742 = EDGE_LOOP ( 'NONE', ( #1736, #9434, #22938, #39525 ) ) ;
#36743 = ORIENTED_EDGE ( 'NONE', *, *, #9754, .T. ) ;
#36744 = VECTOR ( 'NONE', #15661, 39.37007874015748143 ) ;
#36745 = VECTOR ( 'NONE', #33735, 39.37007874015748143 ) ;
#36746 = CARTESIAN_POINT ( 'NONE',  ( 0.000000000000000000, 3.346456692913386100, 0.000000000000000000 ) ) ;
#36747 = ORIENTED_EDGE ( 'NONE', *, *, #1111, .T. ) ;
#36748 = DIRECTION ( 'NONE',  ( 0.1785568947986370392, 1.142009442734629415E-16, -0.9839295885986295565 ) ) ;
#36749 = CARTESIAN_POINT ( 'NONE',  ( 0.000000000000000000, 3.267716535433071279, 0.000000000000000000 ) ) ;
#36750 = VECTOR ( 'NONE', #11930, 39.37007874015748143 ) ;
#36751 = AXIS2_PLACEMENT_3D ( 'NONE', #13736, #42107, #29480 ) ;
#36752 = DIRECTION ( 'NONE',  ( 1.734723475976806848E-16, 0.000000000000000000, 1.000000000000000000 ) ) ;
#36753 = CARTESIAN_POINT ( 'NONE',  ( -0.2727639067037607723, 0.000000000000000000, -0.4724409448818883694 ) ) ;
#36754 = CARTESIAN_POINT ( 'NONE',  ( -1.636583440222563635, 3.346456692913386100, 0.9448818897637749625 ) ) ;
#36755 = VECTOR ( 'NONE', #47255, 39.37007874015748143 ) ;
#36756 = ORIENTED_EDGE ( 'NONE', *, *, #47852, .T. ) ;
#36757 = CARTESIAN_POINT ( 'NONE',  ( 4.268512490100411402E-16, 3.267716535433071279, 0.9448818897637749625 ) ) ;
#36758 = PLANE ( 'NONE',  #4260 ) ;
#36759 = EDGE_CURVE ( 'NONE', #28099, #3513, #24351, .T. ) ;
#36760 = ORIENTED_EDGE ( 'NONE', *, *, #50951, .T. ) ;
#36761 = DIRECTION ( 'NONE',  ( -1.000000000000000000, 0.000000000000000000, 0.000000000000000000 ) ) ;
#36762 = CARTESIAN_POINT ( 'NONE',  ( 1.636583440222563857, 0.000000000000000000, 1.574803149606291974 ) ) ;
#36763 = LINE ( 'NONE', #48077, #15592 ) ;
#36764 = ORIENTED_EDGE ( 'NONE', *, *, #30650, .T. ) ;
#36765 = CARTESIAN_POINT ( 'NONE',  ( -1.909347346926324462, 3.346456692913386100, 0.7874015748031456541 ) ) ;
#36766 = ADVANCED_FACE ( 'NONE', ( #28724 ), #48521, .T. ) ;
#36767 = FACE_OUTER_BOUND ( 'NONE', #47764, .T. ) ;
#36768 = EDGE_LOOP ( 'NONE', ( #4648, #43712, #23930, #5517 ) ) ;
#36769 = LINE ( 'NONE', #1902, #36234 ) ;
#36770 = CARTESIAN_POINT ( 'NONE',  ( 2.947574761915769059, 5.905511811023623991, -0.1816379373804906106 ) ) ;
#36771 = VERTEX_POINT ( 'NONE', #13499 ) ;
#36772 = DIRECTION ( 'NONE',  ( -1.000000000000000000, 0.000000000000000000, 1.734723475976806848E-16 ) ) ;
#36773 = CARTESIAN_POINT ( 'NONE',  ( -0.07591351300297333182, 0.000000000000000000, -1.102362204724405714 ) ) ;
#36774 = FACE_OUTER_BOUND ( 'NONE', #2065, .T. ) ;
#36775 = LINE ( 'NONE', #32143, #10331 ) ;
#36776 = DIRECTION ( 'NONE',  ( 1.000000000000000000, 0.000000000000000000, 0.000000000000000000 ) ) ;
#36777 = ORIENTED_EDGE ( 'NONE', *, *, #20193, .F. ) ;
#36778 = ORIENTED_EDGE ( 'NONE', *, *, #20656, .F. ) ;
#36779 = CARTESIAN_POINT ( 'NONE',  ( -1.636583440222564301, 3.346456692913386100, -1.325930245594398871 ) ) ;
#36780 = AXIS2_PLACEMENT_3D ( 'NONE', #45484, #16690, #37271 ) ;
#36781 = CARTESIAN_POINT ( 'NONE',  ( 0.7423782071083085965, 3.346456692913386100, -0.1968503937007880511 ) ) ;
#36782 = VECTOR ( 'NONE', #1238, 39.37007874015748143 ) ;
#36783 = EDGE_LOOP ( 'NONE', ( #10667, #39353, #47526, #45495 ) ) ;
#36784 = CARTESIAN_POINT ( 'NONE',  ( -1.091055626815042645, 3.346456692913386100, -1.771653543307081025 ) ) ;
#36785 = CARTESIAN_POINT ( 'NONE',  ( 0.7423782071083092626, 0.000000000000000000, 2.204724409448808764 ) ) ;
#36786 = CARTESIAN_POINT ( 'NONE',  ( -1.166969139818015977, 3.346456692913386100, -1.417322834645664109 ) ) ;
#36787 = VECTOR ( 'NONE', #15380, 39.37007874015748143 ) ;
#36788 = CARTESIAN_POINT ( 'NONE',  ( -1.711605288297850969, 0.0005051743623580321960, -0.3401845456954783464 ) ) ;
#36789 = ORIENTED_EDGE ( 'NONE', *, *, #325, .F. ) ;
#36790 = ORIENTED_EDGE ( 'NONE', *, *, #50163, .F. ) ;
#36791 = CARTESIAN_POINT ( 'NONE',  ( 0.1968503937007878568, 3.346456692913386100, 1.889763779527550369 ) ) ;
#36792 = CARTESIAN_POINT ( 'NONE',  ( -1.195183497228115035E-16, 3.346456692913386100, 0.6299212598425161236 ) ) ;
#36793 = VECTOR ( 'NONE', #12629, 39.37007874015748143 ) ;
#36794 = EDGE_CURVE ( 'NONE', #2180, #46194, #33892, .T. ) ;
#36795 = CARTESIAN_POINT ( 'NONE',  ( 1.909347346926324684, 0.000000000000000000, 0.2755905511810994302 ) ) ;
#36796 = VERTEX_POINT ( 'NONE', #17881 ) ;
#36797 = CARTESIAN_POINT ( 'NONE',  ( 0.5455278134075212115, 0.000000000000000000, -0.3149606299212593941 ) ) ;
#36799 = AXIS2_PLACEMENT_3D ( 'NONE', #31438, #15934, #4321 ) ;
#36798 = FACE_BOUND ( 'NONE', #45694, .T. ) ;
#36800 = ORIENTED_EDGE ( 'NONE', *, *, #7494, .T. ) ;
#36801 = LINE ( 'NONE', #5552, #23276 ) ;
#36802 = ORIENTED_EDGE ( 'NONE', *, *, #5822, .F. ) ;
#36803 = ORIENTED_EDGE ( 'NONE', *, *, #29423, .T. ) ;
#36804 = CARTESIAN_POINT ( 'NONE',  ( -1.636583440222563635, 0.000000000000000000, 0.6299212598425164567 ) ) ;
#36805 = EDGE_CURVE ( 'NONE', #27975, #9992, #10642, .T. ) ;
#36806 = B_SPLINE_CURVE_WITH_KNOTS ( 'NONE', 3,
 ( #50249, #6938, #31701, #47401 ),
 .UNSPECIFIED., .F., .F.,
 ( 4, 4 ),
 ( 0.1211873102087489551, 0.1625992483279400103 ),
 .UNSPECIFIED. ) ;
#36807 = EDGE_CURVE ( 'NONE', #11701, #18566, #21754, .T. ) ;
#36808 = ORIENTED_EDGE ( 'NONE', *, *, #3106, .F. ) ;
#36809 = CARTESIAN_POINT ( 'NONE',  ( 0.000000000000000000, 2.755905511811024056, 0.000000000000000000 ) ) ;
#36810 = ORIENTED_EDGE ( 'NONE', *, *, #42197, .F. ) ;
#36811 = EDGE_CURVE ( 'NONE', #40680, #25916, #9878, .T. ) ;
#36812 = LINE ( 'NONE', #42876, #16408 ) ;
#36813 = CARTESIAN_POINT ( 'NONE',  ( 0.8952071785065199849, 1.205361022782829114E-17, 1.972340328593147785 ) ) ;
#36814 = LINE ( 'NONE', #25189, #37458 ) ;
#36815 = ADVANCED_FACE ( 'NONE', ( #5750 ), #44969, .F. ) ;
#36816 = AXIS2_PLACEMENT_3D ( 'NONE', #47999, #15534, #24303 ) ;
#36817 = CARTESIAN_POINT ( 'NONE',  ( 1.135809427359538271, 0.01508310756785651019, -1.647033034181351052 ) ) ;
#36818 = CARTESIAN_POINT ( 'NONE',  ( 0.5455278134075216556, 0.000000000000000000, 1.692913385826762873 ) ) ;
#36819 = LINE ( 'NONE', #20288, #25363 ) ;
#36820 = AXIS2_PLACEMENT_3D ( 'NONE', #30723, #22972, #10344 ) ;
#36821 = ORIENTED_EDGE ( 'NONE', *, *, #47256, .F. ) ;
#36822 = FACE_OUTER_BOUND ( 'NONE', #12911, .T. ) ;
#36823 = AXIS2_PLACEMENT_3D ( 'NONE', #30584, #10711, #10457 ) ;
#36824 = AXIS2_PLACEMENT_3D ( 'NONE', #19925, #35443, #36211 ) ;
#36825 = CARTESIAN_POINT ( 'NONE',  ( -0.5455278134075216556, 0.000000000000000000, -2.204724409448810540 ) ) ;
#36826 = EDGE_CURVE ( 'NONE', #21641, #44588, #29237, .T. ) ;
#36827 = ORIENTED_EDGE ( 'NONE', *, *, #22650, .F. ) ;
#36828 = DIRECTION ( 'NONE',  ( 1.734723475976806848E-16, 0.000000000000000000, 1.000000000000000000 ) ) ;
#36829 = CARTESIAN_POINT ( 'NONE',  ( -1.712496953225537188, 3.346456692913386100, 0.7874015748031456541 ) ) ;
#36830 = ORIENTED_EDGE ( 'NONE', *, *, #5054, .T. ) ;
#36831 = LINE ( 'NONE', #43781, #26282 ) ;
#36832 = VECTOR ( 'NONE', #23903, 39.37007874015748143 ) ;
#36833 = DIRECTION ( 'NONE',  ( 0.000000000000000000, 0.000000000000000000, -1.000000000000000000 ) ) ;
#36834 = EDGE_CURVE ( 'NONE', #8104, #8660, #21496, .T. ) ;
#36835 = CARTESIAN_POINT ( 'NONE',  ( 0.000000000000000000, 0.000000000000000000, 0.000000000000000000 ) ) ;
#36836 = VECTOR ( 'NONE', #45019, 39.37007874015748143 ) ;
#36837 = ADVANCED_FACE ( 'NONE', ( #18381 ), #49069, .F. ) ;
#36838 = ORIENTED_EDGE ( 'NONE', *, *, #9043, .F. ) ;
#36839 = DIRECTION ( 'NONE',  ( -3.469446951953613696E-16, 0.000000000000000000, -1.000000000000000000 ) ) ;
#36840 = ORIENTED_EDGE ( 'NONE', *, *, #34821, .T. ) ;
#36841 = FACE_BOUND ( 'NONE', #24261, .T. ) ;
#36842 = DIRECTION ( 'NONE',  ( 0.000000000000000000, -1.000000000000000000, 0.000000000000000000 ) ) ;
#36843 = CARTESIAN_POINT ( 'NONE',  ( -1.712496953225537188, 0.000000000000000000, 0.9055118110236167750 ) ) ;
#36844 = DIRECTION ( 'NONE',  ( 1.734723475976806848E-16, -0.000000000000000000, 1.000000000000000000 ) ) ;
#36845 = ORIENTED_EDGE ( 'NONE', *, *, #26152, .F. ) ;
#36846 = EDGE_LOOP ( 'NONE', ( #9749, #14606, #5711 ) ) ;
#36847 = CARTESIAN_POINT ( 'NONE',  ( 1.560669927219590525, 3.267716535433071279, 0.2755905511810996522 ) ) ;
#36848 = EDGE_LOOP ( 'NONE', ( #25889, #26686, #5674, #38967 ) ) ;
#36849 = LINE ( 'NONE', #28574, #21127 ) ;
#36850 = EDGE_LOOP ( 'NONE', ( #23261, #29614, #33824, #48428, #50777, #3321, #46350, #3996 ) ) ;
#36851 = DIRECTION ( 'NONE',  ( 0.9998717552508121775, 0.01601477604151182663, 0.000000000000000000 ) ) ;
#36852 = ORIENTED_EDGE ( 'NONE', *, *, #51006, .F. ) ;
#36853 = DIRECTION ( 'NONE',  ( -3.469446951953613696E-16, 0.000000000000000000, -1.000000000000000000 ) ) ;
#36854 = VECTOR ( 'NONE', #48144, 39.37007874015748143 ) ;
#36855 = EDGE_CURVE ( 'NONE', #38556, #30992, #42125, .T. ) ;
#36856 = CARTESIAN_POINT ( 'NONE',  ( -2.157989646284840468, 1.673342082170779621, -0.1819910592820468964 ) ) ;
#36857 = VECTOR ( 'NONE', #34836, 39.37007874015748143 ) ;
#36858 = ORIENTED_EDGE ( 'NONE', *, *, #10803, .F. ) ;
#36859 = CARTESIAN_POINT ( 'NONE',  ( 0.7381027496705272473, 1.730766751998747521, -2.859439394060913298 ) ) ;
#36860 = ORIENTED_EDGE ( 'NONE', *, *, #26883, .F. ) ;
#36861 = B_SPLINE_CURVE_WITH_KNOTS ( 'NONE', 3,
 ( #27699, #23575, #11959, #31589 ),
 .UNSPECIFIED., .F., .F.,
 ( 4, 4 ),
 ( 2.032841336367455452E-07, 0.01843528932679509152 ),
 .UNSPECIFIED. ) ;
#36862 = EDGE_LOOP ( 'NONE', ( #42327, #33764, #28813, #20879 ) ) ;
#36863 = EDGE_CURVE ( 'NONE', #17189, #47793, #45975, .T. ) ;
#36864 = VECTOR ( 'NONE', #5495, 39.37007874015748143 ) ;
#36865 = EDGE_CURVE ( 'NONE', #40614, #12124, #45216, .T. ) ;
#36866 = ORIENTED_EDGE ( 'NONE', *, *, #9998, .T. ) ;
#36867 = ORIENTED_EDGE ( 'NONE', *, *, #41438, .F. ) ;
#36868 = CARTESIAN_POINT ( 'NONE',  ( 1.015142113812069979, 0.000000000000000000, 1.732283464566921172 ) ) ;
#36869 = CARTESIAN_POINT ( 'NONE',  ( -2.464291103507775915, 0.000000000000000000, -1.626664315311338260 ) ) ;
#36870 = EDGE_CURVE ( 'NONE', #19430, #13784, #15616, .T. ) ;
#36871 = VERTEX_POINT ( 'NONE', #10387 ) ;
#36872 = CARTESIAN_POINT ( 'NONE',  ( -0.4358240471401270688, 1.708633904392455660, 2.677201428532125949 ) ) ;
#36873 = ORIENTED_EDGE ( 'NONE', *, *, #40851, .T. ) ;
#36874 = CARTESIAN_POINT ( 'NONE',  ( -0.07591351300297333182, 0.000000000000000000, -1.732283464566922726 ) ) ;
#36875 = CARTESIAN_POINT ( 'NONE',  ( 2.966619746092224783E-16, 3.313179664429866556, 2.422428857167389982 ) ) ;
#36876 = B_SPLINE_CURVE_WITH_KNOTS ( 'NONE', 3,
 ( #46431, #50041, #26088, #11102 ),
 .UNSPECIFIED., .F., .F.,
 ( 4, 4 ),
 ( 4.094226701244036431E-07, 0.04399192588115360264 ),
 .UNSPECIFIED. ) ;
#36877 = ORIENTED_EDGE ( 'NONE', *, *, #6525, .T. ) ;
#36878 = LINE ( 'NONE', #28088, #17068 ) ;
#36879 = CARTESIAN_POINT ( 'NONE',  ( 0.7423782071083087075, 3.346456692913386100, 0.3149606299212576177 ) ) ;
#36880 = ORIENTED_EDGE ( 'NONE', *, *, #30853, .T. ) ;
#36881 = CARTESIAN_POINT ( 'NONE',  ( -0.6214413264104939882, 0.000000000000000000, 1.102362204724404160 ) ) ;
#36882 = CARTESIAN_POINT ( 'NONE',  ( 0.000000000000000000, 3.267716535433071279, -1.299212598425193210 ) ) ;
#36883 = EDGE_CURVE ( 'NONE', #50795, #24825, #33131, .T. ) ;
#36884 = CARTESIAN_POINT ( 'NONE',  ( 1.785493683324574254, 0.000000000000000000, -1.119626681005672530 ) ) ;
#36885 = DIRECTION ( 'NONE',  ( -1.000000000000000000, -0.000000000000000000, -0.000000000000000000 ) ) ;
#36886 = EDGE_CURVE ( 'NONE', #11192, #16625, #46604, .T. ) ;
#36887 = DIRECTION ( 'NONE',  ( -0.4738686624729965269, 0.000000000000000000, -0.8805955318567391110 ) ) ;
#36888 = ORIENTED_EDGE ( 'NONE', *, *, #22756, .T. ) ;
#36889 = DIRECTION ( 'NONE',  ( 0.000000000000000000, 0.000000000000000000, -1.000000000000000000 ) ) ;
#36890 = VECTOR ( 'NONE', #34383, 39.37007874015748143 ) ;
#36891 = VECTOR ( 'NONE', #41649, 39.37007874015748143 ) ;
#36892 = CARTESIAN_POINT ( 'NONE',  ( -1.195183497228115035E-16, 3.267716535433071279, -0.9448818897637765168 ) ) ;
#36893 = EDGE_CURVE ( 'NONE', #31173, #27651, #48814, .T. ) ;
#36894 = ORIENTED_EDGE ( 'NONE', *, *, #37870, .T. ) ;
#36895 = VECTOR ( 'NONE', #13829, 39.37007874015748143 ) ;
#36896 = LINE ( 'NONE', #1517, #34183 ) ;
#36897 = EDGE_CURVE ( 'NONE', #39028, #26405, #30006, .T. ) ;
#36898 = ADVANCED_FACE ( 'NONE', ( #34143 ), #14513, .F. ) ;
#36899 = VERTEX_POINT ( 'NONE', #46477 ) ;
#36900 = CARTESIAN_POINT ( 'NONE',  ( 0.002207914879453961969, 5.905511811023623991, 0.04916304461325442243 ) ) ;
#36901 = DIRECTION ( 'NONE',  ( -0.000000000000000000, 0.000000000000000000, 1.000000000000000000 ) ) ;
#36902 = CARTESIAN_POINT ( 'NONE',  ( 2.009930929872536964, 1.574803149606302854, -0.8055662819783826478 ) ) ;
#36903 = CARTESIAN_POINT ( 'NONE',  ( -0.5455278134075214336, 0.000000000000000000, 0.3149606299212577287 ) ) ;
#36904 = CARTESIAN_POINT ( 'NONE',  ( 0.000000000000000000, 3.267716535433071279, 0.000000000000000000 ) ) ;
#36905 = ORIENTED_EDGE ( 'NONE', *, *, #45825, .T. ) ;
#36906 = CARTESIAN_POINT ( 'NONE',  ( 0.9442395380435398833, 1.624600478255878055, -2.074157072296122450 ) ) ;
#36907 = DIRECTION ( 'NONE',  ( 0.000000000000000000, 0.000000000000000000, 1.000000000000000000 ) ) ;
#36908 = VERTEX_POINT ( 'NONE', #26871 ) ;
#36909 = CARTESIAN_POINT ( 'NONE',  ( 2.755905511811024056, 2.913385826771657250, 1.023622047244094446 ) ) ;
#36910 = VECTOR ( 'NONE', #19960, 39.37007874015748854 ) ;
#36911 = ORIENTED_EDGE ( 'NONE', *, *, #11069, .T. ) ;
#36912 = DIRECTION ( 'NONE',  ( -0.000000000000000000, 0.000000000000000000, 1.000000000000000000 ) ) ;
#36913 = CARTESIAN_POINT ( 'NONE',  ( 2.455254121193349182, 1.659040775461701811, -1.640354758330454077 ) ) ;
#36914 = DIRECTION ( 'NONE',  ( -0.7818314824680221431, 7.240175090764046435E-17, -0.6234898018587431423 ) ) ;
#36915 = CARTESIAN_POINT ( 'NONE',  ( -2.254539048594918604, 1.675968636652996224, -0.9101168094050288149 ) ) ;
#36916 = ORIENTED_EDGE ( 'NONE', *, *, #6618, .F. ) ;
#36917 = VERTEX_POINT ( 'NONE', #19377 ) ;
#36918 = LINE ( 'NONE', #25291, #11967 ) ;
#36919 = CARTESIAN_POINT ( 'NONE',  ( 0.9838852166858930159, 5.905511811023623991, 1.929635236160318179 ) ) ;
#36920 = FACE_BOUND ( 'NONE', #26790, .T. ) ;
#36921 = ORIENTED_EDGE ( 'NONE', *, *, #48938, .T. ) ;
#36922 = CARTESIAN_POINT ( 'NONE',  ( -2.454875160333845674, 0.000000000000000000, -0.03937007874015881204 ) ) ;
#36923 = LINE ( 'NONE', #37436, #20058 ) ;
#36924 = EDGE_CURVE ( 'NONE', #50043, #15158, #34642, .T. ) ;
#36925 = AXIS2_PLACEMENT_3D ( 'NONE', #33094, #41337, #29195 ) ;
#36926 = EDGE_LOOP ( 'NONE', ( #32508, #28690, #29633, #48115 ) ) ;
#36927 = DIRECTION ( 'NONE',  ( -1.000000000000000000, 0.000000000000000000, 0.000000000000000000 ) ) ;
#36928 = EDGE_CURVE ( 'NONE', #29512, #42332, #15519, .T. ) ;
#36929 = EDGE_CURVE ( 'NONE', #43136, #33404, #23510, .T. ) ;
#36930 = CARTESIAN_POINT ( 'NONE',  ( -1.883118996231724962, 1.042646074230517472, -1.732359575492526504 ) ) ;
#36931 = VERTEX_POINT ( 'NONE', #27130 ) ;
#36932 = VERTEX_POINT ( 'NONE', #46968 ) ;
#36933 = VECTOR ( 'NONE', #29932, 39.37007874015748143 ) ;
#36934 = ADVANCED_FACE ( 'NONE', ( #7770 ), #50325, .F. ) ;
#36935 = ORIENTED_EDGE ( 'NONE', *, *, #13159, .T. ) ;
#36936 = DIRECTION ( 'NONE',  ( -9.701723960855733411E-17, 1.000000000000000000, -8.476140964546406840E-17 ) ) ;
#36937 = LINE ( 'NONE', #43630, #48861 ) ;
#36938 = CARTESIAN_POINT ( 'NONE',  ( -1.597750071202345135, 0.000000000000000000, -0.7364305798568749895 ) ) ;
#36939 = DIRECTION ( 'NONE',  ( 1.000000000000000000, 0.000000000000000000, -3.469446951953613696E-16 ) ) ;
#36940 = AXIS2_PLACEMENT_3D ( 'NONE', #33576, #9298, #41307 ) ;
#36941 = ORIENTED_EDGE ( 'NONE', *, *, #19262, .F. ) ;
#36942 = B_SPLINE_CURVE_WITH_KNOTS ( 'NONE', 3,
 ( #18345, #40259, #50786, #15729 ),
 .UNSPECIFIED., .F., .F.,
 ( 4, 4 ),
 ( 2.472934783152532252E-07, 0.01680610193886662024 ),
 .UNSPECIFIED. ) ;
#36943 = ORIENTED_EDGE ( 'NONE', *, *, #25868, .F. ) ;
#36944 = LINE ( 'NONE', #538, #20829 ) ;
#36945 = LINE ( 'NONE', #12666, #41137 ) ;
#36946 = FACE_BOUND ( 'NONE', #7864, .T. ) ;
#36947 = EDGE_CURVE ( 'NONE', #23628, #39512, #31524, .T. ) ;
#36948 = CIRCLE ( 'NONE', #34473, 2.165354330708661568 ) ;
#36949 = DIRECTION ( 'NONE',  ( 1.734723475976806848E-16, -0.000000000000000000, 1.000000000000000000 ) ) ;
#36950 = CARTESIAN_POINT ( 'NONE',  ( -1.905671854841497259, 1.205361022782829114E-17, 2.256015092822653667 ) ) ;
#36951 = ADVANCED_FACE ( 'NONE', ( #15764 ), #35145, .T. ) ;
#36952 = FACE_OUTER_BOUND ( 'NONE', #10216, .T. ) ;
#36953 = CARTESIAN_POINT ( 'NONE',  ( 2.138597145901430352, 1.574803149606302854, 0.3393547186367255608 ) ) ;
#36954 = ORIENTED_EDGE ( 'NONE', *, *, #28843, .T. ) ;
#36955 = CARTESIAN_POINT ( 'NONE',  ( 0.1155636338427008941, -0.5222242541845523167, 0.000000000000000000 ) ) ;
#36956 = DIRECTION ( 'NONE',  ( -0.000000000000000000, 1.000000000000000000, -0.000000000000000000 ) ) ;
#36957 = EDGE_CURVE ( 'NONE', #6865, #43780, #3393, .T. ) ;
#36958 = EDGE_LOOP ( 'NONE', ( #45016, #38321, #194, #21657 ) ) ;
#36959 = ORIENTED_EDGE ( 'NONE', *, *, #38843, .F. ) ;
#36960 = CARTESIAN_POINT ( 'NONE',  ( -1.636583440222564301, 3.346456692913386100, -1.456692913385822186 ) ) ;
#36961 = DIRECTION ( 'NONE',  ( -3.469446951953613696E-16, 0.000000000000000000, -1.000000000000000000 ) ) ;
#36962 = CIRCLE ( 'NONE', #29551, 2.165354330708661568 ) ;
#36963 = ORIENTED_EDGE ( 'NONE', *, *, #2888, .T. ) ;
#36964 = ORIENTED_EDGE ( 'NONE', *, *, #22072, .F. ) ;
#36965 = LINE ( 'NONE', #13725, #41900 ) ;
#36966 = CIRCLE ( 'NONE', #14701, 2.493791675044291445 ) ;
#36967 = EDGE_LOOP ( 'NONE', ( #27159, #23135, #28050, #9228 ) ) ;
#36968 = VECTOR ( 'NONE', #47593, 39.37007874015748143 ) ;
#36969 = VECTOR ( 'NONE', #22734, 39.37007874015748143 ) ;
#36970 = CARTESIAN_POINT ( 'NONE',  ( 1.363819533518803251, 3.346456692913386100, -0.1574803149606304187 ) ) ;
#36971 = DIRECTION ( 'NONE',  ( 0.000000000000000000, -1.000000000000000000, 0.000000000000000000 ) ) ;
#36972 = CIRCLE ( 'NONE', #30377, 2.164630168518208109 ) ;
#36973 = ORIENTED_EDGE ( 'NONE', *, *, #49302, .T. ) ;
#36974 = ORIENTED_EDGE ( 'NONE', *, *, #34378, .T. ) ;
#36975 = VERTEX_POINT ( 'NONE', #47217 ) ;
#36976 = CARTESIAN_POINT ( 'NONE',  ( -1.572100079625529556, 1.686782128119526325, 1.874211475136934535 ) ) ;
#36977 = ORIENTED_EDGE ( 'NONE', *, *, #47720, .T. ) ;
#36978 = ORIENTED_EDGE ( 'NONE', *, *, #48817, .T. ) ;
#36979 = LINE ( 'NONE', #13476, #36373 ) ;
#36980 = CARTESIAN_POINT ( 'NONE',  ( -0.5455278134075208785, 0.000000000000000000, 1.574803149606291974 ) ) ;
#36981 = CARTESIAN_POINT ( 'NONE',  ( -2.903572669614648660, 5.118110236220475784, 1.294565943894125937 ) ) ;
#36982 = AXIS2_PLACEMENT_3D ( 'NONE', #3152, #27144, #3659 ) ;
#36983 = ORIENTED_EDGE ( 'NONE', *, *, #36213, .F. ) ;
#36984 = CARTESIAN_POINT ( 'NONE',  ( 1.015142113812069313, 3.267716535433071279, -3.521981712565032389E-16 ) ) ;
#36985 = CARTESIAN_POINT ( 'NONE',  ( 0.8182917201112819283, 3.346456692913386100, -0.3543307086614175816 ) ) ;
#36986 = DIRECTION ( 'NONE',  ( -0.000000000000000000, 1.000000000000000000, -0.000000000000000000 ) ) ;
#36987 = ORIENTED_EDGE ( 'NONE', *, *, #50581, .F. ) ;
#36988 = DIRECTION ( 'NONE',  ( 1.734723475976806848E-16, 0.000000000000000000, 1.000000000000000000 ) ) ;
#36989 = LINE ( 'NONE', #43942, #40057 ) ;
#36990 = EDGE_CURVE ( 'NONE', #10750, #37269, #14767, .T. ) ;
#36991 = ADVANCED_FACE ( 'NONE', ( #42373 ), #23017, .F. ) ;
#36992 = CARTESIAN_POINT ( 'NONE',  ( 2.076281802138679300, 3.346456692913386100, -0.3543307086614178592 ) ) ;
#36993 = ORIENTED_EDGE ( 'NONE', *, *, #10625, .T. ) ;
#36994 = VERTEX_POINT ( 'NONE', #50823 ) ;
#36995 = LENGTH_MEASURE_WITH_UNIT ( LENGTH_MEASURE( 0.02539999999999999897 ), #48052 );
#36996 = EDGE_CURVE ( 'NONE', #46747, #49534, #10886, .T. ) ;
#36997 = CARTESIAN_POINT ( 'NONE',  ( -1.232620761116186126, 1.574803149606302854, -1.780282403660753410 ) ) ;
#36998 =( BOUNDED_CURVE ( )  B_SPLINE_CURVE ( 3, ( #1769, #45370, #48968, #10031 ),
 .UNSPECIFIED., .F., .F. ) 
 B_SPLINE_CURVE_WITH_KNOTS ( ( 4, 4 ),
 ( 4.674186630050075841, 4.725131524484309509 ),
 .UNSPECIFIED. ) 
 CURVE ( )  GEOMETRIC_REPRESENTATION_ITEM ( )  RATIONAL_B_SPLINE_CURVE ( ( 1.000000000000000000, 0.9997837298384644189, 0.9997837298384644189, 1.000000000000000000 ) ) 
 REPRESENTATION_ITEM ( '' )  );
#36999 = AXIS2_PLACEMENT_3D ( 'NONE', #32924, #17669, #32666 ) ;
#37000 = DIRECTION ( 'NONE',  ( -1.045785279492541006E-16, -1.000000000000000000, -5.036236473261559574E-17 ) ) ;
#37001 = EDGE_CURVE ( 'NONE', #5174, #49411, #4930, .T. ) ;
#37002 = DIRECTION ( 'NONE',  ( 0.000000000000000000, -1.000000000000000000, 0.000000000000000000 ) ) ;
#37003 = VERTEX_POINT ( 'NONE', #38269 ) ;
#37004 = ORIENTED_EDGE ( 'NONE', *, *, #47248, .T. ) ;
#37005 = CARTESIAN_POINT ( 'NONE',  ( -2.100227814008681637, 0.000000000000000000, -2.076109931251943763 ) ) ;
#37006 = CIRCLE ( 'NONE', #8134, 2.165354330708661568 ) ;
#37007 = EDGE_LOOP ( 'NONE', ( #11579, #25088, #18802, #45132 ) ) ;
#37008 = CARTESIAN_POINT ( 'NONE',  ( 0.000000000000000000, 3.267716535433071279, -0.3543307086614171930 ) ) ;
#37009 = CARTESIAN_POINT ( 'NONE',  ( -0.6214413264104939882, 3.346456692913386100, 1.102362204724404160 ) ) ;
#37010 = VECTOR ( 'NONE', #40850, 39.37007874015748854 ) ;
#37011 = VECTOR ( 'NONE', #29015, 39.37007874015748143 ) ;
#37012 = EDGE_CURVE ( 'NONE', #49445, #30308, #2891, .T. ) ;
#37013 = LINE ( 'NONE', #21255, #46438 ) ;
#37014 = LINE ( 'NONE', #49341, #48295 ) ;
#37015 = CARTESIAN_POINT ( 'NONE',  ( -1.166969139818015977, 3.346456692913386100, -1.102362204724405270 ) ) ;
#37016 = EDGE_LOOP ( 'NONE', ( #960, #18122, #6280, #15459 ) ) ;
#37017 = DIRECTION ( 'NONE',  ( 0.000000000000000000, 0.000000000000000000, -1.000000000000000000 ) ) ;
#37018 = EDGE_CURVE ( 'NONE', #10535, #18938, #50572, .T. ) ;
#37019 = CARTESIAN_POINT ( 'NONE',  ( 1.015142113812069313, 3.267716535433071279, 0.4724409448818868706 ) ) ;
#37020 = ORIENTED_EDGE ( 'NONE', *, *, #30489, .T. ) ;
#37021 = DIRECTION ( 'NONE',  ( -3.469446951953613696E-16, 0.000000000000000000, -1.000000000000000000 ) ) ;
#37022 = CARTESIAN_POINT ( 'NONE',  ( 1.558105373646060388, 3.267716535433071279, 1.417322834645662777 ) ) ;
#37023 = FACE_OUTER_BOUND ( 'NONE', #7702, .T. ) ;
#37024 = VERTEX_POINT ( 'NONE', #39010 ) ;
#37025 = CARTESIAN_POINT ( 'NONE',  ( 0.1968503937007873017, 0.000000000000000000, -0.3149606299212591165 ) ) ;
#37026 = CARTESIAN_POINT ( 'NONE',  ( 2.074634995449671226, 0.01972627099085171726, -0.1424341672639439782 ) ) ;
#37027 = ORIENTED_EDGE ( 'NONE', *, *, #14839, .T. ) ;
#37028 = LINE ( 'NONE', #44496, #26314 ) ;
#37029 = DIRECTION ( 'NONE',  ( 1.000000000000000000, -0.000000000000000000, 0.000000000000000000 ) ) ;
#37030 = ORIENTED_EDGE ( 'NONE', *, *, #7943, .T. ) ;
#37031 = DIRECTION ( 'NONE',  ( -0.000000000000000000, 1.000000000000000000, -0.000000000000000000 ) ) ;
#37032 = EDGE_CURVE ( 'NONE', #2471, #21641, #31274, .T. ) ;
#37033 = FACE_OUTER_BOUND ( 'NONE', #45641, .T. ) ;
#37034 = DIRECTION ( 'NONE',  ( -3.469446951953613696E-16, 0.000000000000000000, -1.000000000000000000 ) ) ;
#37035 = LINE ( 'NONE', #14549, #7090 ) ;
#37036 = AXIS2_PLACEMENT_3D ( 'NONE', #10107, #42101, #9855 ) ;
#37037 = DIRECTION ( 'NONE',  ( -1.000000000000000000, 0.000000000000000000, 0.000000000000000000 ) ) ;
#37038 = VERTEX_POINT ( 'NONE', #3902 ) ;
#37039 = ORIENTED_EDGE ( 'NONE', *, *, #29945, .F. ) ;
#37040 = CARTESIAN_POINT ( 'NONE',  ( 0.08139965876239094178, 1.610780518492231694, 0.000000000000000000 ) ) ;
#37041 = PLANE ( 'NONE',  #22180 ) ;
#37042 = ORIENTED_EDGE ( 'NONE', *, *, #14094, .T. ) ;
#37043 = DIRECTION ( 'NONE',  ( -3.469446951953613696E-16, 0.000000000000000000, -1.000000000000000000 ) ) ;
#37044 = DIRECTION ( 'NONE',  ( -1.000000000000000000, 0.000000000000000000, 0.000000000000000000 ) ) ;
#37045 = CARTESIAN_POINT ( 'NONE',  ( 1.687984952120845428, 3.267716535433071279, 1.259842519685033135 ) ) ;
#37046 = CARTESIAN_POINT ( 'NONE',  ( 2.378961647330872786, 0.000000000000000000, -0.5118110236220471121 ) ) ;
#37047 = VECTOR ( 'NONE', #47034, 39.37007874015748143 ) ;
#37048 = VERTEX_POINT ( 'NONE', #7014 ) ;
#37049 = ORIENTED_EDGE ( 'NONE', *, *, #43663, .F. ) ;
#37050 = LINE ( 'NONE', #13044, #4016 ) ;
#37051 = FACE_OUTER_BOUND ( 'NONE', #46823, .T. ) ;
#37052 = DIRECTION ( 'NONE',  ( 0.000000000000000000, 0.000000000000000000, -1.000000000000000000 ) ) ;
#37053 = ORIENTED_EDGE ( 'NONE', *, *, #24749, .F. ) ;
#37054 = VECTOR ( 'NONE', #46320, 39.37007874015748143 ) ;
#37055 = DIRECTION ( 'NONE',  ( -1.000000000000000000, 0.000000000000000000, 0.000000000000000000 ) ) ;
#37056 = FACE_BOUND ( 'NONE', #47317, .T. ) ;
#37057 = VERTEX_POINT ( 'NONE', #18 ) ;
#37058 = DIRECTION ( 'NONE',  ( -0.000000000000000000, 1.000000000000000000, -0.000000000000000000 ) ) ;
#37059 = ORIENTED_EDGE ( 'NONE', *, *, #19422, .T. ) ;
#37060 = ORIENTED_EDGE ( 'NONE', *, *, #49327, .F. ) ;
#37061 = VECTOR ( 'NONE', #17964, 39.37007874015748143 ) ;
#37062 = CARTESIAN_POINT ( 'NONE',  ( -1.252725762389900188, 0.005294869427718575626, -1.265815002325405336 ) ) ;
#37063 = EDGE_CURVE ( 'NONE', #50100, #22707, #18643, .T. ) ;
#37064 = EDGE_CURVE ( 'NONE', #4522, #30941, #13188, .T. ) ;
#37065 = ORIENTED_EDGE ( 'NONE', *, *, #32021, .T. ) ;
#37066 = CARTESIAN_POINT ( 'NONE',  ( 2.145573199472960546, 1.752687626240418073, -2.028682376369756568 ) ) ;
#37067 = EDGE_CURVE ( 'NONE', #50364, #47890, #28809, .T. ) ;
#37068 = CARTESIAN_POINT ( 'NONE',  ( 1.287906020515830141, 3.267716535433071279, -4.468321617281355077E-16 ) ) ;
#37069 = ORIENTED_EDGE ( 'NONE', *, *, #50377, .F. ) ;
#37070 = LINE ( 'NONE', #33202, #22004 ) ;
#37071 = DIRECTION ( 'NONE',  ( -3.469446951953613696E-16, 0.000000000000000000, -1.000000000000000000 ) ) ;
#37072 = EDGE_CURVE ( 'NONE', #31903, #26214, #32557, .T. ) ;
#37073 = VECTOR ( 'NONE', #43357, 39.37007874015748143 ) ;
#37074 = DIRECTION ( 'NONE',  ( 1.000000000000000000, 0.000000000000000000, 0.000000000000000000 ) ) ;
#37075 = DIRECTION ( 'NONE',  ( -1.000000000000000000, 0.000000000000000000, -0.000000000000000000 ) ) ;
#37076 = CARTESIAN_POINT ( 'NONE',  ( -2.009930929872524974, 5.905511811023623991, -0.8055662819784118467 ) ) ;
#37077 = ORIENTED_EDGE ( 'NONE', *, *, #38133, .F. ) ;
#37078 = CARTESIAN_POINT ( 'NONE',  ( 0.1067246931122726866, 0.02962905676920215767, 0.000000000000000000 ) ) ;
#37079 = ADVANCED_FACE ( 'NONE', ( #24024 ), #48249, .F. ) ;
#37080 = DIRECTION ( 'NONE',  ( 1.734723475976806848E-16, -0.000000000000000000, 1.000000000000000000 ) ) ;
#37081 = AXIS2_PLACEMENT_3D ( 'NONE', #28402, #43634, #47733 ) ;
#37082 = EDGE_LOOP ( 'NONE', ( #6751, #9343, #37626, #34011, #37977 ) ) ;
#37083 = FACE_OUTER_BOUND ( 'NONE', #47131, .T. ) ;
#37084 = CARTESIAN_POINT ( 'NONE',  ( 0.000000000000000000, 1.574803149606302854, 0.000000000000000000 ) ) ;
#37085 = ORIENTED_EDGE ( 'NONE', *, *, #14336, .T. ) ;
#37086 = DIRECTION ( 'NONE',  ( -3.469446951953613696E-16, 0.000000000000000000, -1.000000000000000000 ) ) ;
#37087 = EDGE_CURVE ( 'NONE', #45414, #1023, #4921, .T. ) ;
#37088 = CARTESIAN_POINT ( 'NONE',  ( -1.439733046521776139, 0.000000000000000000, 0.3149606299212578953 ) ) ;
#37089 = CARTESIAN_POINT ( 'NONE',  ( -1.166969139818015533, 3.346456692913386100, 0.4724409448818871482 ) ) ;
#37090 = ORIENTED_EDGE ( 'NONE', *, *, #25202, .F. ) ;
#37091 = CARTESIAN_POINT ( 'NONE',  ( 1.636583440222563857, 3.346456692913386100, 0.1181102362204701633 ) ) ;
#37092 = VECTOR ( 'NONE', #16047, 39.37007874015748143 ) ;
#37093 = ORIENTED_EDGE ( 'NONE', *, *, #5355, .T. ) ;
#37094 = FACE_BOUND ( 'NONE', #25158, .T. ) ;
#37095 = EDGE_CURVE ( 'NONE', #5048, #20757, #35905, .T. ) ;
#37096 = CARTESIAN_POINT ( 'NONE',  ( 1.775400203342704764, 1.475394431724762478, -2.359903268218703332 ) ) ;
#37097 = CARTESIAN_POINT ( 'NONE',  ( -1.439733046521776139, 0.000000000000000000, 1.259842519685033357 ) ) ;
#37098 = DIRECTION ( 'NONE',  ( -3.986037398843765983E-20, -1.000000000000000000, -1.160734090543304660E-16 ) ) ;
#37099 = ORIENTED_EDGE ( 'NONE', *, *, #49539, .T. ) ;
#37100 = VERTEX_POINT ( 'NONE', #40551 ) ;
#37101 = PLANE ( 'NONE',  #30390 ) ;
#37102 = ORIENTED_EDGE ( 'NONE', *, *, #33338, .T. ) ;
#37103 = ADVANCED_FACE ( 'NONE', ( #24540 ), #47989, .F. ) ;
#37104 = CARTESIAN_POINT ( 'NONE',  ( 2.106197740627112402, 0.000000000000000000, 0.1574803149606280872 ) ) ;
#37105 = ORIENTED_EDGE ( 'NONE', *, *, #50373, .T. ) ;
#37106 = EDGE_CURVE ( 'NONE', #10548, #49624, #20923, .T. ) ;
#37107 = LINE ( 'NONE', #43807, #4197 ) ;
#37108 = AXIS2_PLACEMENT_3D ( 'NONE', #18942, #18439, #34193 ) ;
#37109 = ORIENTED_EDGE ( 'NONE', *, *, #2056, .F. ) ;
#37110 = DIRECTION ( 'NONE',  ( 1.000000000000000000, 0.000000000000000000, 0.000000000000000000 ) ) ;
#37111 = B_SPLINE_CURVE_WITH_KNOTS ( 'NONE', 3,
 ( #19973, #39865, #12762, #4757 ),
 .UNSPECIFIED., .F., .F.,
 ( 4, 4 ),
 ( 2.925317793448864180E-05, 0.02001440658342761025 ),
 .UNSPECIFIED. ) ;
#37112 = DIRECTION ( 'NONE',  ( -1.000000000000000000, 0.000000000000000000, -0.000000000000000000 ) ) ;
#37113 = EDGE_LOOP ( 'NONE', ( #9930, #13944, #34881, #12168 ) ) ;
#37114 = B_SPLINE_CURVE_WITH_KNOTS ( 'NONE', 3,
 ( #41879, #22764, #14766, #30515 ),
 .UNSPECIFIED., .F., .F.,
 ( 4, 4 ),
 ( 0.001750221845292458797, 0.004250273344973329141 ),
 .UNSPECIFIED. ) ;
#37115 = FACE_OUTER_BOUND ( 'NONE', #31746, .T. ) ;
#37116 = ORIENTED_EDGE ( 'NONE', *, *, #7485, .F. ) ;
#37117 = EDGE_LOOP ( 'NONE', ( #16119, #42829, #49265, #44833 ) ) ;
#37118 = EDGE_CURVE ( 'NONE', #1350, #34628, #16282, .T. ) ;
#37119 = VECTOR ( 'NONE', #50515, 39.37007874015748143 ) ;
#37120 = VECTOR ( 'NONE', #7340, 39.37007874015748143 ) ;
#37121 = ORIENTED_EDGE ( 'NONE', *, *, #3978, .F. ) ;
#37122 = ORIENTED_EDGE ( 'NONE', *, *, #24585, .F. ) ;
#37123 = EDGE_CURVE ( 'NONE', #31137, #6824, #27891, .T. ) ;
#37124 = CARTESIAN_POINT ( 'NONE',  ( 1.560669927219590747, 3.267716535433071279, -0.1574803149606304187 ) ) ;
#37125 = EDGE_CURVE ( 'NONE', #3769, #47245, #19883, .T. ) ;
#37126 = VERTEX_POINT ( 'NONE', #17064 ) ;
#37127 = AXIS2_PLACEMENT_3D ( 'NONE', #17344, #33104, #20691 ) ;
#37128 = CARTESIAN_POINT ( 'NONE',  ( 2.121469926805689354, 6.692913385826772199, -0.4337334748181388422 ) ) ;
#37129 = VERTEX_POINT ( 'NONE', #16025 ) ;
#37130 = CARTESIAN_POINT ( 'NONE',  ( -2.574535399664545920, 1.576620825002011061, 0.7847720717991576445 ) ) ;
#37131 = DIRECTION ( 'NONE',  ( 0.000000000000000000, 1.000000000000000000, 0.000000000000000000 ) ) ;
#37132 = ORIENTED_EDGE ( 'NONE', *, *, #10469, .T. ) ;
#37133 = B_SPLINE_CURVE_WITH_KNOTS ( 'NONE', 3,
 ( #11254, #35507, #26983, #4015 ),
 .UNSPECIFIED., .F., .F.,
 ( 4, 4 ),
 ( 2.656726248922481073E-07, 0.01672130471895163367 ),
 .UNSPECIFIED. ) ;
#37134 = B_SPLINE_CURVE_WITH_KNOTS ( 'NONE', 3,
 ( #17143, #43976, #40635, #21014 ),
 .UNSPECIFIED., .F., .F.,
 ( 4, 4 ),
 ( 0.1211775127643062860, 0.1625894504277921315 ),
 .UNSPECIFIED. ) ;
#37135 = FACE_OUTER_BOUND ( 'NONE', #14364, .T. ) ;
#37136 = LINE ( 'NONE', #14134, #26970 ) ;
#37137 = EDGE_LOOP ( 'NONE', ( #32368, #41009, #43100, #4882 ) ) ;
#37138 = DIRECTION ( 'NONE',  ( -0.000000000000000000, 1.000000000000000000, -0.000000000000000000 ) ) ;
#37139 = DIRECTION ( 'NONE',  ( -3.469446951953613696E-16, 0.000000000000000000, -1.000000000000000000 ) ) ;
#37140 = FACE_OUTER_BOUND ( 'NONE', #10088, .T. ) ;
#37141 = FACE_OUTER_BOUND ( 'NONE', #22501, .T. ) ;
#37142 = CARTESIAN_POINT ( 'NONE',  ( 0.9836083787002611878, 1.574803149606302854, -1.929060376159698720 ) ) ;
#37143 = VERTEX_POINT ( 'NONE', #8022 ) ;
#37144 = CARTESIAN_POINT ( 'NONE',  ( 1.363819533518803251, 3.346456692913386100, -0.9842519685039348154 ) ) ;
#37145 = EDGE_CURVE ( 'NONE', #40318, #40457, #28144, .T. ) ;
#37146 = CARTESIAN_POINT ( 'NONE',  ( 0.07982360342473591996, 1.709180471932028711, 0.000000000000000000 ) ) ;
#37147 = VERTEX_POINT ( 'NONE', #43883 ) ;
#37148 = CARTESIAN_POINT ( 'NONE',  ( 0.000000000000000000, 3.267716535433071279, 0.9448818897637746295 ) ) ;
#37149 = ORIENTED_EDGE ( 'NONE', *, *, #12794, .T. ) ;
#37150 = DIRECTION ( 'NONE',  ( 0.000000000000000000, 0.000000000000000000, -1.000000000000000000 ) ) ;
#37151 = EDGE_CURVE ( 'NONE', #180, #30647, #4153, .T. ) ;
#37152 = CARTESIAN_POINT ( 'NONE',  ( -1.712991727494380223, 1.205361022782829114E-17, -0.3405009913947248945 ) ) ;
#37153 = CONICAL_SURFACE ( 'NONE', #43711, 2.246510896728926010, 0.01601546068027819014 ) ;
#37154 = DIRECTION ( 'NONE',  ( 0.9959742939952384022, -1.044444007753810152E-17, 0.08963930890344089242 ) ) ;
#37155 = VECTOR ( 'NONE', #581, 39.37007874015748143 ) ;
#37156 = EDGE_CURVE ( 'NONE', #48863, #36721, #20763, .T. ) ;
#37157 = CARTESIAN_POINT ( 'NONE',  ( -1.779568955232875060, 1.574803149606302854, -1.233650562797313555 ) ) ;
#37158 = DIRECTION ( 'NONE',  ( 0.000000000000000000, -1.000000000000000000, 0.000000000000000000 ) ) ;
#37159 = ORIENTED_EDGE ( 'NONE', *, *, #13904, .F. ) ;
#37160 = EDGE_CURVE ( 'NONE', #36720, #43500, #12154, .T. ) ;
#37161 = FACE_OUTER_BOUND ( 'NONE', #34463, .T. ) ;
#37162 = CARTESIAN_POINT ( 'NONE',  ( 0.000000000000000000, 6.692913385826772199, 0.000000000000000000 ) ) ;
#37163 = DIRECTION ( 'NONE',  ( 0.000000000000000000, 1.000000000000000000, 0.000000000000000000 ) ) ;
#37164 = ORIENTED_EDGE ( 'NONE', *, *, #45981, .F. ) ;
#37165 = CARTESIAN_POINT ( 'NONE',  ( -1.181102362204724310, 0.000000000000000000, -1.062992125984252301 ) ) ;
#37166 = VECTOR ( 'NONE', #39694, 39.37007874015748143 ) ;
#37167 = ORIENTED_EDGE ( 'NONE', *, *, #50056, .F. ) ;
#37168 = FACE_OUTER_BOUND ( 'NONE', #1668, .T. ) ;
#37169 = DIRECTION ( 'NONE',  ( -0.000000000000000000, 1.000000000000000000, -0.000000000000000000 ) ) ;
#37170 = DIRECTION ( 'NONE',  ( 1.000000000000000000, -0.000000000000000000, 0.000000000000000000 ) ) ;
#37171 = ADVANCED_FACE ( 'NONE', ( #8792 ), #40034, .T. ) ;
#37172 = LINE ( 'NONE', #13668, #6596 ) ;
#37173 = ORIENTED_EDGE ( 'NONE', *, *, #18099, .T. ) ;
#37174 = ORIENTED_EDGE ( 'NONE', *, *, #22999, .T. ) ;
#37175 = DIRECTION ( 'NONE',  ( 1.000000000000000000, -0.000000000000000000, 0.000000000000000000 ) ) ;
#37176 = LINE ( 'NONE', #5672, #33116 ) ;
#37177 = FACE_BOUND ( 'NONE', #16303, .T. ) ;
#37178 = VERTEX_POINT ( 'NONE', #36167 ) ;
#37179 = EDGE_CURVE ( 'NONE', #45778, #39028, #793, .T. ) ;
#37180 = DIRECTION ( 'NONE',  ( 1.000000000000000000, 0.000000000000000000, 0.000000000000000000 ) ) ;
#37181 = DIRECTION ( 'NONE',  ( 1.000000000000000000, -0.000000000000000000, 0.000000000000000000 ) ) ;
#37182 = VERTEX_POINT ( 'NONE', #25306 ) ;
#37183 = ORIENTED_EDGE ( 'NONE', *, *, #24207, .F. ) ;
#37184 = EDGE_CURVE ( 'NONE', #39803, #24019, #49768, .T. ) ;
#37185 = EDGE_CURVE ( 'NONE', #25804, #6833, #13438, .T. ) ;
#37186 = CARTESIAN_POINT ( 'NONE',  ( -1.909347346926324462, 3.267716535433071279, -0.3543307086614171930 ) ) ;
#37187 = EDGE_CURVE ( 'NONE', #43058, #50549, #18937, .T. ) ;
#37188 = DIRECTION ( 'NONE',  ( -0.000000000000000000, -1.000000000000000000, 0.000000000000000000 ) ) ;
#37189 = ORIENTED_EDGE ( 'NONE', *, *, #33212, .F. ) ;
#37190 = ORIENTED_EDGE ( 'NONE', *, *, #21364, .T. ) ;
#37191 = ORIENTED_EDGE ( 'NONE', *, *, #18412, .F. ) ;
#37192 = FACE_OUTER_BOUND ( 'NONE', #45754, .T. ) ;
#37193 = VECTOR ( 'NONE', #45606, 39.37007874015748143 ) ;
#37194 = CARTESIAN_POINT ( 'NONE',  ( 1.243077785924837197, 0.8677437501918831009, -0.7281234607424009742 ) ) ;
#37195 = VECTOR ( 'NONE', #2504, 39.37007874015748143 ) ;
#37196 = DIRECTION ( 'NONE',  ( -0.3090169943749582204, -0.000000000000000000, 0.9510565162951500895 ) ) ;
#37197 = CARTESIAN_POINT ( 'NONE',  ( -1.325491792074585673, 1.205361022782829114E-17, -2.638988599164751481 ) ) ;
#37198 = VERTEX_POINT ( 'NONE', #29694 ) ;
#37199 = ORIENTED_EDGE ( 'NONE', *, *, #18459, .F. ) ;
#37200 = PLANE ( 'NONE',  #7633 ) ;
#37201 =( CONVERSION_BASED_UNIT ( 'INCH', #41073 ) LENGTH_UNIT ( ) NAMED_UNIT ( #24834 ) );
#37202 = LINE ( 'NONE', #24297, #45566 ) ;
#37203 = VECTOR ( 'NONE', #31127, 39.37007874015748143 ) ;
#37204 = CARTESIAN_POINT ( 'NONE',  ( 1.363819533518803251, 0.000000000000000000, 0.1574803149606283648 ) ) ;
#37205 = LINE ( 'NONE', #5949, #23978 ) ;
#37206 = DIRECTION ( 'NONE',  ( -0.9998717552508122886, -0.01601477604151182316, 0.000000000000000000 ) ) ;
#37207 = DIRECTION ( 'NONE',  ( 1.734723475976806848E-16, 0.000000000000000000, 1.000000000000000000 ) ) ;
#37208 = VERTEX_POINT ( 'NONE', #13696 ) ;
#37209 = DIRECTION ( 'NONE',  ( -1.000000000000000000, 0.000000000000000000, -0.000000000000000000 ) ) ;
#37210 = DIRECTION ( 'NONE',  ( -3.469446951953613696E-16, 0.000000000000000000, -1.000000000000000000 ) ) ;
#37211 = EDGE_LOOP ( 'NONE', ( #35257, #31913, #35611, #29649 ) ) ;
#37212 = ORIENTED_EDGE ( 'NONE', *, *, #38947, .F. ) ;
#37213 = DIRECTION ( 'NONE',  ( -0.000000000000000000, 0.000000000000000000, 1.000000000000000000 ) ) ;
#37214 = LINE ( 'NONE', #25328, #28649 ) ;
#37215 = ADVANCED_FACE ( 'NONE', ( #17316 ), #33585, .F. ) ;
#37216 = EDGE_LOOP ( 'NONE', ( #8372, #21567, #12226, #31833 ) ) ;
#37217 = ADVANCED_FACE ( 'NONE', ( #10076 ), #13160, .F. ) ;
#37218 = EDGE_LOOP ( 'NONE', ( #35957, #29556, #40022, #18475 ) ) ;
#37219 = LINE ( 'NONE', #21721, #4832 ) ;
#37220 = CIRCLE ( 'NONE', #46243, 2.066929133858268042 ) ;
#37221 = ORIENTED_EDGE ( 'NONE', *, *, #8146, .F. ) ;
#37222 = VECTOR ( 'NONE', #21838, 39.37007874015748143 ) ;
#37223 = PLANE ( 'NONE',  #21893 ) ;
#37224 = CARTESIAN_POINT ( 'NONE',  ( -1.439733046521776583, 3.346456692913386100, -0.9448818897637762948 ) ) ;
#37225 = PRESENTATION_LAYER_ASSIGNMENT (  '', '', ( #8357 ) ) ;
#37226 = ORIENTED_EDGE ( 'NONE', *, *, #7215, .F. ) ;
#37227 = ORIENTED_EDGE ( 'NONE', *, *, #35647, .F. ) ;
#37228 = VERTEX_POINT ( 'NONE', #45412 ) ;
#37229 = VECTOR ( 'NONE', #2998, 39.37007874015748143 ) ;
#37230 = DIRECTION ( 'NONE',  ( -1.000000000000000000, -0.000000000000000000, -0.000000000000000000 ) ) ;
#37231 = ORIENTED_EDGE ( 'NONE', *, *, #44017, .T. ) ;
#37232 = VERTEX_POINT ( 'NONE', #25817 ) ;
#37233 = CARTESIAN_POINT ( 'NONE',  ( 0.7423782071083084855, 3.346456692913386100, -1.971134437475891454 ) ) ;
#37234 = CARTESIAN_POINT ( 'NONE',  ( 0.000000000000000000, 3.267716535433071279, 0.000000000000000000 ) ) ;
#37235 = VECTOR ( 'NONE', #1027, 39.37007874015748143 ) ;
#37236 = LINE ( 'NONE', #26363, #7885 ) ;
#37237 = EDGE_CURVE ( 'NONE', #15540, #21218, #29438, .T. ) ;
#37238 = VECTOR ( 'NONE', #24944, 39.37007874015748143 ) ;
#37239 = EDGE_LOOP ( 'NONE', ( #10626, #2501, #35212, #34213 ) ) ;
#37240 = EDGE_CURVE ( 'NONE', #38782, #2547, #33073, .T. ) ;
#37241 = CARTESIAN_POINT ( 'NONE',  ( 2.106197740627112402, 0.000000000000000000, 1.102362204724403938 ) ) ;
#37242 = CARTESIAN_POINT ( 'NONE',  ( -1.166969139818016199, 3.267716535433071279, -1.823990790610291013 ) ) ;
#37243 = CARTESIAN_POINT ( 'NONE',  ( -2.182111253630085290, 3.267716535433071279, 3.785359618865288779E-16 ) ) ;
#37244 = ORIENTED_EDGE ( 'NONE', *, *, #29977, .F. ) ;
#37245 = EDGE_CURVE ( 'NONE', #37726, #27355, #17288, .T. ) ;
#37246 = DIRECTION ( 'NONE',  ( 0.000000000000000000, 0.000000000000000000, -1.000000000000000000 ) ) ;
#37247 = LINE ( 'NONE', #13746, #16999 ) ;
#37248 = EDGE_CURVE ( 'NONE', #12736, #42295, #3271, .T. ) ;
#37249 = FACE_OUTER_BOUND ( 'NONE', #30726, .T. ) ;
#37250 = ORIENTED_EDGE ( 'NONE', *, *, #42928, .T. ) ;
#37251 = EDGE_LOOP ( 'NONE', ( #46142, #3618, #8271 ) ) ;
#37252 = EDGE_CURVE ( 'NONE', #31232, #22619, #6203, .T. ) ;
#37253 = ADVANCED_BREP_SHAPE_REPRESENTATION ( '', ( #41217, #26741 ), #16013 ) ;
#37254 = CARTESIAN_POINT ( 'NONE',  ( 0.7423782071083085965, 3.346456692913386100, -0.5118110236220467790 ) ) ;
#37255 = CARTESIAN_POINT ( 'NONE',  ( -1.391094485341343390, 0.5249441293655172647, 1.667033902411208413 ) ) ;
#37256 = DIRECTION ( 'NONE',  ( 1.734723475976806848E-16, 0.000000000000000000, 1.000000000000000000 ) ) ;
#37257 = ORIENTED_EDGE ( 'NONE', *, *, #47256, .T. ) ;
#37258 = ORIENTED_EDGE ( 'NONE', *, *, #22928, .T. ) ;
#37259 = CARTESIAN_POINT ( 'NONE',  ( -1.645270756471820528, 1.587191622466853413, 1.808365756894092069 ) ) ;
#37260 = ORIENTED_EDGE ( 'NONE', *, *, #30752, .F. ) ;
#37261 = DIRECTION ( 'NONE',  ( 1.000000000000000000, -0.000000000000000000, 0.000000000000000000 ) ) ;
#37262 = LINE ( 'NONE', #14014, #30076 ) ;
#37263 = AXIS2_PLACEMENT_3D ( 'NONE', #22847, #7356, #34974 ) ;
#37264 = VECTOR ( 'NONE', #18186, 39.37007874015748143 ) ;
#37265 = LINE ( 'NONE', #25124, #12675 ) ;
#37266 = CARTESIAN_POINT ( 'NONE',  ( -0.3465944589516569141, 6.692913385826772199, 2.185505870675811035 ) ) ;
#37268 = DIRECTION ( 'NONE',  ( 0.000000000000000000, -1.000000000000000000, 0.000000000000000000 ) ) ;
#37267 = VECTOR ( 'NONE', #12001, 39.37007874015748143 ) ;
#37269 = VERTEX_POINT ( 'NONE', #41067 ) ;
#37270 = CARTESIAN_POINT ( 'NONE',  ( -1.909347346926324906, 3.346456692913386100, -1.102362204724405492 ) ) ;
#37271 = DIRECTION ( 'NONE',  ( 0.000000000000000000, 0.000000000000000000, 1.000000000000000000 ) ) ;
#37272 = AXIS2_PLACEMENT_3D ( 'NONE', #4087, #7694, #11816 ) ;
#37273 = FACE_OUTER_BOUND ( 'NONE', #37401, .T. ) ;
#37274 = VERTEX_POINT ( 'NONE', #14455 ) ;
#37275 = VECTOR ( 'NONE', #25135, 39.37007874015748143 ) ;
#37276 = CARTESIAN_POINT ( 'NONE',  ( -0.8182917201112814842, 3.346456692913386100, 0.5905511811023582691 ) ) ;
#37277 = DIRECTION ( 'NONE',  ( -1.000000000000000000, 0.000000000000000000, -0.000000000000000000 ) ) ;
#37278 = LINE ( 'NONE', #21266, #5689 ) ;
#37279 = ORIENTED_EDGE ( 'NONE', *, *, #38300, .F. ) ;
#37280 = CARTESIAN_POINT ( 'NONE',  ( -1.661821349926435376, 6.692913385826772199, 1.388203579611951621 ) ) ;
#37281 = CARTESIAN_POINT ( 'NONE',  ( 0.000000000000000000, 0.000000000000000000, 0.000000000000000000 ) ) ;
#37282 = ADVANCED_FACE ( 'NONE', ( #21954 ), #6567, .T. ) ;
#37283 = EDGE_CURVE ( 'NONE', #12857, #2160, #2579, .T. ) ;
#37284 = ORIENTED_EDGE ( 'NONE', *, *, #48062, .T. ) ;
#37285 = FACE_OUTER_BOUND ( 'NONE', #31715, .T. ) ;
#37286 = CARTESIAN_POINT ( 'NONE',  ( 0.3382312733057610266, 6.692913385826772199, -2.139420919314966252 ) ) ;
#37287 = VERTEX_POINT ( 'NONE', #41824 ) ;
#37288 = DIRECTION ( 'NONE',  ( -0.4738686624729965269, 0.000000000000000000, -0.8805955318567391110 ) ) ;
#37289 = ADVANCED_FACE ( 'NONE', ( #21440 ), #17565, .F. ) ;
#37290 = LINE ( 'NONE', #41660, #21055 ) ;
#37291 = LINE ( 'NONE', #2164, #34613 ) ;
#37292 = FACE_OUTER_BOUND ( 'NONE', #11684, .T. ) ;
#37293 = CARTESIAN_POINT ( 'NONE',  ( -1.363819533518803473, 3.346456692913386100, 1.535433070866133232 ) ) ;
#37294 = VERTEX_POINT ( 'NONE', #49013 ) ;
#37295 = ORIENTED_EDGE ( 'NONE', *, *, #19697, .T. ) ;
#37296 = DIRECTION ( 'NONE',  ( -1.000000000000000000, 0.000000000000000000, 0.000000000000000000 ) ) ;
#37297 = DIRECTION ( 'NONE',  ( -0.000000000000000000, 1.000000000000000000, -0.000000000000000000 ) ) ;
#37298 = ORIENTED_EDGE ( 'NONE', *, *, #12217, .F. ) ;
#37299 = FACE_OUTER_BOUND ( 'NONE', #4658, .T. ) ;
#37300 = DIRECTION ( 'NONE',  ( 1.000000000000000000, 0.000000000000000000, -3.469446951953613696E-16 ) ) ;
#37301 = DIRECTION ( 'NONE',  ( 1.734723475976806848E-16, -0.000000000000000000, 1.000000000000000000 ) ) ;
#37302 = ORIENTED_EDGE ( 'NONE', *, *, #2595, .T. ) ;
#37303 = VECTOR ( 'NONE', #19431, 39.37007874015748143 ) ;
#37304 = ORIENTED_EDGE ( 'NONE', *, *, #25264, .F. ) ;
#37305 = ADVANCED_FACE ( 'NONE', ( #1562 ), #4121, .T. ) ;
#37306 = CARTESIAN_POINT ( 'NONE',  ( -1.741748233172855320, 0.000000000000000000, -0.08495931630248562683 ) ) ;
#37307 =( BOUNDED_CURVE ( )  B_SPLINE_CURVE ( 3, ( #5693, #37194, #1811, #17561 ),
 .UNSPECIFIED., .F., .F. ) 
 B_SPLINE_CURVE_WITH_KNOTS ( ( 4, 4 ),
 ( 5.526304732732018721, 5.989339700484524798 ),
 .UNSPECIFIED. ) 
 CURVE ( )  GEOMETRIC_REPRESENTATION_ITEM ( )  RATIONAL_B_SPLINE_CURVE ( ( 1.000000000000000000, 0.9822128812423631672, 0.9822128812423631672, 1.000000000000000000 ) ) 
 REPRESENTATION_ITEM ( '' )  );
#37308 = CARTESIAN_POINT ( 'NONE',  ( -1.377952755905510918, 0.000000000000000000, -4.133858267716536083 ) ) ;
#37309 = LINE ( 'NONE', #37562, #12361 ) ;
#37310 = ORIENTED_EDGE ( 'NONE', *, *, #3519, .T. ) ;
#37311 = CARTESIAN_POINT ( 'NONE',  ( -0.8182917201112814842, 3.346456692913386100, 0.7874015748031456541 ) ) ;
#37312 = AXIS2_PLACEMENT_3D ( 'NONE', #21164, #1535, #56 ) ;
#37313 = FACE_BOUND ( 'NONE', #16935, .T. ) ;
#37314 = EDGE_LOOP ( 'NONE', ( #24175, #40219, #28995, #12214 ) ) ;
#37315 = B_SPLINE_CURVE_WITH_KNOTS ( 'NONE', 3,
 ( #43392, #39276, #35158, #27389 ),
 .UNSPECIFIED., .F., .F.,
 ( 4, 4 ),
 ( 2.330467117010365678E-07, 0.01702404298823860518 ),
 .UNSPECIFIED. ) ;
#37316 = ADVANCED_FACE ( 'NONE', ( #9821 ), #5942, .F. ) ;
#37317 = LINE ( 'NONE', #10189, #19953 ) ;
#37318 = ORIENTED_EDGE ( 'NONE', *, *, #14770, .T. ) ;
#37319 = VECTOR ( 'NONE', #18245, 39.37007874015748143 ) ;
#37320 = EDGE_LOOP ( 'NONE', ( #37430, #1286, #39392, #40171 ) ) ;
#37321 = CARTESIAN_POINT ( 'NONE',  ( -2.182111253630085290, 3.346456692913386100, 0.3149606299212578953 ) ) ;
#37322 = CARTESIAN_POINT ( 'NONE',  ( -1.909347346926324906, 3.346456692913386100, -0.8893194486674343979 ) ) ;
#37323 = VECTOR ( 'NONE', #28820, 39.37007874015748143 ) ;
#37324 = ORIENTED_EDGE ( 'NONE', *, *, #38188, .F. ) ;
#37325 = LINE ( 'NONE', #33198, #45058 ) ;
#37326 = DIRECTION ( 'NONE',  ( 0.000000000000000000, 0.000000000000000000, -1.000000000000000000 ) ) ;
#37327 = EDGE_LOOP ( 'NONE', ( #39986, #30284, #34759, #1703 ) ) ;
#37328 = EDGE_CURVE ( 'NONE', #18704, #36771, #17819, .T. ) ;
#37329 = CARTESIAN_POINT ( 'NONE',  ( 1.004206812140325145, 1.632800078982482139, 2.535642212739530610 ) ) ;
#37330 = LINE ( 'NONE', #17699, #14405 ) ;
#37331 = DIRECTION ( 'NONE',  ( -3.469446951953613696E-16, 0.000000000000000000, -1.000000000000000000 ) ) ;
#37332 = CARTESIAN_POINT ( 'NONE',  ( -1.091055626815042645, 0.000000000000000000, -1.141732283464563569 ) ) ;
#37333 = DIRECTION ( 'NONE',  ( 1.283101021437939896E-16, 1.000000000000000000, -1.154811821032073265E-17 ) ) ;
#37334 = ORIENTED_EDGE ( 'NONE', *, *, #21545, .T. ) ;
#37335 = DIRECTION ( 'NONE',  ( -3.469446951953613696E-16, 0.000000000000000000, -1.000000000000000000 ) ) ;
#37336 = DIRECTION ( 'NONE',  ( -0.7071067811865486830, 0.000000000000000000, -0.7071067811865462405 ) ) ;
#37337 = VERTEX_POINT ( 'NONE', #42573 ) ;
#37338 = AXIS2_PLACEMENT_3D ( 'NONE', #15454, #10572, #7207 ) ;
#37339 = CARTESIAN_POINT ( 'NONE',  ( -1.985260859929297572, 0.000000000000000000, -0.3149606299212589500 ) ) ;
#37340 = DIRECTION ( 'NONE',  ( 1.000000000000000000, 0.000000000000000000, 0.000000000000000000 ) ) ;
#37341 = ORIENTED_EDGE ( 'NONE', *, *, #24554, .F. ) ;
#37342 = DIRECTION ( 'NONE',  ( -0.000000000000000000, 1.000000000000000000, -0.000000000000000000 ) ) ;
#37343 = CARTESIAN_POINT ( 'NONE',  ( -1.727163557247779480, 0.000000000000000000, 0.2505061835542949922 ) ) ;
#37344 = CARTESIAN_POINT ( 'NONE',  ( 1.945791886572777685, 0.000000000000000000, -0.8495516078614956390 ) ) ;
#37345 = AXIS2_PLACEMENT_3D ( 'NONE', #11758, #27496, #26986 ) ;
#37346 = EDGE_CURVE ( 'NONE', #32538, #50196, #44803, .T. ) ;
#37347 = ORIENTED_EDGE ( 'NONE', *, *, #35573, .T. ) ;
#37348 = VECTOR ( 'NONE', #15821, 39.37007874015748143 ) ;
#37349 = DIRECTION ( 'NONE',  ( -0.000000000000000000, 1.000000000000000000, -0.000000000000000000 ) ) ;
#37350 = VERTEX_POINT ( 'NONE', #11337 ) ;
#37351 = FACE_BOUND ( 'NONE', #15536, .T. ) ;
#37352 = EDGE_CURVE ( 'NONE', #8873, #35502, #3589, .T. ) ;
#37353 = CARTESIAN_POINT ( 'NONE',  ( 1.015142113812069313, 3.346456692913386100, 0.4724409448818868706 ) ) ;
#37354 = VECTOR ( 'NONE', #37029, 39.37007874015748143 ) ;
#37355 = CARTESIAN_POINT ( 'NONE',  ( -1.439733046521776583, 3.346456692913386100, -0.3149606299212592275 ) ) ;
#37357 = EDGE_CURVE ( 'NONE', #47624, #3690, #46417, .T. ) ;
#37356 = CARTESIAN_POINT ( 'NONE',  ( 0.000000000000000000, 3.267716535433071279, 0.1574803149606283648 ) ) ;
#37358 = EDGE_CURVE ( 'NONE', #5201, #10800, #461, .T. ) ;
#37359 = EDGE_LOOP ( 'NONE', ( #18569, #11617, #48760, #2366 ) ) ;
#37360 = VERTEX_POINT ( 'NONE', #23449 ) ;
#37361 = AXIS2_PLACEMENT_3D ( 'NONE', #37078, #9707, #25443 ) ;
#37362 = CARTESIAN_POINT ( 'NONE',  ( -1.088485032206041980, 1.592042674141829650, 1.917766907668551069 ) ) ;
#37363 = VERTEX_POINT ( 'NONE', #38463 ) ;
#37364 = PLANE ( 'NONE',  #8770 ) ;
#37365 = B_SPLINE_CURVE_WITH_KNOTS ( 'NONE', 3,
 ( #14774, #37771, #50089, #26635 ),
 .UNSPECIFIED., .F., .F.,
 ( 4, 4 ),
 ( 2.472189838406668358E-07, 0.01917498170529582241 ),
 .UNSPECIFIED. ) ;
#37366 = ORIENTED_EDGE ( 'NONE', *, *, #14132, .F. ) ;
#37367 = DIRECTION ( 'NONE',  ( -0.9998717552508122886, -0.01601477604151181275, 0.000000000000000000 ) ) ;
#37368 = EDGE_CURVE ( 'NONE', #13971, #14497, #26571, .T. ) ;
#37369 = ORIENTED_EDGE ( 'NONE', *, *, #43479, .F. ) ;
#37370 = LINE ( 'NONE', #13612, #22478 ) ;
#37371 = CARTESIAN_POINT ( 'NONE',  ( 2.823445274216730638, 5.905511811023623991, 0.8656477926280686797 ) ) ;
#37372 = ORIENTED_EDGE ( 'NONE', *, *, #8243, .F. ) ;
#37373 = EDGE_CURVE ( 'NONE', #24661, #14486, #6956, .T. ) ;
#37374 = CARTESIAN_POINT ( 'NONE',  ( -0.5110942157764869487, 1.711289833164726160, 2.908233010320107059 ) ) ;
#37375 = ORIENTED_EDGE ( 'NONE', *, *, #8273, .T. ) ;
#37376 = VERTEX_POINT ( 'NONE', #11083 ) ;
#37377 = ADVANCED_FACE ( 'NONE', ( #6708 ), #51020, .F. ) ;
#37378 = VERTEX_POINT ( 'NONE', #23200 ) ;
#37379 = VERTEX_POINT ( 'NONE', #22706 ) ;
#37380 = CARTESIAN_POINT ( 'NONE',  ( -1.091055626815042645, 3.346456692913386100, -0.9448818897637760728 ) ) ;
#37381 = VECTOR ( 'NONE', #20457, 39.37007874015748143 ) ;
#37382 = VERTEX_POINT ( 'NONE', #3085 ) ;
#37383 = LINE ( 'NONE', #10257, #13899 ) ;
#37384 = ADVANCED_FACE ( 'NONE', ( #18586 ), #18834, .F. ) ;
#37385 = LINE ( 'NONE', #18255, #34320 ) ;
#37386 = AXIS2_PLACEMENT_3D ( 'NONE', #27631, #7012, #43375 ) ;
#37387 = AXIS2_PLACEMENT_3D ( 'NONE', #13890, #34277, #21890 ) ;
#37388 = CARTESIAN_POINT ( 'NONE',  ( 1.478089240774732582, 0.05159396975604255142, 1.241682111880268558 ) ) ;
#37389 = ORIENTED_EDGE ( 'NONE', *, *, #30970, .T. ) ;
#37390 = FACE_OUTER_BOUND ( 'NONE', #21034, .T. ) ;
#37391 = LINE ( 'NONE', #45859, #22967 ) ;
#37392 = VECTOR ( 'NONE', #35990, 39.37007874015748854 ) ;
#37393 = EDGE_LOOP ( 'NONE', ( #40080, #34355, #28380, #18028 ) ) ;
#37394 = CARTESIAN_POINT ( 'NONE',  ( -0.5455278134075216556, 3.346456692913386100, -2.204724409448810540 ) ) ;
#37395 = DIRECTION ( 'NONE',  ( -0.1342332658176522420, 1.150282676381580509E-16, -0.9909497617679352555 ) ) ;
#37396 = EDGE_CURVE ( 'NONE', #32922, #9737, #30200, .T. ) ;
#37397 = CARTESIAN_POINT ( 'NONE',  ( -1.195183497228115035E-16, 3.346456692913386100, 0.3149606299212576177 ) ) ;
#37398 = CARTESIAN_POINT ( 'NONE',  ( -0.8182917201112819283, 0.000000000000000000, -0.7874015748031467643 ) ) ;
#37399 = LINE ( 'NONE', #28868, #2909 ) ;
#37400 = CARTESIAN_POINT ( 'NONE',  ( -2.001301579076982584, 3.346456692913386100, -0.8267716535433052849 ) ) ;
#37401 = EDGE_LOOP ( 'NONE', ( #21349, #32749, #48006, #34070 ) ) ;
#37402 = DIRECTION ( 'NONE',  ( 0.000000000000000000, 0.000000000000000000, 1.000000000000000000 ) ) ;
#37403 = CARTESIAN_POINT ( 'NONE',  ( -1.531732224425391253, 1.205361022782829114E-17, 0.8801458454442117052 ) ) ;
#37404 = ORIENTED_EDGE ( 'NONE', *, *, #5898, .F. ) ;
#37405 = DIRECTION ( 'NONE',  ( -1.000000000000000000, 0.000000000000000000, 1.734723475976806848E-16 ) ) ;
#37406 = ORIENTED_EDGE ( 'NONE', *, *, #10594, .T. ) ;
#37407 = CARTESIAN_POINT ( 'NONE',  ( -1.636583440222563635, 3.346456692913386100, 1.259842519685033357 ) ) ;
#37408 = ADVANCED_FACE ( 'NONE', ( #7218 ), #23093, .T. ) ;
#37409 = CARTESIAN_POINT ( 'NONE',  ( -0.8238130908517355966, 1.694707076513333410, 2.054984861273213337 ) ) ;
#37410 = CARTESIAN_POINT ( 'NONE',  ( -2.182111253630085290, 3.346456692913386100, 0.1181102362204704270 ) ) ;
#37411 = DIRECTION ( 'NONE',  ( 1.734723475976806848E-16, -0.000000000000000000, 1.000000000000000000 ) ) ;
#37412 = FACE_OUTER_BOUND ( 'NONE', #26434, .T. ) ;
#37413 = ORIENTED_EDGE ( 'NONE', *, *, #4971, .F. ) ;
#37414 = EDGE_CURVE ( 'NONE', #48104, #2922, #3332, .T. ) ;
#37415 = LINE ( 'NONE', #45378, #17543 ) ;
#37416 = VECTOR ( 'NONE', #24848, 39.37007874015748143 ) ;
#37417 = ORIENTED_EDGE ( 'NONE', *, *, #4039, .F. ) ;
#37418 = CARTESIAN_POINT ( 'NONE',  ( -2.120026437385223783, 1.579675233831871806, 1.196720460861670610 ) ) ;
#37419 = ORIENTED_EDGE ( 'NONE', *, *, #27170, .F. ) ;
#37420 = PLANE ( 'NONE',  #39462 ) ;
#37421 = VECTOR ( 'NONE', #3862, 39.37007874015748143 ) ;
#37422 = CARTESIAN_POINT ( 'NONE',  ( 1.759095177328794168, 1.049866565877818125, 1.002495067636045345 ) ) ;
#37423 = ORIENTED_EDGE ( 'NONE', *, *, #32822, .T. ) ;
#37424 = VECTOR ( 'NONE', #47161, 39.37007874015748143 ) ;
#37425 = AXIS2_PLACEMENT_3D ( 'NONE', #5881, #33528, #2267 ) ;
#37426 = CARTESIAN_POINT ( 'NONE',  ( -2.932638728931780125, 1.673548413681422042, 0.3475908556737793420 ) ) ;
#37427 = LINE ( 'NONE', #45388, #22447 ) ;
#37428 = VECTOR ( 'NONE', #38478, 39.37007874015748143 ) ;
#37429 = CARTESIAN_POINT ( 'NONE',  ( 1.052882392248851273, 1.735662962607948057, 2.758708974802636327 ) ) ;
#37430 = ORIENTED_EDGE ( 'NONE', *, *, #41315, .T. ) ;
#37431 = VERTEX_POINT ( 'NONE', #38955 ) ;
#37432 = DIRECTION ( 'NONE',  ( -1.000000000000000000, 0.000000000000000000, 1.734723475976806848E-16 ) ) ;
#37433 = FACE_BOUND ( 'NONE', #20682, .T. ) ;
#37434 = ORIENTED_EDGE ( 'NONE', *, *, #15237, .T. ) ;
#37435 = CARTESIAN_POINT ( 'NONE',  ( -1.442444474601640492, 0.004816277389180329341, -1.011116641508509995 ) ) ;
#37436 = CARTESIAN_POINT ( 'NONE',  ( 1.015142113812069979, 3.346456692913386100, 2.047244094488179567 ) ) ;
#37437 = EDGE_CURVE ( 'NONE', #48050, #39080, #42072, .T. ) ;
#37438 = EDGE_LOOP ( 'NONE', ( #39582, #17369, #46611, #14687 ) ) ;
#37439 = VERTEX_POINT ( 'NONE', #22456 ) ;
#37440 = DIRECTION ( 'NONE',  ( 1.734723475976806848E-16, -0.000000000000000000, 1.000000000000000000 ) ) ;
#37441 = DIRECTION ( 'NONE',  ( 0.000000000000000000, 1.000000000000000000, 0.000000000000000000 ) ) ;
#37442 = ORIENTED_EDGE ( 'NONE', *, *, #34152, .F. ) ;
#37443 = VERTEX_POINT ( 'NONE', #43063 ) ;
#37444 = EDGE_CURVE ( 'NONE', #22025, #16346, #34833, .T. ) ;
#37445 = VERTEX_POINT ( 'NONE', #31214 ) ;
#37446 = CARTESIAN_POINT ( 'NONE',  ( -2.043170538425928662, 3.346456692913386100, -0.5118110236220464460 ) ) ;
#37447 = B_SPLINE_CURVE_WITH_KNOTS ( 'NONE', 3,
 ( #8207, #4327, #16463, #32218 ),
 .UNSPECIFIED., .F., .F.,
 ( 4, 4 ),
 ( 0.01122604379886785533, 0.03073620398351814553 ),
 .UNSPECIFIED. ) ;
#37448 = DIRECTION ( 'NONE',  ( 1.000000000000000000, 0.000000000000000000, 0.000000000000000000 ) ) ;
#37449 = EDGE_CURVE ( 'NONE', #9370, #38459, #46914, .T. ) ;
#37450 = ADVANCED_FACE ( 'NONE', ( #27320 ), #4350, .T. ) ;
#37451 = CARTESIAN_POINT ( 'NONE',  ( 2.017116292511733633, 3.267716535433071279, 0.7874015748031456541 ) ) ;
#37452 = DIRECTION ( 'NONE',  ( 1.000000000000000000, 0.000000000000000000, -3.469446951953613696E-16 ) ) ;
#37453 = EDGE_LOOP ( 'NONE', ( #20540, #45842, #21876, #21906 ) ) ;
#37454 = ORIENTED_EDGE ( 'NONE', *, *, #20793, .F. ) ;
#37455 = CIRCLE ( 'NONE', #20927, 1.850107469027523432 ) ;
#37456 = CARTESIAN_POINT ( 'NONE',  ( -0.1450362469327504955, 6.692913385826772199, -2.160491579385213967 ) ) ;
#37457 = CARTESIAN_POINT ( 'NONE',  ( 0.000000000000000000, 3.267716535433071279, -1.771653543307080581 ) ) ;
#37458 = VECTOR ( 'NONE', #17952, 39.37007874015748143 ) ;
#37459 = CARTESIAN_POINT ( 'NONE',  ( 1.909347346926324462, 0.000000000000000000, -0.7874015748031473194 ) ) ;
#37460 = EDGE_CURVE ( 'NONE', #31646, #49607, #8992, .T. ) ;
#37461 = CONICAL_SURFACE ( 'NONE', #8541, 1.850107469027523210, 0.6386652850508578450 ) ;
#37462 = LINE ( 'NONE', #49019, #30107 ) ;
#37463 = VECTOR ( 'NONE', #6564, 39.37007874015748143 ) ;
#37464 = ADVANCED_FACE ( 'NONE', ( #20609 ), #36363, .F. ) ;
#37465 = LINE ( 'NONE', #49527, #12436 ) ;
#37466 = AXIS2_PLACEMENT_3D ( 'NONE', #50775, #27591, #15222 ) ;
#37467 = DIRECTION ( 'NONE',  ( -3.469446951953613696E-16, 0.000000000000000000, -1.000000000000000000 ) ) ;
#37468 = DIRECTION ( 'NONE',  ( 1.000000000000000000, 0.000000000000000000, 0.000000000000000000 ) ) ;
#37469 = ORIENTED_EDGE ( 'NONE', *, *, #21088, .T. ) ;
#37470 = DIRECTION ( 'NONE',  ( -0.01601477604151182663, 0.9998717552508123996, -0.000000000000000000 ) ) ;
#37471 = FACE_OUTER_BOUND ( 'NONE', #25784, .T. ) ;
#37472 = EDGE_LOOP ( 'NONE', ( #29161, #14246, #13242, #15202 ) ) ;
#37474 = EDGE_CURVE ( 'NONE', #8450, #18246, #32237, .T. ) ;
#37473 = ORIENTED_EDGE ( 'NONE', *, *, #2908, .F. ) ;
#37475 = CARTESIAN_POINT ( 'NONE',  ( 1.015142113812069091, 3.226129038349118794, -2.244094488188969283 ) ) ;
#37476 = ORIENTED_EDGE ( 'NONE', *, *, #37252, .F. ) ;
#37477 = EDGE_CURVE ( 'NONE', #8594, #45509, #986, .T. ) ;
#37478 = EDGE_CURVE ( 'NONE', #9370, #29512, #31721, .T. ) ;
#37479 = ORIENTED_EDGE ( 'NONE', *, *, #26443, .T. ) ;
#37480 = LINE ( 'NONE', #1068, #18832 ) ;
#37481 = VERTEX_POINT ( 'NONE', #15709 ) ;
#37482 = LINE ( 'NONE', #5969, #9510 ) ;
#37483 = DIRECTION ( 'NONE',  ( -0.000000000000000000, 1.000000000000000000, -0.000000000000000000 ) ) ;
#37484 = EDGE_LOOP ( 'NONE', ( #28216, #201, #22321, #8322 ) ) ;
#37485 = VERTEX_POINT ( 'NONE', #598 ) ;
#37486 = ORIENTED_EDGE ( 'NONE', *, *, #19428, .F. ) ;
#37487 = CARTESIAN_POINT ( 'NONE',  ( -0.8182917201112821504, 3.346456692913386100, 1.940849049717691344 ) ) ;
#37488 = VECTOR ( 'NONE', #2898, 39.37007874015748143 ) ;
#37489 = ORIENTED_EDGE ( 'NONE', *, *, #74, .T. ) ;
#37490 = EDGE_LOOP ( 'NONE', ( #35059, #47115, #7512, #379 ) ) ;
#37491 = DIRECTION ( 'NONE',  ( 1.000000000000000000, -0.000000000000000000, 0.000000000000000000 ) ) ;
#37492 = CARTESIAN_POINT ( 'NONE',  ( 0.000000000000000000, 6.692913385826772199, 0.000000000000000000 ) ) ;
#37493 = DIRECTION ( 'NONE',  ( -3.986037398843765983E-20, -1.000000000000000000, -1.160734090543304660E-16 ) ) ;
#37494 = AXIS2_PLACEMENT_3D ( 'NONE', #7928, #19536, #27286 ) ;
#37495 = AXIS2_PLACEMENT_3D ( 'NONE', #29648, #6660, #13647 ) ;
#37496 = VERTEX_POINT ( 'NONE', #12352 ) ;
#37497 = CARTESIAN_POINT ( 'NONE',  ( 0.000000000000000000, 3.267716535433071279, 0.000000000000000000 ) ) ;
#37498 = LINE ( 'NONE', #29737, #37416 ) ;
#37499 = CARTESIAN_POINT ( 'NONE',  ( 1.091055626815042423, 0.000000000000000000, -2.086614173228339641 ) ) ;
#37500 = ORIENTED_EDGE ( 'NONE', *, *, #8525, .T. ) ;
#37501 = PLANE ( 'NONE',  #29026 ) ;
#37502 = LINE ( 'NONE', #18375, #16183 ) ;
#37503 = VECTOR ( 'NONE', #34729, 39.37007874015748143 ) ;
#37504 = CARTESIAN_POINT ( 'NONE',  ( -0.6214413264104945434, 3.267716535433071279, -0.7874015748031467643 ) ) ;
#37505 = ORIENTED_EDGE ( 'NONE', *, *, #5620, .F. ) ;
#37506 = ORIENTED_EDGE ( 'NONE', *, *, #44222, .T. ) ;
#37507 = LINE ( 'NONE', #14250, #6637 ) ;
#37508 = ADVANCED_FACE ( 'NONE', ( #47932 ), #28085, .F. ) ;
#37509 = EDGE_CURVE ( 'NONE', #50129, #29717, #12099, .T. ) ;
#37510 = LINE ( 'NONE', #17878, #588 ) ;
#37511 = DIRECTION ( 'NONE',  ( -1.000000000000000000, -0.000000000000000000, -0.000000000000000000 ) ) ;
#37512 = ORIENTED_EDGE ( 'NONE', *, *, #10755, .F. ) ;
#37514 = EDGE_CURVE ( 'NONE', #2835, #7511, #214, .T. ) ;
#37513 = ORIENTED_EDGE ( 'NONE', *, *, #38395, .F. ) ;
#37515 = CARTESIAN_POINT ( 'NONE',  ( -0.7330548839819540641, 1.630543939889479210, 2.093275022833150700 ) ) ;
#37516 = ORIENTED_EDGE ( 'NONE', *, *, #25354, .T. ) ;
#37517 = CARTESIAN_POINT ( 'NONE',  ( 1.015142113812069313, 3.267716535433071279, -3.521981712565032389E-16 ) ) ;
#37518 = FACE_OUTER_BOUND ( 'NONE', #33793, .T. ) ;
#37519 = LINE ( 'NONE', #45731, #43131 ) ;
#37520 = CARTESIAN_POINT ( 'NONE',  ( 0.000000000000000000, 1.574803149606302854, 0.000000000000000000 ) ) ;
#37521 = DIRECTION ( 'NONE',  ( -0.000000000000000000, 1.000000000000000000, -0.000000000000000000 ) ) ;
#37522 = ORIENTED_EDGE ( 'NONE', *, *, #18585, .T. ) ;
#37523 = VECTOR ( 'NONE', #21194, 39.37007874015748143 ) ;
#37524 = LINE ( 'NONE', #10145, #18443 ) ;
#37525 = CARTESIAN_POINT ( 'NONE',  ( 1.287906020515830141, 3.267716535433071279, -0.8267716535433055070 ) ) ;
#37526 = VECTOR ( 'NONE', #4419, 39.37007874015748143 ) ;
#37527 = ADVANCED_FACE ( 'NONE', ( #8733 ), #39568, .T. ) ;
#37528 = CARTESIAN_POINT ( 'NONE',  ( 0.1968503937007873017, 3.346456692913386100, -0.6299212598425177889 ) ) ;
#37529 = VECTOR ( 'NONE', #23356, 39.37007874015748143 ) ;
#37530 = ORIENTED_EDGE ( 'NONE', *, *, #33519, .F. ) ;
#37531 = PLANE ( 'NONE',  #19084 ) ;
#37532 = EDGE_CURVE ( 'NONE', #24163, #14608, #15963, .T. ) ;
#37533 = CARTESIAN_POINT ( 'NONE',  ( 1.775400203342704764, 1.475394431724762478, -2.359903268218703332 ) ) ;
#37534 = CARTESIAN_POINT ( 'NONE',  ( -0.8942052331142552601, 0.000000000000000000, -0.1968503937007881899 ) ) ;
#37535 = VERTEX_POINT ( 'NONE', #40237 ) ;
#37536 = EDGE_CURVE ( 'NONE', #35361, #43946, #36106, .T. ) ;
#37537 = LINE ( 'NONE', #14030, #25063 ) ;
#37538 = VECTOR ( 'NONE', #12319, 39.37007874015748143 ) ;
#37539 = EDGE_CURVE ( 'NONE', #32210, #30461, #43828, .T. ) ;
#37540 = ORIENTED_EDGE ( 'NONE', *, *, #3252, .F. ) ;
#37541 = CARTESIAN_POINT ( 'NONE',  ( -1.166969139818015977, 3.346456692913386100, -1.417322834645664109 ) ) ;
#37543 = CARTESIAN_POINT ( 'NONE',  ( 2.555365368299595323E-16, 6.692913385826772199, 2.086614173228346303 ) ) ;
#37542 = B_SPLINE_CURVE_WITH_KNOTS ( 'NONE', 3,
 ( #26209, #44793, #9449, #25698 ),
 .UNSPECIFIED., .F., .F.,
 ( 4, 4 ),
 ( 2.767189446683712919E-07, 0.002500421657723224042 ),
 .UNSPECIFIED. ) ;
#37544 = ORIENTED_EDGE ( 'NONE', *, *, #43139, .F. ) ;
#37545 = CARTESIAN_POINT ( 'NONE',  ( -2.823445274216743073, 1.675250974312822105, 0.8656477926280276014 ) ) ;
#37546 = LINE ( 'NONE', #29534, #31731 ) ;
#37547 = PLANE ( 'NONE',  #5720 ) ;
#37548 = CARTESIAN_POINT ( 'NONE',  ( 0.002207914879453961969, 5.905511811023623991, -2.115467123904953617 ) ) ;
#37549 = CARTESIAN_POINT ( 'NONE',  ( 1.287906020515830141, 0.000000000000000000, -0.9448818897637765168 ) ) ;
#37550 = ORIENTED_EDGE ( 'NONE', *, *, #32564, .F. ) ;
#37551 = ORIENTED_EDGE ( 'NONE', *, *, #30595, .T. ) ;
#37552 = CARTESIAN_POINT ( 'NONE',  ( -0.3486774197067340486, 3.267716535433071279, 2.007874015748021268 ) ) ;
#37553 = CARTESIAN_POINT ( 'NONE',  ( -0.5455278134075214336, 3.346456692913386100, 0.3149606299212577287 ) ) ;
#37554 = ORIENTED_EDGE ( 'NONE', *, *, #37156, .F. ) ;
#37555 = DIRECTION ( 'NONE',  ( -0.000000000000000000, 1.000000000000000000, -0.000000000000000000 ) ) ;
#37556 = PLANE ( 'NONE',  #47417 ) ;
#37557 = CARTESIAN_POINT ( 'NONE',  ( -2.182111253630085290, 0.000000000000000000, 0.9448818897637749625 ) ) ;
#37558 = ORIENTED_EDGE ( 'NONE', *, *, #23509, .F. ) ;
#37559 = ORIENTED_EDGE ( 'NONE', *, *, #49346, .F. ) ;
#37560 = LINE ( 'NONE', #1927, #7338 ) ;
#37561 = CARTESIAN_POINT ( 'NONE',  ( -2.055928985459924530, 5.905511811023623991, 0.7197570096327607914 ) ) ;
#37562 = CARTESIAN_POINT ( 'NONE',  ( 1.560669927219590747, 0.000000000000000000, 0.4724409448818871482 ) ) ;
#37563 = ORIENTED_EDGE ( 'NONE', *, *, #12283, .T. ) ;
#37564 = DIRECTION ( 'NONE',  ( 0.000000000000000000, -1.000000000000000000, 0.000000000000000000 ) ) ;
#37565 = CARTESIAN_POINT ( 'NONE',  ( 0.000000000000000000, 3.267716535433071279, 0.3149606299212573401 ) ) ;
#37566 = AXIS2_PLACEMENT_3D ( 'NONE', #11285, #35035, #47109 ) ;
#37567 = ORIENTED_EDGE ( 'NONE', *, *, #24865, .F. ) ;
#37568 = VECTOR ( 'NONE', #516, 39.37007874015748143 ) ;
#37569 = CARTESIAN_POINT ( 'NONE',  ( 2.437180031585944207, 1.205361022782829114E-17, -1.667735833703099413 ) ) ;
#37570 = EDGE_LOOP ( 'NONE', ( #20688, #16688, #14544, #17514 ) ) ;
#37571 = VERTEX_POINT ( 'NONE', #44345 ) ;
#37572 = FACE_OUTER_BOUND ( 'NONE', #24357, .T. ) ;
#37573 = DIRECTION ( 'NONE',  ( 0.000000000000000000, 0.000000000000000000, 1.000000000000000000 ) ) ;
#37574 = VECTOR ( 'NONE', #45437, 39.37007874015748143 ) ;
#37575 = VECTOR ( 'NONE', #37998, 39.37007874015748143 ) ;
#37576 = ORIENTED_EDGE ( 'NONE', *, *, #21251, .F. ) ;
#37577 = CARTESIAN_POINT ( 'NONE',  ( 0.2878729406458415685, 0.5249316497054297148, 1.861923634248271231 ) ) ;
#37578 = LINE ( 'NONE', #2461, #25493 ) ;
#37579 = ORIENTED_EDGE ( 'NONE', *, *, #6125, .F. ) ;
#37580 = EDGE_CURVE ( 'NONE', #24715, #15133, #43578, .T. ) ;
#37581 = AXIS2_PLACEMENT_3D ( 'NONE', #39365, #117, #23357 ) ;
#37582 = EDGE_CURVE ( 'NONE', #7484, #3114, #36618, .T. ) ;
#37583 = DIRECTION ( 'NONE',  ( -0.9998717552508122886, -0.01601477604151182316, 0.000000000000000000 ) ) ;
#37584 = ADVANCED_FACE ( 'NONE', ( #31465 ), #20080, .F. ) ;
#37585 = DIRECTION ( 'NONE',  ( 5.779879058770898378E-18, 1.000000000000000000, 1.286990067732318227E-16 ) ) ;
#37586 = CARTESIAN_POINT ( 'NONE',  ( -2.182111253630085290, 3.226699998040846395, -1.141732283464563791 ) ) ;
#37587 = DIRECTION ( 'NONE',  ( 3.986037398843765983E-20, 1.000000000000000000, 1.160734090543304660E-16 ) ) ;
#37588 = CARTESIAN_POINT ( 'NONE',  ( 1.015142113812069979, 0.000000000000000000, 1.220472440944875281 ) ) ;
#37589 = ORIENTED_EDGE ( 'NONE', *, *, #20316, .F. ) ;
#37590 = DIRECTION ( 'NONE',  ( -7.993605777301125513E-15, 0.000000000000000000, 1.000000000000000000 ) ) ;
#37591 = DIRECTION ( 'NONE',  ( 0.000000000000000000, 0.000000000000000000, -1.000000000000000000 ) ) ;
#37592 = ORIENTED_EDGE ( 'NONE', *, *, #40225, .T. ) ;
#37593 = DIRECTION ( 'NONE',  ( 1.000000000000000000, 0.000000000000000000, 0.000000000000000000 ) ) ;
#37594 = EDGE_CURVE ( 'NONE', #49287, #6252, #39975, .T. ) ;
#37595 = CARTESIAN_POINT ( 'NONE',  ( -2.438548951736694725, 3.267716535433071279, -0.1574803149606298636 ) ) ;
#37596 = ORIENTED_EDGE ( 'NONE', *, *, #15241, .T. ) ;
#37597 = DIRECTION ( 'NONE',  ( -0.000000000000000000, 1.000000000000000000, -0.000000000000000000 ) ) ;
#37598 = DIRECTION ( 'NONE',  ( -3.469446951953613696E-16, 0.000000000000000000, -1.000000000000000000 ) ) ;
#37599 = CARTESIAN_POINT ( 'NONE',  ( 2.734482843737263025, 1.452693199995327644, -1.115254632218672270 ) ) ;
#37600 = VECTOR ( 'NONE', #6538, 39.37007874015748854 ) ;
#37601 = CIRCLE ( 'NONE', #25207, 2.165354330708661568 ) ;
#37602 = EDGE_CURVE ( 'NONE', #13729, #50819, #360, .T. ) ;
#37603 = ORIENTED_EDGE ( 'NONE', *, *, #31937, .F. ) ;
#37604 = FACE_OUTER_BOUND ( 'NONE', #41321, .T. ) ;
#37605 = ORIENTED_EDGE ( 'NONE', *, *, #10433, .T. ) ;
#37606 = DIRECTION ( 'NONE',  ( 0.000000000000000000, 1.000000000000000000, 0.000000000000000000 ) ) ;
#37607 = AXIS2_PLACEMENT_3D ( 'NONE', #13161, #44881, #9535 ) ;
#37608 = CARTESIAN_POINT ( 'NONE',  ( 1.287906020515830585, 3.346456692913386100, 1.889763779527550369 ) ) ;
#37609 = CARTESIAN_POINT ( 'NONE',  ( 0.1067246931122726866, 0.02962905676920215767, 0.000000000000000000 ) ) ;
#37610 = CARTESIAN_POINT ( 'NONE',  ( 1.363819533518803251, 0.000000000000000000, 1.102362204724403938 ) ) ;
#37611 = VECTOR ( 'NONE', #21148, 39.37007874015748143 ) ;
#37612 = AXIS2_PLACEMENT_3D ( 'NONE', #40069, #12439, #36202 ) ;
#37613 = VERTEX_POINT ( 'NONE', #27575 ) ;
#37614 = EDGE_LOOP ( 'NONE', ( #38767, #6186, #3366, #24928 ) ) ;
#37615 = CARTESIAN_POINT ( 'NONE',  ( -2.101391096692225791, 1.575819129783617489, -0.5301069970517552354 ) ) ;
#37616 = EDGE_LOOP ( 'NONE', ( #27645, #48553, #36077, #25406 ) ) ;
#37617 = CARTESIAN_POINT ( 'NONE',  ( 1.636583440222563857, 3.346456692913386100, -0.3149606299212596716 ) ) ;
#37618 = ORIENTED_EDGE ( 'NONE', *, *, #44327, .T. ) ;
#37619 = CARTESIAN_POINT ( 'NONE',  ( 0.000000000000000000, 3.267716535433071279, 0.000000000000000000 ) ) ;
#37620 = ORIENTED_EDGE ( 'NONE', *, *, #16951, .T. ) ;
#37621 = CARTESIAN_POINT ( 'NONE',  ( -1.091055626815042645, 0.000000000000000000, -0.1968503937007881899 ) ) ;
#37622 = LINE ( 'NONE', #6877, #42145 ) ;
#37623 = ORIENTED_EDGE ( 'NONE', *, *, #50380, .F. ) ;
#37624 = PLANE ( 'NONE',  #23208 ) ;
#37625 = ORIENTED_EDGE ( 'NONE', *, *, #47196, .T. ) ;
#37626 = ORIENTED_EDGE ( 'NONE', *, *, #42291, .F. ) ;
#37627 = AXIS2_PLACEMENT_3D ( 'NONE', #39530, #3658, #19892 ) ;
#37628 = ORIENTED_EDGE ( 'NONE', *, *, #46206, .T. ) ;
#37629 = VERTEX_POINT ( 'NONE', #28858 ) ;
#37630 = DIRECTION ( 'NONE',  ( 1.734723475976806848E-16, -0.000000000000000000, 1.000000000000000000 ) ) ;
#37631 = ADVANCED_FACE ( 'NONE', ( #45598 ), #2261, .F. ) ;
#37632 = AXIS2_PLACEMENT_3D ( 'NONE', #24981, #45093, #33767 ) ;
#37633 = EDGE_CURVE ( 'NONE', #15411, #42940, #37643, .T. ) ;
#37634 = AXIS2_PLACEMENT_3D ( 'NONE', #47355, #16683, #12541 ) ;
#37635 = ORIENTED_EDGE ( 'NONE', *, *, #20165, .F. ) ;
#37636 = B_SPLINE_CURVE_WITH_KNOTS ( 'NONE', 3,
 ( #1435, #17191, #43637, #39014 ),
 .UNSPECIFIED., .F., .F.,
 ( 4, 4 ),
 ( 0.001674362740038782627, 0.004174460773670277645 ),
 .UNSPECIFIED. ) ;
#37637 = CARTESIAN_POINT ( 'NONE',  ( 1.387820626701303572, 1.664513642032426466, -1.826445746185616503 ) ) ;
#37638 = CIRCLE ( 'NONE', #33517, 2.165354330708661568 ) ;
#37639 = CARTESIAN_POINT ( 'NONE',  ( -0.07591351300297340121, 3.267716535433071279, -0.9842519685039344823 ) ) ;
#37640 = ADVANCED_FACE ( 'NONE', ( #21378 ), #44847, .F. ) ;
#37641 = VECTOR ( 'NONE', #10036, 39.37007874015748143 ) ;
#37642 = EDGE_CURVE ( 'NONE', #16311, #22056, #47780, .T. ) ;
#37643 = LINE ( 'NONE', #41256, #14036 ) ;
#37644 = VERTEX_POINT ( 'NONE', #41501 ) ;
#37645 = CIRCLE ( 'NONE', #15373, 2.106299212598425008 ) ;
#37646 = CARTESIAN_POINT ( 'NONE',  ( -0.5455278134075208785, 3.346456692913386100, 0.4330708661417290162 ) ) ;
#37647 = LINE ( 'NONE', #42253, #37725 ) ;
#37648 = VERTEX_POINT ( 'NONE', #40745 ) ;
#37649 = CARTESIAN_POINT ( 'NONE',  ( 2.069752515245542046, 1.205361022782829114E-17, -0.5228856972975560735 ) ) ;
#37650 = DIRECTION ( 'NONE',  ( 1.734723475976806848E-16, 0.000000000000000000, 1.000000000000000000 ) ) ;
#37651 = CARTESIAN_POINT ( 'NONE',  ( 2.823445274216730638, 1.664781993127344872, 0.8656477926280681245 ) ) ;
#37652 = LINE ( 'NONE', #45864, #35521 ) ;
#37653 = ORIENTED_EDGE ( 'NONE', *, *, #16866, .T. ) ;
#37654 = CARTESIAN_POINT ( 'NONE',  ( 0.1067246931122726866, 0.02962905676920215767, 0.000000000000000000 ) ) ;
#37655 = EDGE_CURVE ( 'NONE', #10470, #45968, #51042, .T. ) ;
#37656 = DIRECTION ( 'NONE',  ( 0.7818314824680221431, 0.000000000000000000, 0.6234898018587431423 ) ) ;
#37657 = VERTEX_POINT ( 'NONE', #6134 ) ;
#37658 = DIRECTION ( 'NONE',  ( 0.000000000000000000, -1.000000000000000000, 0.000000000000000000 ) ) ;
#37659 = LINE ( 'NONE', #26278, #9446 ) ;
#37660 = ORIENTED_EDGE ( 'NONE', *, *, #34002, .T. ) ;
#37661 = FACE_OUTER_BOUND ( 'NONE', #22629, .T. ) ;
#37662 = B_SPLINE_CURVE_WITH_KNOTS ( 'NONE', 3,
 ( #33584, #15147, #35028, #46602 ),
 .UNSPECIFIED., .F., .F.,
 ( 4, 4 ),
 ( 3.737662051086792397E-07, 0.05012529773801908256 ),
 .UNSPECIFIED. ) ;
#37663 = EDGE_CURVE ( 'NONE', #37629, #33123, #14131, .T. ) ;
#37664 = ORIENTED_EDGE ( 'NONE', *, *, #7952, .T. ) ;
#37665 = CARTESIAN_POINT ( 'NONE',  ( 1.726519710923990480, 1.205361022782829114E-17, -1.198633063221572481 ) ) ;
#37666 = LINE ( 'NONE', #26529, #42366 ) ;
#37667 = FACE_OUTER_BOUND ( 'NONE', #6759, .T. ) ;
#37668 = CARTESIAN_POINT ( 'NONE',  ( -1.833791099076586217, 5.905511811023623991, -1.151507526013721305 ) ) ;
#37669 = DIRECTION ( 'NONE',  ( -0.000000000000000000, 1.000000000000000000, -0.000000000000000000 ) ) ;
#37670 = ORIENTED_EDGE ( 'NONE', *, *, #16268, .F. ) ;
#37671 = EDGE_CURVE ( 'NONE', #38575, #39739, #13630, .T. ) ;
#37672 = VECTOR ( 'NONE', #33785, 39.37007874015748143 ) ;
#37673 = PLANE ( 'NONE',  #207 ) ;
#37674 = VECTOR ( 'NONE', #1747, 39.37007874015748143 ) ;
#37675 = EDGE_LOOP ( 'NONE', ( #8573, #10452, #24524, #30607 ) ) ;
#37676 = VERTEX_POINT ( 'NONE', #33012 ) ;
#37677 = B_SPLINE_CURVE_WITH_KNOTS ( 'NONE', 3,
 ( #307, #21661, #37422, #4952 ),
 .UNSPECIFIED., .F., .F.,
 ( 4, 4 ),
 ( 0.1211873102087489551, 0.1625992483279400380 ),
 .UNSPECIFIED. ) ;
#37678 = CARTESIAN_POINT ( 'NONE',  ( -0.2727639067037608278, 3.346456692913386100, -1.929133858267710000 ) ) ;
#37679 = AXIS2_PLACEMENT_3D ( 'NONE', #44534, #40683, #13572 ) ;
#37680 = ORIENTED_EDGE ( 'NONE', *, *, #24506, .T. ) ;
#37681 = DIRECTION ( 'NONE',  ( -0.000000000000000000, 0.000000000000000000, 1.000000000000000000 ) ) ;
#37682 = CARTESIAN_POINT ( 'NONE',  ( -2.623503965249869729, 0.000000000000000000, 1.355882097269835107 ) ) ;
#37683 = EDGE_CURVE ( 'NONE', #33009, #58, #29631, .T. ) ;
#37684 = VERTEX_POINT ( 'NONE', #9245 ) ;
#37685 = LINE ( 'NONE', #18810, #21492 ) ;
#37686 = CIRCLE ( 'NONE', #15404, 1.181102362204723200 ) ;
#37687 = CARTESIAN_POINT ( 'NONE',  ( -0.6214413264104945434, 3.346456692913386100, -1.102362204724405492 ) ) ;
#37688 = CONICAL_SURFACE ( 'NONE', #26137, 2.165354330708661568, 0.2617993877991570129 ) ;
#37689 = LINE ( 'NONE', #2301, #19759 ) ;
#37690 = ORIENTED_EDGE ( 'NONE', *, *, #1883, .T. ) ;
#37691 = ORIENTED_EDGE ( 'NONE', *, *, #29340, .F. ) ;
#37692 = DIRECTION ( 'NONE',  ( 1.000000000000000000, 0.000000000000000000, 0.000000000000000000 ) ) ;
#37693 = FACE_BOUND ( 'NONE', #24671, .T. ) ;
#37694 = ORIENTED_EDGE ( 'NONE', *, *, #44917, .F. ) ;
#37695 = CARTESIAN_POINT ( 'NONE',  ( -0.7874015748031496509, 0.000000000000000000, -0.7480314960629921295 ) ) ;
#37696 = CARTESIAN_POINT ( 'NONE',  ( -0.2156685157583827228, 5.905511811023623991, -2.945280361644577294 ) ) ;
#37697 = ORIENTED_EDGE ( 'NONE', *, *, #32570, .T. ) ;
#37698 = ORIENTED_EDGE ( 'NONE', *, *, #46725, .F. ) ;
#37699 = LINE ( 'NONE', #21429, #8463 ) ;
#37700 = DIRECTION ( 'NONE',  ( 8.902872254220023478E-17, 1.000000000000000000, -9.311674343991161395E-17 ) ) ;
#37701 = ORIENTED_EDGE ( 'NONE', *, *, #15834, .F. ) ;
#37702 = VERTEX_POINT ( 'NONE', #21882 ) ;
#37703 = VERTEX_POINT ( 'NONE', #29882 ) ;
#37704 = CARTESIAN_POINT ( 'NONE',  ( 0.1968503937007878568, 3.267716535433071279, -6.829619984160672837E-17 ) ) ;
#37705 = EDGE_CURVE ( 'NONE', #32825, #19764, #22141, .T. ) ;
#37706 = DIRECTION ( 'NONE',  ( -1.000000000000000000, -0.000000000000000000, -0.000000000000000000 ) ) ;
#37707 = ADVANCED_FACE ( 'NONE', ( #21626 ), #25247, .F. ) ;
#37709 = CARTESIAN_POINT ( 'NONE',  ( 0.5343643221173207669, 1.723869505195006147, 2.668977133226676290 ) ) ;
#37708 = VECTOR ( 'NONE', #9647, 39.37007874015748854 ) ;
#37710 = EDGE_CURVE ( 'NONE', #50633, #31767, #17000, .T. ) ;
#37711 = DIRECTION ( 'NONE',  ( 0.000000000000000000, 1.000000000000000000, 0.000000000000000000 ) ) ;
#37712 = ORIENTED_EDGE ( 'NONE', *, *, #30207, .F. ) ;
#37713 = ORIENTED_EDGE ( 'NONE', *, *, #21192, .F. ) ;
#37715 = VECTOR ( 'NONE', #36561, 39.37007874015748854 ) ;
#37714 = CARTESIAN_POINT ( 'NONE',  ( -1.166969139818016199, 0.000000000000000000, -1.299212598425192544 ) ) ;
#37716 = LINE ( 'NONE', #37457, #33745 ) ;
#37717 = PLANE ( 'NONE',  #20028 ) ;
#37718 = CARTESIAN_POINT ( 'NONE',  ( -0.4461448448314593307, 1.667947728109364647, 2.182847745222971092 ) ) ;
#37719 = DIRECTION ( 'NONE',  ( -1.000000000000000000, 0.000000000000000000, 0.000000000000000000 ) ) ;
#37720 = CARTESIAN_POINT ( 'NONE',  ( 2.361042194882304379, 3.267716535433071279, 0.6299212598425161236 ) ) ;
#37721 = CARTESIAN_POINT ( 'NONE',  ( 1.560669927219590525, 0.000000000000000000, 0.5905511811023579360 ) ) ;
#37722 = EDGE_LOOP ( 'NONE', ( #10415, #25525, #639, #45108 ) ) ;
#37723 = LINE ( 'NONE', #18850, #26720 ) ;
#37724 = DIRECTION ( 'NONE',  ( -0.000000000000000000, 1.000000000000000000, -0.000000000000000000 ) ) ;
#37725 = VECTOR ( 'NONE', #2263, 39.37007874015748143 ) ;
#37726 = VERTEX_POINT ( 'NONE', #24992 ) ;
#37727 = EDGE_LOOP ( 'NONE', ( #27115, #13649, #36954, #13290 ) ) ;
#37728 = DIRECTION ( 'NONE',  ( -3.469446951953613696E-16, 0.000000000000000000, -1.000000000000000000 ) ) ;
#37729 = ORIENTED_EDGE ( 'NONE', *, *, #7827, .F. ) ;
#37730 = EDGE_CURVE ( 'NONE', #39348, #28725, #32760, .T. ) ;
#37731 = ORIENTED_EDGE ( 'NONE', *, *, #37106, .T. ) ;
#37732 = DIRECTION ( 'NONE',  ( 0.3513748240813304724, 0.000000000000000000, 0.9362348706397417564 ) ) ;
#37733 = EDGE_CURVE ( 'NONE', #19488, #48282, #45097, .T. ) ;
#37734 = ORIENTED_EDGE ( 'NONE', *, *, #19270, .F. ) ;
#37735 = CARTESIAN_POINT ( 'NONE',  ( 1.039905234370930520, 2.755905511811024056, -0.5599999049406324536 ) ) ;
#37736 = DIRECTION ( 'NONE',  ( -1.000000000000000000, -0.000000000000000000, -0.000000000000000000 ) ) ;
#37737 = VECTOR ( 'NONE', #20196, 39.37007874015748143 ) ;
#37738 = AXIS2_PLACEMENT_3D ( 'NONE', #18855, #34606, #26345 ) ;
#37739 = ORIENTED_EDGE ( 'NONE', *, *, #3013, .T. ) ;
#37740 = ORIENTED_EDGE ( 'NONE', *, *, #39136, .T. ) ;
#37741 = DIRECTION ( 'NONE',  ( 0.5407162030609372616, -0.6444004775717706579, 0.5407162030609374836 ) ) ;
#37742 = ORIENTED_EDGE ( 'NONE', *, *, #16470, .T. ) ;
#37743 = VERTEX_POINT ( 'NONE', #17753 ) ;
#37744 = EDGE_CURVE ( 'NONE', #47890, #12778, #21124, .T. ) ;
#37745 = DIRECTION ( 'NONE',  ( 0.000000000000000000, 0.000000000000000000, 1.000000000000000000 ) ) ;
#37746 = CYLINDRICAL_SURFACE ( 'NONE', #31849, 2.952755905511811552 ) ;
#37747 = CARTESIAN_POINT ( 'NONE',  ( -1.439733046521776139, 3.267716535433071279, -4.780733988912460139E-16 ) ) ;
#37748 = AXIS2_PLACEMENT_3D ( 'NONE', #19060, #42559, #42303 ) ;
#37749 = ADVANCED_FACE ( 'NONE', ( #1496 ), #28847, .T. ) ;
#37750 = ORIENTED_EDGE ( 'NONE', *, *, #40225, .F. ) ;
#37751 = CARTESIAN_POINT ( 'NONE',  ( -1.363819533518803029, 3.346456692913386100, 0.9055118110236167750 ) ) ;
#37752 = CARTESIAN_POINT ( 'NONE',  ( 1.530693736245518854, 1.574803149606302854, -1.531579597454043373 ) ) ;
#37753 = CARTESIAN_POINT ( 'NONE',  ( -2.258024766633058622, 3.267716535433071279, -0.03937007874015881204 ) ) ;
#37754 = VERTEX_POINT ( 'NONE', #30391 ) ;
#37755 = CARTESIAN_POINT ( 'NONE',  ( -2.715141060683412100, 0.000000000000000000, -1.160506983230102040 ) ) ;
#37756 = DIRECTION ( 'NONE',  ( 1.734723475976806848E-16, -0.000000000000000000, 1.000000000000000000 ) ) ;
#37757 = DIRECTION ( 'NONE',  ( 1.000000000000000000, 0.000000000000000000, -3.469446951953613696E-16 ) ) ;
#37758 = ORIENTED_EDGE ( 'NONE', *, *, #35590, .F. ) ;
#37759 = ORIENTED_EDGE ( 'NONE', *, *, #50874, .T. ) ;
#37760 = EDGE_CURVE ( 'NONE', #34814, #23582, #22894, .T. ) ;
#37761 = DIRECTION ( 'NONE',  ( -3.469446951953613696E-16, 0.000000000000000000, -1.000000000000000000 ) ) ;
#37762 = CARTESIAN_POINT ( 'NONE',  ( 0.000000000000000000, 3.267716535433071279, 1.574803149606291974 ) ) ;
#37763 = EDGE_CURVE ( 'NONE', #41844, #45206, #31150, .T. ) ;
#37764 = EDGE_CURVE ( 'NONE', #13212, #9488, #21322, .T. ) ;
#37765 = DIRECTION ( 'NONE',  ( 0.08963930890342654279, 0.000000000000000000, 0.9959742939952397345 ) ) ;
#37766 = ORIENTED_EDGE ( 'NONE', *, *, #4932, .T. ) ;
#37767 = ORIENTED_EDGE ( 'NONE', *, *, #2017, .T. ) ;
#37768 = EDGE_CURVE ( 'NONE', #17591, #38922, #19012, .T. ) ;
#37769 = CARTESIAN_POINT ( 'NONE',  ( 3.927031490892378253E-16, 0.000000000000000000, 1.377952755905504256 ) ) ;
#37770 = EDGE_LOOP ( 'NONE', ( #27095, #49484, #31785, #47816 ) ) ;
#37771 = CARTESIAN_POINT ( 'NONE',  ( -1.547867290569560961, 1.691170706622086017, -2.214182027291666355 ) ) ;
#37772 = CARTESIAN_POINT ( 'NONE',  ( -0.07591351300297277671, 0.000000000000000000, 2.047244094488179567 ) ) ;
#37773 = AXIS2_PLACEMENT_3D ( 'NONE', #39619, #19731, #19478 ) ;
#37774 = AXIS2_PLACEMENT_3D ( 'NONE', #38174, #46379, #42535 ) ;
#37775 = CARTESIAN_POINT ( 'NONE',  ( 1.695772546416037363, 1.477242674555747426, -2.417756147381349141 ) ) ;
#37776 = PLANE ( 'NONE',  #40901 ) ;
#37777 = DIRECTION ( 'NONE',  ( 0.000000000000000000, 0.000000000000000000, -1.000000000000000000 ) ) ;
#37778 = ORIENTED_EDGE ( 'NONE', *, *, #7887, .T. ) ;
#37779 = CARTESIAN_POINT ( 'NONE',  ( 0.000000000000000000, 6.692913385826772199, 0.000000000000000000 ) ) ;
#37780 = CARTESIAN_POINT ( 'NONE',  ( 1.557927422371225612, 0.000000000000000000, 0.7824709080581413456 ) ) ;
#37781 = VECTOR ( 'NONE', #41302, 39.37007874015748143 ) ;
#37782 = DIRECTION ( 'NONE',  ( -1.000000000000000000, -0.000000000000000000, -0.000000000000000000 ) ) ;
#37783 = EDGE_LOOP ( 'NONE', ( #24893, #27738, #38348, #13237 ) ) ;
#37785 = CARTESIAN_POINT ( 'NONE',  ( 0.08119777152254364916, 1.623385212329073957, 0.000000000000000000 ) ) ;
#37784 = VECTOR ( 'NONE', #34670, 39.37007874015748143 ) ;
#37786 = CARTESIAN_POINT ( 'NONE',  ( 2.182111253630085290, 0.000000000000000000, 0.3149606299212573401 ) ) ;
#37787 = PLANE ( 'NONE',  #2405 ) ;
#37788 = VERTEX_POINT ( 'NONE', #15406 ) ;
#37789 = EDGE_CURVE ( 'NONE', #4458, #37754, #38892, .T. ) ;
#37790 = VECTOR ( 'NONE', #23192, 39.37007874015748143 ) ;
#37791 = DIRECTION ( 'NONE',  ( 0.000000000000000000, 0.000000000000000000, -1.000000000000000000 ) ) ;
#37792 = ORIENTED_EDGE ( 'NONE', *, *, #26253, .F. ) ;
#37793 = DIRECTION ( 'NONE',  ( -1.000000000000000000, 0.000000000000000000, -0.000000000000000000 ) ) ;
#37794 = LINE ( 'NONE', #30033, #47976 ) ;
#37795 = ORIENTED_EDGE ( 'NONE', *, *, #44980, .T. ) ;
#37796 = AXIS2_PLACEMENT_3D ( 'NONE', #6273, #29247, #45733 ) ;
#37797 = CARTESIAN_POINT ( 'NONE',  ( 0.2727639067037604392, 3.267716535433071279, 0.2755905511810994302 ) ) ;
#37798 = EDGE_CURVE ( 'NONE', #44880, #41924, #7650, .T. ) ;
#37799 = CARTESIAN_POINT ( 'NONE',  ( 1.287906020515829919, 0.000000000000000000, -1.259842519685035134 ) ) ;
#37800 = LINE ( 'NONE', #2425, #12378 ) ;
#37801 = LINE ( 'NONE', #14039, #16938 ) ;
#37802 = EDGE_CURVE ( 'NONE', #31344, #37886, #3024, .T. ) ;
#37803 = EDGE_CURVE ( 'NONE', #50692, #6941, #7405, .T. ) ;
#37804 = ORIENTED_EDGE ( 'NONE', *, *, #29170, .T. ) ;
#37805 = ORIENTED_EDGE ( 'NONE', *, *, #10975, .F. ) ;
#37806 = DIRECTION ( 'NONE',  ( 1.734723475976806848E-16, -0.000000000000000000, 1.000000000000000000 ) ) ;
#37807 = DIRECTION ( 'NONE',  ( 1.000000000000000000, 0.000000000000000000, -3.469446951953613696E-16 ) ) ;
#37808 = ORIENTED_EDGE ( 'NONE', *, *, #27878, .F. ) ;
#37809 = CARTESIAN_POINT ( 'NONE',  ( -2.362204724409450396, 1.172985819482486924, 1.181102362204724088 ) ) ;
#37810 = LINE ( 'NONE', #22052, #5492 ) ;
#37811 = FACE_OUTER_BOUND ( 'NONE', #19373, .T. ) ;
#37812 = ORIENTED_EDGE ( 'NONE', *, *, #7138, .F. ) ;
#37813 = ORIENTED_EDGE ( 'NONE', *, *, #39675, .F. ) ;
#37814 = FACE_OUTER_BOUND ( 'NONE', #39446, .T. ) ;
#37815 = CARTESIAN_POINT ( 'NONE',  ( 2.182111253630085290, 3.267716535433071279, -1.161035397307311917E-15 ) ) ;
#37816 = AXIS2_PLACEMENT_3D ( 'NONE', #38183, #35058, #26541 ) ;
#37817 = DIRECTION ( 'NONE',  ( -3.469446951953613696E-16, 0.000000000000000000, -1.000000000000000000 ) ) ;
#37818 = EDGE_CURVE ( 'NONE', #48094, #32722, #46857, .T. ) ;
#37819 = ORIENTED_EDGE ( 'NONE', *, *, #27211, .F. ) ;
#37820 = CARTESIAN_POINT ( 'NONE',  ( 0.000000000000000000, 2.755905511811024056, 0.000000000000000000 ) ) ;
#37821 = CARTESIAN_POINT ( 'NONE',  ( -1.363819533518803473, 3.267716535433071279, -1.732283464566922726 ) ) ;
#37822 = EDGE_LOOP ( 'NONE', ( #15179, #21834, #21212, #45159, #14062, #35229, #24459, #12530, #37102, #47087, #39158, #28755, #16754, #41658, #7620, #43090, #49987, #23632, #44266, #16913, #3611, #26150, #4773, #10100, #42201, #2951, #301, #25872, #45456, #48976, #33256, #39699, #26891, #28503, #43198, #42819, #27149, #595, #5294, #36877, #30510, #49613, #50468, #13208, #20918, #40880, #32809, #27494, #27430, #50988, #28305, #40027, #15938, #25532, #17035, #39253, #40216, #20958, #8348, #36319, #11935, #14072, #17744, #42912, #45429, #21600, #45170, #10598, #29824, #206, #18233, #8981, #29264, #6403, #27996, #49184 ) ) ;
#37823 = CARTESIAN_POINT ( 'NONE',  ( 0.5756566573088583993, 1.629780628454260194, 2.896516654582643291 ) ) ;
#37824 = ORIENTED_EDGE ( 'NONE', *, *, #12904, .F. ) ;
#37826 = ORIENTED_EDGE ( 'NONE', *, *, #9890, .F. ) ;
#37825 = VECTOR ( 'NONE', #12083, 39.37007874015748143 ) ;
#37827 = EDGE_CURVE ( 'NONE', #17626, #31910, #23132, .T. ) ;
#37828 = DIRECTION ( 'NONE',  ( 1.000000000000000000, 0.000000000000000000, 0.000000000000000000 ) ) ;
#37829 = DIRECTION ( 'NONE',  ( 1.000000000000000000, 0.000000000000000000, -3.469446951953613696E-16 ) ) ;
#37830 = CIRCLE ( 'NONE', #32027, 2.244934639244525076 ) ;
#37831 = VECTOR ( 'NONE', #46390, 39.37007874015748143 ) ;
#37832 = PLANE ( 'NONE',  #42082 ) ;
#37833 = EDGE_LOOP ( 'NONE', ( #42062, #24610, #32173, #24984 ) ) ;
#37834 = CARTESIAN_POINT ( 'NONE',  ( -2.454875160333845674, 3.245198442041970832, 0.02684680494028401573 ) ) ;
#37835 = EDGE_CURVE ( 'NONE', #11648, #1706, #39772, .T. ) ;
#37836 = EDGE_CURVE ( 'NONE', #2302, #35717, #46108, .T. ) ;
#37838 = LINE ( 'NONE', #41947, #13123 ) ;
#37837 = VECTOR ( 'NONE', #41253, 39.37007874015748143 ) ;
#37839 = ORIENTED_EDGE ( 'NONE', *, *, #1820, .T. ) ;
#37840 = ADVANCED_FACE ( 'NONE', ( #27005 ), #30643, .F. ) ;
#37841 = VECTOR ( 'NONE', #6086, 39.37007874015748143 ) ;
#37842 = VERTEX_POINT ( 'NONE', #3526 ) ;
#37843 = DIRECTION ( 'NONE',  ( -8.032339854997460071E-17, 1.000000000000000000, 1.007223559679395367E-16 ) ) ;
#37844 = CARTESIAN_POINT ( 'NONE',  ( 0.4788131938641111973, 1.504819983455083277, 2.914091152102192162 ) ) ;
#37845 = AXIS2_PLACEMENT_3D ( 'NONE', #44593, #9249, #5372 ) ;
#37846 = PLANE ( 'NONE',  #2540 ) ;
#37847 = CARTESIAN_POINT ( 'NONE',  ( -1.091055626815042201, 0.000000000000000000, 1.259842519685033357 ) ) ;
#37848 = LINE ( 'NONE', #25192, #34439 ) ;
#37849 = ORIENTED_EDGE ( 'NONE', *, *, #41563, .F. ) ;
#37850 = CARTESIAN_POINT ( 'NONE',  ( -1.166969139818015533, 3.346456692913386100, 0.7874015748031456541 ) ) ;
#37851 = DIRECTION ( 'NONE',  ( -0.000000000000000000, 1.000000000000000000, -0.000000000000000000 ) ) ;
#37852 = ORIENTED_EDGE ( 'NONE', *, *, #28463, .F. ) ;
#37853 = DIRECTION ( 'NONE',  ( -3.469446951953613696E-16, 0.000000000000000000, -1.000000000000000000 ) ) ;
#37854 = DIRECTION ( 'NONE',  ( -3.469446951953613696E-16, 0.000000000000000000, -1.000000000000000000 ) ) ;
#37855 = ORIENTED_EDGE ( 'NONE', *, *, #26504, .T. ) ;
#37856 = DIRECTION ( 'NONE',  ( -0.000000000000000000, 0.000000000000000000, 1.000000000000000000 ) ) ;
#37857 = AXIS2_PLACEMENT_3D ( 'NONE', #21601, #9474, #40979 ) ;
#37858 = DIRECTION ( 'NONE',  ( -0.000000000000000000, 1.000000000000000000, -0.000000000000000000 ) ) ;
#37859 = LINE ( 'NONE', #49166, #16961 ) ;
#37860 = B_SPLINE_CURVE_WITH_KNOTS ( 'NONE', 3,
 ( #46044, #37834, #42442, #42935 ),
 .UNSPECIFIED., .F., .F.,
 ( 4, 4 ),
 ( 0.02645197609580694081, 0.03146547178533463940 ),
 .UNSPECIFIED. ) ;
#37861 = ORIENTED_EDGE ( 'NONE', *, *, #38319, .F. ) ;
#37862 = CARTESIAN_POINT ( 'NONE',  ( 2.949782676795221992, 0.000000000000000000, -0.1324748927672375898 ) ) ;
#37863 = EDGE_LOOP ( 'NONE', ( #2937, #29569, #14189 ) ) ;
#37864 = FACE_BOUND ( 'NONE', #41272, .T. ) ;
#37865 = DIRECTION ( 'NONE',  ( 1.734723475976806848E-16, -0.000000000000000000, 1.000000000000000000 ) ) ;
#37866 = VECTOR ( 'NONE', #30247, 39.37007874015748143 ) ;
#37867 = VECTOR ( 'NONE', #18198, 39.37007874015748143 ) ;
#37868 = DIRECTION ( 'NONE',  ( 1.000000000000000000, 0.000000000000000000, 0.000000000000000000 ) ) ;
#37869 = DIRECTION ( 'NONE',  ( 1.042246309068005903E-16, 1.000000000000000000, -7.572362681945165783E-17 ) ) ;
#37870 = EDGE_CURVE ( 'NONE', #21120, #24910, #28708, .T. ) ;
#37871 = AXIS2_PLACEMENT_3D ( 'NONE', #8539, #797, #48253 ) ;
#37872 = EDGE_CURVE ( 'NONE', #13698, #37269, #45856, .T. ) ;
#37873 = VERTEX_POINT ( 'NONE', #3272 ) ;
#37874 = ORIENTED_EDGE ( 'NONE', *, *, #44543, .F. ) ;
#37875 = DIRECTION ( 'NONE',  ( 1.734723475976806848E-16, -0.000000000000000000, 1.000000000000000000 ) ) ;
#37876 = AXIS2_PLACEMENT_3D ( 'NONE', #31359, #14856, #38852 ) ;
#37877 = CARTESIAN_POINT ( 'NONE',  ( 1.091055626815042645, 0.000000000000000000, -0.8267716535433055070 ) ) ;
#37878 = ORIENTED_EDGE ( 'NONE', *, *, #14365, .T. ) ;
#37879 = DIRECTION ( 'NONE',  ( 1.000000000000000000, 0.000000000000000000, 0.000000000000000000 ) ) ;
#37880 = ORIENTED_EDGE ( 'NONE', *, *, #21830, .T. ) ;
#37881 = CARTESIAN_POINT ( 'NONE',  ( 1.909347346926324684, 0.000000000000000000, 0.4724409448818868706 ) ) ;
#37882 = DIRECTION ( 'NONE',  ( -3.469446951953613696E-16, 0.000000000000000000, -1.000000000000000000 ) ) ;
#37883 = ORIENTED_EDGE ( 'NONE', *, *, #15879, .T. ) ;
#37884 = LINE ( 'NONE', #17993, #41433 ) ;
#37885 = ORIENTED_EDGE ( 'NONE', *, *, #27896, .F. ) ;
#37886 = VERTEX_POINT ( 'NONE', #42009 ) ;
#37887 = EDGE_CURVE ( 'NONE', #26436, #24660, #10765, .T. ) ;
#37888 = ADVANCED_FACE ( 'NONE', ( #6647 ), #15149, .F. ) ;
#37889 = AXIS2_PLACEMENT_3D ( 'NONE', #35950, #578, #23056 ) ;
#37890 = VERTEX_POINT ( 'NONE', #36306 ) ;
#37891 = ORIENTED_EDGE ( 'NONE', *, *, #49068, .F. ) ;
#37892 = LINE ( 'NONE', #44584, #17029 ) ;
#37893 = EDGE_CURVE ( 'NONE', #17882, #14542, #31404, .T. ) ;
#37894 = ORIENTED_EDGE ( 'NONE', *, *, #43886, .T. ) ;
#37895 = DIRECTION ( 'NONE',  ( -3.469446951953613696E-16, 0.000000000000000000, -1.000000000000000000 ) ) ;
#37896 = CARTESIAN_POINT ( 'NONE',  ( -1.733526556417524622, 0.000000000000000000, 0.1851600754179555941 ) ) ;
#37897 = VECTOR ( 'NONE', #33834, 39.37007874015748143 ) ;
#37898 = CARTESIAN_POINT ( 'NONE',  ( -1.735432873265435161, 1.581680620477750931, 1.321016258651915409 ) ) ;
#37899 = VECTOR ( 'NONE', #27986, 39.37007874015748143 ) ;
#37900 = DIRECTION ( 'NONE',  ( -0.4738686624729965269, 1.022326139627305519E-16, -0.8805955318567391110 ) ) ;
#37901 = CARTESIAN_POINT ( 'NONE',  ( -0.2304536187657762192, 1.049866565067838264, -2.011542525589492758 ) ) ;
#37902 = ORIENTED_EDGE ( 'NONE', *, *, #35483, .T. ) ;
#37903 = LINE ( 'NONE', #34023, #7631 ) ;
#37904 = CARTESIAN_POINT ( 'NONE',  ( -2.182111253630085290, 3.346456692913386100, 0.3149606299212578953 ) ) ;
#37905 = AXIS2_PLACEMENT_3D ( 'NONE', #45502, #9915, #14038 ) ;
#37906 = CARTESIAN_POINT ( 'NONE',  ( -1.312623452344869657, 1.205361022782829114E-17, 1.722945714930904648 ) ) ;
#37907 = DIRECTION ( 'NONE',  ( -0.000000000000000000, 1.000000000000000000, -0.000000000000000000 ) ) ;
#37908 = ORIENTED_EDGE ( 'NONE', *, *, #44054, .F. ) ;
#37909 = DIRECTION ( 'NONE',  ( -1.000000000000000000, 0.000000000000000000, 1.734723475976806848E-16 ) ) ;
#37910 = CARTESIAN_POINT ( 'NONE',  ( -0.8182917201112814842, 3.346456692913386100, 1.535433070866133898 ) ) ;
#37911 = ORIENTED_EDGE ( 'NONE', *, *, #49103, .F. ) ;
#37912 = DIRECTION ( 'NONE',  ( 0.8345732537213079727, 0.000000000000000000, -0.5508969814520945363 ) ) ;
#37913 = LINE ( 'NONE', #48959, #49782 ) ;
#37914 = ORIENTED_EDGE ( 'NONE', *, *, #42839, .F. ) ;
#37915 = ORIENTED_EDGE ( 'NONE', *, *, #2705, .F. ) ;
#37916 = DIRECTION ( 'NONE',  ( 0.9639628606958511314, 0.000000000000000000, 0.2660368455666826115 ) ) ;
#37917 = CARTESIAN_POINT ( 'NONE',  ( -1.547009873100170907, 1.617506960006209527, -1.547179421581643011 ) ) ;
#37918 = CARTESIAN_POINT ( 'NONE',  ( 1.636583440222563857, 3.346456692913386100, 1.062992125984245639 ) ) ;
#37919 = LINE ( 'NONE', #9784, #18509 ) ;
#37920 = CARTESIAN_POINT ( 'NONE',  ( 2.099568260077706583, 1.574803149606302854, -0.5296909464895790398 ) ) ;
#37921 = VECTOR ( 'NONE', #49496, 39.37007874015748143 ) ;
#37922 = EDGE_LOOP ( 'NONE', ( #16003, #43592, #46723, #31477 ) ) ;
#37923 = CARTESIAN_POINT ( 'NONE',  ( 2.106197740627111514, 3.267716535433071279, -0.7874015748031473194 ) ) ;
#37924 = ADVANCED_FACE ( 'NONE', ( #3783 ), #47104, .F. ) ;
#37925 = ORIENTED_EDGE ( 'NONE', *, *, #31290, .F. ) ;
#37926 = ORIENTED_EDGE ( 'NONE', *, *, #23845, .T. ) ;
#37927 = EDGE_CURVE ( 'NONE', #32172, #42867, #40179, .T. ) ;
#37928 = CARTESIAN_POINT ( 'NONE',  ( -1.091055626815042645, 3.267716535433071279, -1.456692913385822186 ) ) ;
#37929 = ORIENTED_EDGE ( 'NONE', *, *, #26502, .T. ) ;
#37930 = CARTESIAN_POINT ( 'NONE',  ( 0.000000000000000000, 3.267716535433071279, -0.6692913385826764205 ) ) ;
#37931 = FACE_OUTER_BOUND ( 'NONE', #46525, .T. ) ;
#37932 = ORIENTED_EDGE ( 'NONE', *, *, #20802, .F. ) ;
#37933 = EDGE_CURVE ( 'NONE', #26292, #27844, #33877, .T. ) ;
#37934 = AXIS2_PLACEMENT_3D ( 'NONE', #5875, #37131, #13883 ) ;
#37935 = DIRECTION ( 'NONE',  ( 0.1342332658176667304, 1.288287287306305530E-16, -0.9909497617679332571 ) ) ;
#37936 = DIRECTION ( 'NONE',  ( -3.469446951953613696E-16, 0.000000000000000000, -1.000000000000000000 ) ) ;
#37937 = EDGE_CURVE ( 'NONE', #47433, #35962, #674, .T. ) ;
#37938 = DIRECTION ( 'NONE',  ( -8.653332088726061579E-16, 0.7071067811865483499, -0.7071067811865466846 ) ) ;
#37939 = ORIENTED_EDGE ( 'NONE', *, *, #4929, .T. ) ;
#37940 = ORIENTED_EDGE ( 'NONE', *, *, #7683, .T. ) ;
#37941 = CARTESIAN_POINT ( 'NONE',  ( 0.1736737122991879045, 1.616004489590360693, -2.478679879797507368 ) ) ;
#37942 = FACE_BOUND ( 'NONE', #16533, .T. ) ;
#37943 = ORIENTED_EDGE ( 'NONE', *, *, #8526, .T. ) ;
#37944 = VECTOR ( 'NONE', #37483, 39.37007874015748143 ) ;
#37945 = PLANE ( 'NONE',  #32814 ) ;
#37946 = ADVANCED_FACE ( 'NONE', ( #43769 ), #23912, .F. ) ;
#37947 = FACE_OUTER_BOUND ( 'NONE', #15912, .T. ) ;
#37948 = VERTEX_POINT ( 'NONE', #4804 ) ;
#37949 = EDGE_LOOP ( 'NONE', ( #1806, #45274, #25022, #12146 ) ) ;
#37950 = CARTESIAN_POINT ( 'NONE',  ( 0.000000000000000000, 3.267716535433071279, -0.1574803149606298636 ) ) ;
#37951 = DIRECTION ( 'NONE',  ( 1.734723475976806848E-16, -0.000000000000000000, 1.000000000000000000 ) ) ;
#37952 = EDGE_CURVE ( 'NONE', #14507, #25804, #930, .T. ) ;
#37953 = ORIENTED_EDGE ( 'NONE', *, *, #15427, .T. ) ;
#37954 = ORIENTED_EDGE ( 'NONE', *, *, #531, .F. ) ;
#37955 = ORIENTED_EDGE ( 'NONE', *, *, #40546, .T. ) ;
#37956 = FACE_OUTER_BOUND ( 'NONE', #36926, .T. ) ;
#37957 = DIRECTION ( 'NONE',  ( 0.000000000000000000, -1.000000000000000000, 0.000000000000000000 ) ) ;
#37958 = DIRECTION ( 'NONE',  ( 0.000000000000000000, -0.000000000000000000, 1.000000000000000000 ) ) ;
#37959 = CARTESIAN_POINT ( 'NONE',  ( 0.8182917201112819283, 0.000000000000000000, 1.102362204724403938 ) ) ;
#37960 = ORIENTED_EDGE ( 'NONE', *, *, #29307, .F. ) ;
#37961 = VERTEX_POINT ( 'NONE', #19516 ) ;
#37962 = CARTESIAN_POINT ( 'NONE',  ( -0.7331725592709618100, 1.597733653658881758, 2.093588567519426569 ) ) ;
#37963 = DIRECTION ( 'NONE',  ( -0.9998717552508122886, -0.01601477604151180928, 0.000000000000000000 ) ) ;
#37964 = LINE ( 'NONE', #34087, #22517 ) ;
#37965 = EDGE_CURVE ( 'NONE', #24641, #37788, #4549, .T. ) ;
#37966 = DIRECTION ( 'NONE',  ( 0.6910626489868580968, 0.000000000000000000, 0.7227948638273978821 ) ) ;
#37967 = CARTESIAN_POINT ( 'NONE',  ( -0.6734335508564485151, 1.704902552214879963, -2.625115814727751129 ) ) ;
#37968 = B_SPLINE_CURVE_WITH_KNOTS ( 'NONE', 3,
 ( #41064, #49764, #21435, #17813 ),
 .UNSPECIFIED., .F., .F.,
 ( 4, 4 ),
 ( 0.001800744595756896896, 0.004300762518479772645 ),
 .UNSPECIFIED. ) ;
#37969 = AXIS2_PLACEMENT_3D ( 'NONE', #43895, #24300, #40041 ) ;
#37970 = VECTOR ( 'NONE', #32358, 39.37007874015748143 ) ;
#37971 = DIRECTION ( 'NONE',  ( -3.986037398843765983E-20, -1.000000000000000000, -1.160734090543304660E-16 ) ) ;
#37972 = DIRECTION ( 'NONE',  ( -0.9998717552508122886, -0.01601477604151180928, 0.000000000000000000 ) ) ;
#37973 = ORIENTED_EDGE ( 'NONE', *, *, #32454, .F. ) ;
#37974 = CARTESIAN_POINT ( 'NONE',  ( -0.8942052331142552601, 3.346456692913386100, -1.259842519685034690 ) ) ;
#37975 = PLANE ( 'NONE',  #43382 ) ;
#37976 = VECTOR ( 'NONE', #38190, 39.37007874015748143 ) ;
#37977 = ORIENTED_EDGE ( 'NONE', *, *, #20469, .F. ) ;
#37978 = ORIENTED_EDGE ( 'NONE', *, *, #22288, .F. ) ;
#37979 = DIRECTION ( 'NONE',  ( 1.000000000000000000, -0.000000000000000000, 0.000000000000000000 ) ) ;
#37980 = ORIENTED_EDGE ( 'NONE', *, *, #1881, .T. ) ;
#37981 = EDGE_CURVE ( 'NONE', #36589, #48375, #31662, .T. ) ;
#37982 = ORIENTED_EDGE ( 'NONE', *, *, #6593, .T. ) ;
#37983 = DIRECTION ( 'NONE',  ( -0.000000000000000000, 1.000000000000000000, -0.000000000000000000 ) ) ;
#37984 = ORIENTED_EDGE ( 'NONE', *, *, #34263, .T. ) ;
#37985 = ADVANCED_FACE ( 'NONE', ( #8423 ), #39659, .F. ) ;
#37986 = DIRECTION ( 'NONE',  ( -2.582876339026174526E-17, -1.000000000000000000, -1.131632063491654496E-16 ) ) ;
#37987 = LINE ( 'NONE', #25847, #51048 ) ;
#37988 = ADVANCED_FACE ( 'NONE', ( #16685 ), #32438, .F. ) ;
#37989 = ADVANCED_FACE ( 'NONE', ( #31928 ), #44292, .F. ) ;
#37990 = ORIENTED_EDGE ( 'NONE', *, *, #4177, .F. ) ;
#37991 = ORIENTED_EDGE ( 'NONE', *, *, #11103, .F. ) ;
#37992 = LINE ( 'NONE', #2613, #32958 ) ;
#37993 = ORIENTED_EDGE ( 'NONE', *, *, #9754, .F. ) ;
#37994 = ORIENTED_EDGE ( 'NONE', *, *, #10749, .F. ) ;
#37995 = CARTESIAN_POINT ( 'NONE',  ( -0.8306416476351717870, 0.009809765579796675752, -1.611421686139382192 ) ) ;
#37996 = CARTESIAN_POINT ( 'NONE',  ( 0.8182917201112824834, 0.000000000000000000, 1.850393700787392293 ) ) ;
#37997 = LINE ( 'NONE', #10622, #97 ) ;
#37998 = DIRECTION ( 'NONE',  ( -0.8805955318567391110, 0.000000000000000000, 0.4738686624729965269 ) ) ;
#37999 = VECTOR ( 'NONE', #2710, 39.37007874015748143 ) ;
#38000 = ORIENTED_EDGE ( 'NONE', *, *, #12098, .T. ) ;
#38001 = VECTOR ( 'NONE', #12569, 39.37007874015748143 ) ;
#38002 = CARTESIAN_POINT ( 'NONE',  ( -0.3486774197067335490, 3.267716535433071279, 1.209717811016577599E-16 ) ) ;
#38003 = EDGE_CURVE ( 'NONE', #4171, #11553, #35280, .T. ) ;
#38004 = LINE ( 'NONE', #38507, #14289 ) ;
#38005 = LINE ( 'NONE', #10118, #14628 ) ;
#38006 = B_SPLINE_CURVE_WITH_KNOTS ( 'NONE', 3,
 ( #12902, #12642, #21161, #22366 ),
 .UNSPECIFIED., .F., .F.,
 ( 4, 4 ),
 ( 0.001559031566645303814, 0.04607411539233744607 ),
 .UNSPECIFIED. ) ;
#38007 = ORIENTED_EDGE ( 'NONE', *, *, #12286, .F. ) ;
#38008 = DIRECTION ( 'NONE',  ( 0.2660368455666688448, 0.000000000000000000, 0.9639628606958550172 ) ) ;
#38009 = PLANE ( 'NONE',  #2139 ) ;
#38010 = FACE_OUTER_BOUND ( 'NONE', #7221, .T. ) ;
#38011 = ADVANCED_FACE ( 'NONE', ( #15653 ), #8675, .F. ) ;
#38012 = VERTEX_POINT ( 'NONE', #4288 ) ;
#38013 = ORIENTED_EDGE ( 'NONE', *, *, #20606, .T. ) ;
#38014 = CIRCLE ( 'NONE', #33079, 2.106299212598425008 ) ;
#38015 = LENGTH_MEASURE_WITH_UNIT ( LENGTH_MEASURE( 0.02539999999999999897 ), #7268 );
#38016 = CARTESIAN_POINT ( 'NONE',  ( -1.166969139818015755, 3.267716535433071279, 4.048737525165544676E-16 ) ) ;
#38017 = ADVANCED_FACE ( 'NONE', ( #20551 ), #12546, .F. ) ;
#38018 = CARTESIAN_POINT ( 'NONE',  ( 1.014069264286641792, 0.4724409448818898127, -1.014069264286642236 ) ) ;
#38019 = DIRECTION ( 'NONE',  ( 0.000000000000000000, -1.000000000000000000, 0.000000000000000000 ) ) ;
#38020 = ORIENTED_EDGE ( 'NONE', *, *, #16110, .T. ) ;
#38021 = ORIENTED_EDGE ( 'NONE', *, *, #45175, .F. ) ;
#38022 = CARTESIAN_POINT ( 'NONE',  ( 0.000000000000000000, 2.755905511811024056, -0.3740157480314960647 ) ) ;
#38023 = DIRECTION ( 'NONE',  ( -1.000000000000000000, -0.000000000000000000, -0.000000000000000000 ) ) ;
#38024 = ORIENTED_EDGE ( 'NONE', *, *, #8010, .F. ) ;
#38025 = CARTESIAN_POINT ( 'NONE',  ( -1.195183497228115035E-16, 0.000000000000000000, -1.574803149606293529 ) ) ;
#38026 = EDGE_CURVE ( 'NONE', #36594, #22069, #9703, .T. ) ;
#38027 = DIRECTION ( 'NONE',  ( -1.000000000000000000, 0.000000000000000000, -0.000000000000000000 ) ) ;
#38028 = CARTESIAN_POINT ( 'NONE',  ( 1.081562861160096700, 0.04524287409729283588, -1.572369041216798768 ) ) ;
#38029 = DIRECTION ( 'NONE',  ( -3.469446951953613696E-16, 0.000000000000000000, -1.000000000000000000 ) ) ;
#38030 = CARTESIAN_POINT ( 'NONE',  ( 1.091055626815042645, 3.267716535433071279, -1.892679809432644882E-16 ) ) ;
#38031 = ORIENTED_EDGE ( 'NONE', *, *, #36928, .F. ) ;
#38032 = DIRECTION ( 'NONE',  ( -0.000000000000000000, 1.000000000000000000, -0.000000000000000000 ) ) ;
#38033 = DIRECTION ( 'NONE',  ( 1.241861098869888840E-16, 1.000000000000000000, -3.427318860986102267E-17 ) ) ;
#38034 = EDGE_CURVE ( 'NONE', #7688, #46917, #2208, .T. ) ;
#38035 = DIRECTION ( 'NONE',  ( 1.000000000000000000, 0.000000000000000000, 0.000000000000000000 ) ) ;
#38036 = EDGE_CURVE ( 'NONE', #19894, #20329, #17702, .T. ) ;
#38037 = VECTOR ( 'NONE', #22715, 39.37007874015748143 ) ;
#38038 = EDGE_LOOP ( 'NONE', ( #6606, #48242, #12639, #8941 ) ) ;
#38039 = DIRECTION ( 'NONE',  ( 0.000000000000000000, 0.000000000000000000, -1.000000000000000000 ) ) ;
#38040 = CIRCLE ( 'NONE', #17433, 2.165354330708661568 ) ;
#38041 = CARTESIAN_POINT ( 'NONE',  ( 1.014069264286641792, 0.4724409448818898127, -5.863765863415223092E-17 ) ) ;
#38042 = DIRECTION ( 'NONE',  ( -0.000000000000000000, 0.000000000000000000, 1.000000000000000000 ) ) ;
#38043 = ORIENTED_EDGE ( 'NONE', *, *, #39094, .T. ) ;
#38044 = CARTESIAN_POINT ( 'NONE',  ( 4.268512490100411402E-16, 0.000000000000000000, 2.204724409448808764 ) ) ;
#38045 = ORIENTED_EDGE ( 'NONE', *, *, #1260, .T. ) ;
#38046 = CARTESIAN_POINT ( 'NONE',  ( -2.823445274216743073, 0.000000000000000000, 0.8656477926280280455 ) ) ;
#38047 = VECTOR ( 'NONE', #47589, 39.37007874015748143 ) ;
#38048 = ORIENTED_EDGE ( 'NONE', *, *, #9241, .F. ) ;
#38049 = LINE ( 'NONE', #46259, #41889 ) ;
#38050 = EDGE_CURVE ( 'NONE', #46240, #45206, #24934, .T. ) ;
#38051 = VECTOR ( 'NONE', #14342, 39.37007874015748143 ) ;
#38052 = CARTESIAN_POINT ( 'NONE',  ( -1.971834065208965203, 0.000000000000000000, 0.8963217522329899323 ) ) ;
#38053 = LINE ( 'NONE', #18923, #27192 ) ;
#38054 = CARTESIAN_POINT ( 'NONE',  ( 2.106197740627112402, 3.346456692913386100, 0.02067487291359298637 ) ) ;
#38055 =( BOUNDED_CURVE ( )  B_SPLINE_CURVE ( 3, ( #42881, #50580, #3148, #7023 ),
 .UNSPECIFIED., .F., .F. ) 
 B_SPLINE_CURVE_WITH_KNOTS ( ( 4, 4 ),
 ( 0.3208970237599759745, 0.3716576335890542926 ),
 .UNSPECIFIED. ) 
 CURVE ( )  GEOMETRIC_REPRESENTATION_ITEM ( )  RATIONAL_B_SPLINE_CURVE ( ( 1.000000000000000000, 0.9997852915667326812, 0.9997852915667326812, 1.000000000000000000 ) ) 
 REPRESENTATION_ITEM ( '' )  );
#38056 = ADVANCED_FACE ( 'NONE', ( #16945 ), #9954, .F. ) ;
#38057 = ORIENTED_EDGE ( 'NONE', *, *, #43113, .T. ) ;
#38058 = ORIENTED_EDGE ( 'NONE', *, *, #27332, .F. ) ;
#38059 = CARTESIAN_POINT ( 'NONE',  ( -0.3486774197067334380, 0.000000000000000000, 1.259842519685033357 ) ) ;
#38060 = DIRECTION ( 'NONE',  ( 1.734723475976806848E-16, -0.000000000000000000, 1.000000000000000000 ) ) ;
#38061 = ORIENTED_EDGE ( 'NONE', *, *, #21088, .F. ) ;
#38062 = FACE_OUTER_BOUND ( 'NONE', #14761, .T. ) ;
#38063 = LINE ( 'NONE', #3185, #19479 ) ;
#38064 = CARTESIAN_POINT ( 'NONE',  ( 0.2727639067037604947, 3.346456692913386100, -0.1574803149606298636 ) ) ;
#38065 = VERTEX_POINT ( 'NONE', #25439 ) ;
#38066 = ORIENTED_EDGE ( 'NONE', *, *, #50776, .T. ) ;
#38067 = PLANE ( 'NONE',  #41977 ) ;
#38068 = DIRECTION ( 'NONE',  ( 0.4338837391175656699, 0.000000000000000000, -0.9009688679024154823 ) ) ;
#38069 = LINE ( 'NONE', #6572, #38754 ) ;
#38070 = VERTEX_POINT ( 'NONE', #21829 ) ;
#38071 = DIRECTION ( 'NONE',  ( 0.7818314824680311359, 0.000000000000000000, -0.6234898018587319291 ) ) ;
#38072 = FACE_BOUND ( 'NONE', #34421, .T. ) ;
#38073 = ORIENTED_EDGE ( 'NONE', *, *, #35845, .F. ) ;
#38074 = CARTESIAN_POINT ( 'NONE',  ( -1.166969139818015977, 3.346456692913386100, -0.4724409448818886470 ) ) ;
#38075 = EDGE_LOOP ( 'NONE', ( #37295, #18750, #16499, #46702 ) ) ;
#38076 = VERTEX_POINT ( 'NONE', #14079 ) ;
#38077 = LINE ( 'NONE', #37321, #41094 ) ;
#38078 = LINE ( 'NONE', #5555, #34128 ) ;
#38079 = AXIS2_PLACEMENT_3D ( 'NONE', #13077, #29583, #49158 ) ;
#38081 = VECTOR ( 'NONE', #25171, 39.37007874015748143 ) ;
#38080 = LINE ( 'NONE', #2956, #30514 ) ;
#38082 = EDGE_CURVE ( 'NONE', #30055, #24780, #5311, .T. ) ;
#38083 = CARTESIAN_POINT ( 'NONE',  ( -0.2727639067037607723, 0.000000000000000000, 2.362204724409437961 ) ) ;
#38084 = CARTESIAN_POINT ( 'NONE',  ( 2.182111253630085290, 3.267716535433071279, -0.1968503937007886062 ) ) ;
#38085 = VERTEX_POINT ( 'NONE', #29052 ) ;
#38086 = AXIS2_PLACEMENT_3D ( 'NONE', #42037, #22171, #10038 ) ;
#38087 = AXIS2_PLACEMENT_3D ( 'NONE', #26051, #6180, #33818 ) ;
#38088 = ORIENTED_EDGE ( 'NONE', *, *, #49256, .F. ) ;
#38089 = LINE ( 'NONE', #15091, #50781 ) ;
#38090 = ADVANCED_FACE ( 'NONE', ( #20806 ), #49150, .F. ) ;
#38091 = CARTESIAN_POINT ( 'NONE',  ( -2.318785326816343861, 1.683110758435957477, 1.828187939119067851 ) ) ;
#38092 = CIRCLE ( 'NONE', #22418, 2.106299212598425008 ) ;
#38093 = ADVANCED_FACE ( 'NONE', ( #24684 ), #40440, .F. ) ;
#38094 = EDGE_CURVE ( 'NONE', #28481, #38735, #44068, .T. ) ;
#38095 = CARTESIAN_POINT ( 'NONE',  ( 1.636583440222563857, 0.000000000000000000, 0.3149606299212576177 ) ) ;
#38096 = DIRECTION ( 'NONE',  ( 1.000000000000000000, 0.000000000000000000, -3.469446951953613696E-16 ) ) ;
#38097 = DIRECTION ( 'NONE',  ( -0.01601477604151182663, 0.9998717552508123996, -0.000000000000000000 ) ) ;
#38098 = ORIENTED_EDGE ( 'NONE', *, *, #38050, .F. ) ;
#38099 = DIRECTION ( 'NONE',  ( 0.9009688679024154823, 0.000000000000000000, 0.4338837391175656699 ) ) ;
#38100 = ADVANCED_FACE ( 'NONE', ( #32701 ), #5312, .F. ) ;
#38101 = CARTESIAN_POINT ( 'NONE',  ( 1.833433833923350909, 3.267716535433071279, -6.361001426713997494E-16 ) ) ;
#38102 = EDGE_LOOP ( 'NONE', ( #5386, #31813, #30386, #28317, #9629 ) ) ;
#38103 = CARTESIAN_POINT ( 'NONE',  ( 2.491402175429654253, 1.659612532563349285, -1.585592796919505831 ) ) ;
#38104 = DIRECTION ( 'NONE',  ( 1.000000000000000000, 0.000000000000000000, 0.000000000000000000 ) ) ;
#38105 = ORIENTED_EDGE ( 'NONE', *, *, #6286, .T. ) ;
#38106 = LINE ( 'NONE', #9714, #28791 ) ;
#38107 = CARTESIAN_POINT ( 'NONE',  ( -1.734268221780295827, 0.000000000000000000, 0.1852605408175444779 ) ) ;
#38108 = CARTESIAN_POINT ( 'NONE',  ( 0.7381027496705270252, 1.499047760149736952, -2.859439394060913298 ) ) ;
#38109 = ORIENTED_EDGE ( 'NONE', *, *, #19589, .F. ) ;
#38110 = CARTESIAN_POINT ( 'NONE',  ( 0.000000000000000000, 3.267716535433071279, 0.9055118110236167750 ) ) ;
#38111 = ORIENTED_EDGE ( 'NONE', *, *, #24171, .T. ) ;
#38112 = DIRECTION ( 'NONE',  ( 0.000000000000000000, 0.000000000000000000, 1.000000000000000000 ) ) ;
#38113 = DIRECTION ( 'NONE',  ( -0.01601477604151182663, 0.9998717552508123996, -0.000000000000000000 ) ) ;
#38114 = EDGE_CURVE ( 'NONE', #23605, #11539, #47783, .T. ) ;
#38115 = AXIS2_PLACEMENT_3D ( 'NONE', #43684, #12981, #32873 ) ;
#38116 = LINE ( 'NONE', #27227, #12800 ) ;
#38117 = DIRECTION ( 'NONE',  ( -0.000000000000000000, 1.000000000000000000, -0.000000000000000000 ) ) ;
#38118 = ADVANCED_FACE ( 'NONE', ( #13071 ), #21575, .F. ) ;
#38119 = VECTOR ( 'NONE', #27932, 39.37007874015748143 ) ;
#38120 = ORIENTED_EDGE ( 'NONE', *, *, #30715, .T. ) ;
#38121 = ORIENTED_EDGE ( 'NONE', *, *, #7759, .T. ) ;
#38122 = CARTESIAN_POINT ( 'NONE',  ( -1.363819533518803473, 3.346456692913386100, -1.299212598425192544 ) ) ;
#38123 = EDGE_CURVE ( 'NONE', #40287, #51008, #45292, .T. ) ;
#38124 = CARTESIAN_POINT ( 'NONE',  ( -0.5455278134075214336, 3.346456692913386100, -1.889763779527552146 ) ) ;
#38125 = AXIS2_PLACEMENT_3D ( 'NONE', #24920, #12529, #40671 ) ;
#38126 = DIRECTION ( 'NONE',  ( -1.105928667600717569E-16, 1.000000000000000000, -6.607616187506203079E-17 ) ) ;
#38127 = DIRECTION ( 'NONE',  ( -0.000000000000000000, 1.000000000000000000, -0.000000000000000000 ) ) ;
#38128 = CARTESIAN_POINT ( 'NONE',  ( -1.536664496436148184E-16, 3.346456692913386100, -1.771653543307081025 ) ) ;
#38129 = VECTOR ( 'NONE', #46873, 39.37007874015748143 ) ;
#38130 = ORIENTED_EDGE ( 'NONE', *, *, #42786, .F. ) ;
#38131 = ORIENTED_EDGE ( 'NONE', *, *, #49982, .F. ) ;
#38132 = CARTESIAN_POINT ( 'NONE',  ( 1.015142113812069313, 3.346456692913386100, 0.5905511811023579360 ) ) ;
#38133 = EDGE_CURVE ( 'NONE', #21081, #33042, #17195, .T. ) ;
#38134 = CARTESIAN_POINT ( 'NONE',  ( -2.142805232260985182, -3.932816271735134525E-17, 0.3399247426648318582 ) ) ;
#38135 = ORIENTED_EDGE ( 'NONE', *, *, #11622, .F. ) ;
#38136 = DIRECTION ( 'NONE',  ( -1.000000000000000000, 0.000000000000000000, 0.000000000000000000 ) ) ;
#38137 = VERTEX_POINT ( 'NONE', #1694 ) ;
#38138 = ORIENTED_EDGE ( 'NONE', *, *, #10169, .T. ) ;
#38139 = ORIENTED_EDGE ( 'NONE', *, *, #3937, .F. ) ;
#38140 = VERTEX_POINT ( 'NONE', #17444 ) ;
#38141 = CARTESIAN_POINT ( 'NONE',  ( 2.193564619503452828, 1.644610705845120258, 0.7644775380370429918 ) ) ;
#38142 = ORIENTED_EDGE ( 'NONE', *, *, #47684, .F. ) ;
#38143 = DIRECTION ( 'NONE',  ( 0.000000000000000000, -1.000000000000000000, -0.000000000000000000 ) ) ;
#38144 = DIRECTION ( 'NONE',  ( 1.000000000000000000, 0.000000000000000000, 0.000000000000000000 ) ) ;
#38145 = VECTOR ( 'NONE', #20396, 39.37007874015748143 ) ;
#38146 = ADVANCED_FACE ( 'NONE', ( #48887 ), #29315, .F. ) ;
#38147 = ADVANCED_FACE ( 'NONE', ( #22582 ), #37153, .T. ) ;
#38148 = CARTESIAN_POINT ( 'NONE',  ( -0.4788131938641531637, 1.205361022782829114E-17, 2.914091152102186388 ) ) ;
#38149 = EDGE_CURVE ( 'NONE', #24903, #41095, #48973, .T. ) ;
#38150 = CONICAL_SURFACE ( 'NONE', #30731, 3.033577403570480779, 1.554780866114618743 ) ;
#38151 = CARTESIAN_POINT ( 'NONE',  ( -1.439733046521776361, 3.346456692913386100, -0.1968503937007879123 ) ) ;
#38152 = CARTESIAN_POINT ( 'NONE',  ( -0.8182917201112819283, 3.346456692913386100, -1.614173228346451605 ) ) ;
#38153 = EDGE_LOOP ( 'NONE', ( #26373, #45174, #38680, #26060 ) ) ;
#38154 = DIRECTION ( 'NONE',  ( 0.000000000000000000, 0.000000000000000000, 1.000000000000000000 ) ) ;
#38155 = FACE_OUTER_BOUND ( 'NONE', #49015, .T. ) ;
#38156 = VECTOR ( 'NONE', #11700, 39.37007874015748143 ) ;
#38157 = LINE ( 'NONE', #33530, #22696 ) ;
#38158 = CARTESIAN_POINT ( 'NONE',  ( 1.091055626815042645, 3.267716535433071279, 0.7480314960629872445 ) ) ;
#38159 = VECTOR ( 'NONE', #33396, 39.37007874015748143 ) ;
#38160 = AXIS2_PLACEMENT_3D ( 'NONE', #17069, #5700, #8540 ) ;
#38161 = ORIENTED_EDGE ( 'NONE', *, *, #6282, .F. ) ;
#38162 = DIRECTION ( 'NONE',  ( -0.000000000000000000, 1.000000000000000000, -0.000000000000000000 ) ) ;
#38163 = DIRECTION ( 'NONE',  ( -1.000000000000000000, 0.000000000000000000, -0.000000000000000000 ) ) ;
#38164 = VERTEX_POINT ( 'NONE', #45542 ) ;
#38165 = CARTESIAN_POINT ( 'NONE',  ( 2.339241080213585899, 1.657243480315735873, 1.802537235681917815 ) ) ;
#38167 = B_SPLINE_CURVE_WITH_KNOTS ( 'NONE', 3,
 ( #3348, #42088, #18851, #2594 ),
 .UNSPECIFIED., .F., .F.,
 ( 4, 4 ),
 ( 2.007585174703544570E-07, 0.002500777222804251645 ),
 .UNSPECIFIED. ) ;
#38166 = CARTESIAN_POINT ( 'NONE',  ( 1.363819533518803029, 0.000000000000000000, -1.102362204724405714 ) ) ;
#38168 = VERTEX_POINT ( 'NONE', #41955 ) ;
#38169 = FACE_OUTER_BOUND ( 'NONE', #19587, .T. ) ;
#38170 = EDGE_CURVE ( 'NONE', #196, #46048, #24425, .T. ) ;
#38171 = ORIENTED_EDGE ( 'NONE', *, *, #14123, .T. ) ;
#38172 = CARTESIAN_POINT ( 'NONE',  ( 1.352759075253495258, -0.6299212598425202314, 0.2762566512555730269 ) ) ;
#38173 = DIRECTION ( 'NONE',  ( -0.000000000000000000, 0.000000000000000000, 1.000000000000000000 ) ) ;
#38174 = CARTESIAN_POINT ( 'NONE',  ( 0.08119777152254364916, 1.623385212329073957, 0.000000000000000000 ) ) ;
#38175 = ADVANCED_FACE ( 'NONE', ( #47227, #26453 ), #50155, .T. ) ;
#38176 = CARTESIAN_POINT ( 'NONE',  ( 0.000000000000000000, 3.267716535433071279, 1.535433070866133898 ) ) ;
#38177 = DIRECTION ( 'NONE',  ( 0.000000000000000000, -0.000000000000000000, 1.000000000000000000 ) ) ;
#38178 = ORIENTED_EDGE ( 'NONE', *, *, #44992, .F. ) ;
#38179 = EDGE_CURVE ( 'NONE', #20106, #7882, #31531, .T. ) ;
#38180 = DIRECTION ( 'NONE',  ( -1.000000000000000000, -0.000000000000000000, -0.000000000000000000 ) ) ;
#38181 = ORIENTED_EDGE ( 'NONE', *, *, #26826, .F. ) ;
#38182 = ORIENTED_EDGE ( 'NONE', *, *, #34551, .T. ) ;
#38183 = CARTESIAN_POINT ( 'NONE',  ( 0.002207914879453961535, -5.712274067634378313E-18, 0.04916304461325374242 ) ) ;
#38184 = ADVANCED_FACE ( 'NONE', ( #2968 ), #18208, .F. ) ;
#38185 = VERTEX_POINT ( 'NONE', #34467 ) ;
#38186 = LINE ( 'NONE', #37930, #4864 ) ;
#38187 = CARTESIAN_POINT ( 'NONE',  ( -0.6214413264104945434, 3.346456692913386100, -0.3543307086614175816 ) ) ;
#38188 = EDGE_CURVE ( 'NONE', #1872, #33170, #43130, .T. ) ;
#38189 = ORIENTED_EDGE ( 'NONE', *, *, #30694, .T. ) ;
#38190 = DIRECTION ( 'NONE',  ( -0.000000000000000000, 1.000000000000000000, -0.000000000000000000 ) ) ;
#38191 = CARTESIAN_POINT ( 'NONE',  ( -1.166969139818015533, 3.267716535433071279, 1.417322834645662777 ) ) ;
#38192 = AXIS2_PLACEMENT_3D ( 'NONE', #18694, #23308, #19426 ) ;
#38193 = FACE_OUTER_BOUND ( 'NONE', #42540, .T. ) ;
#38194 = VERTEX_POINT ( 'NONE', #10715 ) ;
#38195 = ORIENTED_EDGE ( 'NONE', *, *, #18524, .T. ) ;
#38196 = LINE ( 'NONE', #49751, #18278 ) ;
#38197 = FACE_BOUND ( 'NONE', #6275, .T. ) ;
#38198 = ORIENTED_EDGE ( 'NONE', *, *, #20952, .F. ) ;
#38199 = VECTOR ( 'NONE', #38516, 39.37007874015748143 ) ;
#38200 = VECTOR ( 'NONE', #3594, 39.37007874015748143 ) ;
#38201 = CARTESIAN_POINT ( 'NONE',  ( 0.000000000000000000, 3.267716535433071279, -1.456692913385822186 ) ) ;
#38202 = PLANE ( 'NONE',  #46465 ) ;
#38203 = ORIENTED_EDGE ( 'NONE', *, *, #21722, .F. ) ;
#38204 = ORIENTED_EDGE ( 'NONE', *, *, #7689, .F. ) ;
#38205 = CARTESIAN_POINT ( 'NONE',  ( 1.560669927219590747, 3.346456692913386100, -0.1574803149606304187 ) ) ;
#38206 = AXIS2_PLACEMENT_3D ( 'NONE', #17448, #18212, #10210 ) ;
#38207 = DIRECTION ( 'NONE',  ( 7.097135778201662695E-17, 1.000000000000000000, -1.075170113095010447E-16 ) ) ;
#38208 = ORIENTED_EDGE ( 'NONE', *, *, #6864, .T. ) ;
#38209 = VERTEX_POINT ( 'NONE', #27383 ) ;
#38210 = ORIENTED_EDGE ( 'NONE', *, *, #3808, .T. ) ;
#38211 = CARTESIAN_POINT ( 'NONE',  ( 1.015142113812069091, 3.346456692913386100, -1.912654141836395816 ) ) ;
#38212 = CARTESIAN_POINT ( 'NONE',  ( 0.000000000000000000, 2.362204724409439294, 0.000000000000000000 ) ) ;
#38213 = DIRECTION ( 'NONE',  ( 0.8345732537213079727, 6.391122427287080193E-17, -0.5508969814520945363 ) ) ;
#38214 = ORIENTED_EDGE ( 'NONE', *, *, #39673, .F. ) ;
#38215 = ORIENTED_EDGE ( 'NONE', *, *, #3647, .F. ) ;
#38216 = EDGE_CURVE ( 'NONE', #21605, #2219, #6339, .T. ) ;
#38217 = DIRECTION ( 'NONE',  ( -1.000000000000000000, 0.000000000000000000, -0.000000000000000000 ) ) ;
#38218 = EDGE_CURVE ( 'NONE', #46986, #18782, #35408, .T. ) ;
#38219 = LINE ( 'NONE', #41571, #44763 ) ;
#38220 = DIRECTION ( 'NONE',  ( 0.8805955318567321166, -5.503865196449042635E-17, 0.4738686624730094055 ) ) ;
#38221 = ADVANCED_FACE ( 'NONE', ( #14842 ), #37846, .F. ) ;
#38222 = CARTESIAN_POINT ( 'NONE',  ( -0.3486774197067334935, 3.267716535433071279, 0.7480314960629874665 ) ) ;
#38223 = DIRECTION ( 'NONE',  ( -0.9998717552508121775, -0.01601477604151182316, 0.000000000000000000 ) ) ;
#38224 = LINE ( 'NONE', #46182, #43169 ) ;
#38225 = AXIS2_PLACEMENT_3D ( 'NONE', #39248, #31261, #23498 ) ;
#38226 = VERTEX_POINT ( 'NONE', #33966 ) ;
#38227 = LINE ( 'NONE', #30474, #4465 ) ;
#38228 = DIRECTION ( 'NONE',  ( -3.469446951953613696E-16, 0.000000000000000000, -1.000000000000000000 ) ) ;
#38229 = VECTOR ( 'NONE', #426, 39.37007874015748854 ) ;
#38230 = ORIENTED_EDGE ( 'NONE', *, *, #12257, .T. ) ;
#38231 = VECTOR ( 'NONE', #35844, 39.37007874015748143 ) ;
#38232 = ORIENTED_EDGE ( 'NONE', *, *, #44766, .T. ) ;
#38234 = AXIS2_PLACEMENT_3D ( 'NONE', #45604, #41264, #49459 ) ;
#38233 = CARTESIAN_POINT ( 'NONE',  ( 2.755905511811024056, 2.913385826771657250, -1.023622047244094224 ) ) ;
#38235 = FACE_OUTER_BOUND ( 'NONE', #38386, .T. ) ;
#38236 = EDGE_CURVE ( 'NONE', #27703, #19989, #28062, .T. ) ;
#38237 = ORIENTED_EDGE ( 'NONE', *, *, #13864, .T. ) ;
#38238 = AXIS2_PLACEMENT_3D ( 'NONE', #870, #39345, #11978 ) ;
#38239 = EDGE_CURVE ( 'NONE', #37842, #35391, #3912, .T. ) ;
#38240 = VERTEX_POINT ( 'NONE', #8031 ) ;
#38241 = CARTESIAN_POINT ( 'NONE',  ( -0.2727639067037610499, 0.000000000000000000, -2.047244094488181343 ) ) ;
#38242 = ORIENTED_EDGE ( 'NONE', *, *, #32822, .F. ) ;
#38243 = CARTESIAN_POINT ( 'NONE',  ( 0.8455406139730251569, 3.267716535433071279, -1.929133858267711110 ) ) ;
#38244 = CARTESIAN_POINT ( 'NONE',  ( 1.542217245295272932, 0.05262109711011796892, 1.166931937029544564 ) ) ;
#38245 = EDGE_LOOP ( 'NONE', ( #10618, #33251, #31143, #34751 ) ) ;
#38246 = CARTESIAN_POINT ( 'NONE',  ( -1.863748091109392213, 3.346456692913386100, -1.102362204724405492 ) ) ;
#38247 = ORIENTED_EDGE ( 'NONE', *, *, #18967, .F. ) ;
#38248 = VERTEX_POINT ( 'NONE', #23780 ) ;
#38249 = DIRECTION ( 'NONE',  ( 0.000000000000000000, 0.000000000000000000, -1.000000000000000000 ) ) ;
#38250 = FACE_OUTER_BOUND ( 'NONE', #28279, .T. ) ;
#38251 = CARTESIAN_POINT ( 'NONE',  ( -1.195183497228115035E-16, 3.267716535433071279, -0.3149606299212591165 ) ) ;
#38252 = CARTESIAN_POINT ( 'NONE',  ( 0.002207914879453961969, 5.905511811023623991, 0.04916304461325442243 ) ) ;
#38253 = ORIENTED_EDGE ( 'NONE', *, *, #26058, .F. ) ;
#38254 = DIRECTION ( 'NONE',  ( 0.9005016466594218949, -0.000000000000000000, -0.4348526007323282871 ) ) ;
#38255 = CARTESIAN_POINT ( 'NONE',  ( -1.690941099774203815, 0.0008361491594236539725, -0.4364244636917575804 ) ) ;
#38256 = CARTESIAN_POINT ( 'NONE',  ( 4.268512490100411402E-16, 3.346456692913386100, 1.889763779527550369 ) ) ;
#38257 = ORIENTED_EDGE ( 'NONE', *, *, #35346, .F. ) ;
#38258 = FACE_OUTER_BOUND ( 'NONE', #46192, .T. ) ;
#38259 = AXIS2_PLACEMENT_3D ( 'NONE', #25180, #30069, #6326 ) ;
#38260 = VECTOR ( 'NONE', #13069, 39.37007874015748143 ) ;
#38261 = ORIENTED_EDGE ( 'NONE', *, *, #26699, .T. ) ;
#38262 = AXIS2_PLACEMENT_3D ( 'NONE', #30978, #47439, #19593 ) ;
#38263 = ORIENTED_EDGE ( 'NONE', *, *, #17440, .T. ) ;
#38264 = DIRECTION ( 'NONE',  ( -0.3250930791930596864, 0.5055833184555331705, 0.7991870857066361022 ) ) ;
#38265 = VECTOR ( 'NONE', #30285, 39.37007874015748143 ) ;
#38266 = AXIS2_PLACEMENT_3D ( 'NONE', #50037, #45931, #10597 ) ;
#38267 = CARTESIAN_POINT ( 'NONE',  ( -3.346456692913387432, 0.000000000000000000, 2.165354330708661124 ) ) ;
#38268 = CARTESIAN_POINT ( 'NONE',  ( 1.776015598323502198, 0.5249316497054298258, 0.6288076369129006471 ) ) ;
#38269 = CARTESIAN_POINT ( 'NONE',  ( 0.04921259842519670746, 1.514263714023589502, 2.952755905511811108 ) ) ;
#38270 = ORIENTED_EDGE ( 'NONE', *, *, #38003, .T. ) ;
#38271 = VERTEX_POINT ( 'NONE', #30083 ) ;
#38272 = EDGE_CURVE ( 'NONE', #42546, #31066, #45797, .T. ) ;
#38273 = VECTOR ( 'NONE', #46739, 39.37007874015748143 ) ;
#38274 = SURFACE_STYLE_FILL_AREA ( #50328 ) ;
#38275 = EDGE_CURVE ( 'NONE', #22076, #48087, #22338, .T. ) ;
#38276 = PLANE ( 'NONE',  #16881 ) ;
#38277 = B_SPLINE_CURVE_WITH_KNOTS ( 'NONE', 3,
 ( #42506, #6887, #26503, #31147 ),
 .UNSPECIFIED., .F., .F.,
 ( 4, 4 ),
 ( 2.102951466402419151E-07, 0.002500239283416568880 ),
 .UNSPECIFIED. ) ;
#38278 = ORIENTED_EDGE ( 'NONE', *, *, #10050, .F. ) ;
#38279 = LINE ( 'NONE', #2392, #12602 ) ;
#38280 = CARTESIAN_POINT ( 'NONE',  ( -2.882375110776534299, 1.574243653623555339, -0.6410540981532866223 ) ) ;
#38281 = EDGE_CURVE ( 'NONE', #25746, #33365, #48256, .T. ) ;
#38282 = ADVANCED_FACE ( 'NONE', ( #44159 ), #4417, .F. ) ;
#38283 = EDGE_CURVE ( 'NONE', #41994, #23774, #12942, .T. ) ;
#38284 = FACE_OUTER_BOUND ( 'NONE', #25812, .T. ) ;
#38285 = DIRECTION ( 'NONE',  ( -0.000000000000000000, 0.000000000000000000, 1.000000000000000000 ) ) ;
#38286 = CARTESIAN_POINT ( 'NONE',  ( 0.8182917201112824834, 0.000000000000000000, 1.535433070866133898 ) ) ;
#38287 = VERTEX_POINT ( 'NONE', #21196 ) ;
#38288 = CARTESIAN_POINT ( 'NONE',  ( 4.580371886574746102E-17, 2.755905511811024056, 0.3740157480314960647 ) ) ;
#38289 = CARTESIAN_POINT ( 'NONE',  ( -0.4513972801127658641, 3.267716535433071279, -2.401574803149598036 ) ) ;
#38290 = CARTESIAN_POINT ( 'NONE',  ( -0.06966273521059175577, 2.755905511811024056, 0.3674709282358789575 ) ) ;
#38291 = VERTEX_POINT ( 'NONE', #13195 ) ;
#38292 = CARTESIAN_POINT ( 'NONE',  ( 0.4696143004045484348, 3.267716535433071279, 2.165354330708650910 ) ) ;
#38293 = DIRECTION ( 'NONE',  ( -0.000000000000000000, 1.000000000000000000, -0.000000000000000000 ) ) ;
#38294 = EDGE_CURVE ( 'NONE', #17089, #15497, #32052, .T. ) ;
#38295 = CARTESIAN_POINT ( 'NONE',  ( 1.441853549388196321, 3.267716535433071279, 1.535433070866133898 ) ) ;
#38296 = ORIENTED_EDGE ( 'NONE', *, *, #21790, .F. ) ;
#38297 = PLANE ( 'NONE',  #29183 ) ;
#38298 = VECTOR ( 'NONE', #28720, 39.37007874015748143 ) ;
#38299 = VECTOR ( 'NONE', #41633, 39.37007874015748143 ) ;
#38300 = EDGE_CURVE ( 'NONE', #48919, #50319, #20152, .T. ) ;
#38301 = ORIENTED_EDGE ( 'NONE', *, *, #25701, .F. ) ;
#38302 = AXIS2_PLACEMENT_3D ( 'NONE', #4573, #28309, #8953 ) ;
#38303 = FACE_OUTER_BOUND ( 'NONE', #48270, .T. ) ;
#38304 = EDGE_LOOP ( 'NONE', ( #34234, #10647, #31649, #4649 ) ) ;
#38305 = DIRECTION ( 'NONE',  ( -0.9998717552508122886, -0.01601477604151180928, 0.000000000000000000 ) ) ;
#38306 = VECTOR ( 'NONE', #952, 39.37007874015748143 ) ;
#38307 = VECTOR ( 'NONE', #11097, 39.37007874015748143 ) ;
#38308 = FACE_OUTER_BOUND ( 'NONE', #2632, .T. ) ;
#38309 = DIRECTION ( 'NONE',  ( 1.000000000000000000, 0.000000000000000000, 0.000000000000000000 ) ) ;
#38310 = DIRECTION ( 'NONE',  ( 1.734723475976806848E-16, 0.000000000000000000, 1.000000000000000000 ) ) ;
#38311 = EDGE_CURVE ( 'NONE', #30476, #3517, #9059, .T. ) ;
#38312 = ORIENTED_EDGE ( 'NONE', *, *, #12937, .F. ) ;
#38313 = ORIENTED_EDGE ( 'NONE', *, *, #50952, .F. ) ;
#38314 = DIRECTION ( 'NONE',  ( -0.000000000000000000, 1.000000000000000000, -0.000000000000000000 ) ) ;
#38315 = CARTESIAN_POINT ( 'NONE',  ( -0.4349608091551073197, 1.574803149606302854, 2.121218629000295230 ) ) ;
#38316 = ORIENTED_EDGE ( 'NONE', *, *, #37671, .F. ) ;
#38317 = CARTESIAN_POINT ( 'NONE',  ( 0.5455278134075214336, 3.267716535433071279, -9.463399047163225645E-17 ) ) ;
#38318 = CARTESIAN_POINT ( 'NONE',  ( -0.3486774197067339376, 3.267716535433071279, -0.6299212598425175669 ) ) ;
#38319 = EDGE_CURVE ( 'NONE', #23810, #17176, #47742, .T. ) ;
#38320 = ORIENTED_EDGE ( 'NONE', *, *, #40646, .T. ) ;
#38321 = ORIENTED_EDGE ( 'NONE', *, *, #34516, .T. ) ;
#38322 = CARTESIAN_POINT ( 'NONE',  ( -0.1692531782225912829, 2.755905511811024056, 0.3335283217915853138 ) ) ;
#38323 = PLANE ( 'NONE',  #46396 ) ;
#38324 = DIRECTION ( 'NONE',  ( 7.097135778201508621E-17, 1.000000000000000000, 1.075170113095020677E-16 ) ) ;
#38325 = ORIENTED_EDGE ( 'NONE', *, *, #28629, .T. ) ;
#38326 = CARTESIAN_POINT ( 'NONE',  ( -0.6214413264104945434, 3.267716535433071279, 2.012537465693970962 ) ) ;
#38327 = CARTESIAN_POINT ( 'NONE',  ( -1.439733046521776139, 0.000000000000000000, -4.780733988912460139E-16 ) ) ;
#38328 = ORIENTED_EDGE ( 'NONE', *, *, #42236, .F. ) ;
#38329 = DIRECTION ( 'NONE',  ( 0.000000000000000000, 0.000000000000000000, 1.000000000000000000 ) ) ;
#38330 = VERTEX_POINT ( 'NONE', #12417 ) ;
#38331 = VERTEX_POINT ( 'NONE', #48511 ) ;
#38332 = CARTESIAN_POINT ( 'NONE',  ( -1.536664496436148184E-16, 0.000000000000000000, -1.456692913385822630 ) ) ;
#38333 = LINE ( 'NONE', #2953, #19323 ) ;
#38334 = CARTESIAN_POINT ( 'NONE',  ( 4.268512490100411402E-16, 3.346456692913386100, 2.204724409448808764 ) ) ;
#38335 = CARTESIAN_POINT ( 'NONE',  ( 2.277873973731426194, 1.754757658573260048, 1.879489153247668076 ) ) ;
#38336 = FACE_OUTER_BOUND ( 'NONE', #18741, .T. ) ;
#38337 = ORIENTED_EDGE ( 'NONE', *, *, #40026, .F. ) ;
#38338 = CIRCLE ( 'NONE', #46544, 2.165354330708661568 ) ;
#38339 = VERTEX_POINT ( 'NONE', #28928 ) ;
#38340 = LINE ( 'NONE', #3212, #47485 ) ;
#38341 = CARTESIAN_POINT ( 'NONE',  ( 1.014069264286641570, 0.5905511811023621549, -1.062992125984252301 ) ) ;
#38342 = ADVANCED_FACE ( 'NONE', ( #8545 ), #20935, .F. ) ;
#38343 = EDGE_CURVE ( 'NONE', #4293, #4534, #24808, .T. ) ;
#38344 = CARTESIAN_POINT ( 'NONE',  ( -1.472219874544909768, 1.597879704547665369, 2.560030851058948898 ) ) ;
#38345 = ADVANCED_FACE ( 'NONE', ( #16809 ), #12162, .T. ) ;
#38346 = DIRECTION ( 'NONE',  ( -0.9998717552508122886, -0.01601477604151181275, 0.000000000000000000 ) ) ;
#38347 = FACE_OUTER_BOUND ( 'NONE', #25217, .T. ) ;
#38348 = ORIENTED_EDGE ( 'NONE', *, *, #11458, .F. ) ;
#38349 = DIRECTION ( 'NONE',  ( -0.000000000000000000, 1.000000000000000000, -0.000000000000000000 ) ) ;
#38350 = CARTESIAN_POINT ( 'NONE',  ( -1.166969139818015533, 3.346456692913386100, 0.7874015748031456541 ) ) ;
#38351 = ORIENTED_EDGE ( 'NONE', *, *, #25040, .F. ) ;
#38352 = FACE_OUTER_BOUND ( 'NONE', #14877, .T. ) ;
#38353 = CARTESIAN_POINT ( 'NONE',  ( -1.091055626815042645, 3.346456692913386100, -1.456692913385822186 ) ) ;
#38354 = ORIENTED_EDGE ( 'NONE', *, *, #2507, .F. ) ;
#38355 = CARTESIAN_POINT ( 'NONE',  ( -0.7145799201509074328, 1.574803149606302854, 2.044048657746648789 ) ) ;
#38356 = CARTESIAN_POINT ( 'NONE',  ( 1.560669927219590303, 3.267716535433071279, -5.414661521997676285E-16 ) ) ;
#38357 = FACE_OUTER_BOUND ( 'NONE', #39478, .T. ) ;
#38358 = VERTEX_POINT ( 'NONE', #44662 ) ;
#38359 = DIRECTION ( 'NONE',  ( 0.000000000000000000, -1.000000000000000000, 0.000000000000000000 ) ) ;
#38360 = ORIENTED_EDGE ( 'NONE', *, *, #5851, .F. ) ;
#38361 = PLANE ( 'NONE',  #18794 ) ;
#38362 = CARTESIAN_POINT ( 'NONE',  ( 1.287906020515830141, 3.267716535433071279, 1.259842519685033357 ) ) ;
#38363 = DIRECTION ( 'NONE',  ( -1.000000000000000000, 0.000000000000000000, 1.734723475976806848E-16 ) ) ;
#38364 = ADVANCED_FACE ( 'NONE', ( #40558 ), #32307, .F. ) ;
#38365 = ORIENTED_EDGE ( 'NONE', *, *, #50857, .T. ) ;
#38366 = ORIENTED_EDGE ( 'NONE', *, *, #37764, .F. ) ;
#38367 = PLANE ( 'NONE',  #8360 ) ;
#38368 = VECTOR ( 'NONE', #11028, 39.37007874015748143 ) ;
#38369 = CARTESIAN_POINT ( 'NONE',  ( -1.068402561569949283, 6.692913385826772199, -1.884154513482188209 ) ) ;
#38370 = VECTOR ( 'NONE', #37175, 39.37007874015748143 ) ;
#38371 = CARTESIAN_POINT ( 'NONE',  ( 1.636583440222563857, 3.346456692913386100, 0.7480314960629872445 ) ) ;
#38372 = DIRECTION ( 'NONE',  ( -3.986037398843765983E-20, -1.000000000000000000, -1.160734090543304660E-16 ) ) ;
#38373 = EDGE_CURVE ( 'NONE', #50100, #29332, #36174, .T. ) ;
#38374 = VECTOR ( 'NONE', #38491, 39.37007874015748143 ) ;
#38375 = CARTESIAN_POINT ( 'NONE',  ( 0.000000000000000000, 3.346456692913386100, 0.000000000000000000 ) ) ;
#38376 = ORIENTED_EDGE ( 'NONE', *, *, #5741, .T. ) ;
#38377 = VERTEX_POINT ( 'NONE', #47996 ) ;
#38378 = CARTESIAN_POINT ( 'NONE',  ( 2.793030215715258446, 0.000000000000000000, 0.9592557174602679426 ) ) ;
#38379 = ADVANCED_FACE ( 'NONE', ( #12674 ), #39782, .F. ) ;
#38380 = LINE ( 'NONE', #30625, #12440 ) ;
#38381 = VECTOR ( 'NONE', #25976, 39.37007874015748143 ) ;
#38382 = ORIENTED_EDGE ( 'NONE', *, *, #40456, .F. ) ;
#38383 = EDGE_CURVE ( 'NONE', #39867, #20338, #36430, .T. ) ;
#38384 = CARTESIAN_POINT ( 'NONE',  ( -0.5756566573089004768, 1.710292258889409833, 2.896516654582634853 ) ) ;
#38385 = VERTEX_POINT ( 'NONE', #40305 ) ;
#38386 = EDGE_LOOP ( 'NONE', ( #4439, #36959, #49231, #27567, #2319, #4704, #46123, #34132, #21160, #20894, #18359, #23686, #2933 ) ) ;
#38387 = EDGE_CURVE ( 'NONE', #42728, #40166, #1051, .T. ) ;
#38388 = ORIENTED_EDGE ( 'NONE', *, *, #14073, .F. ) ;
#38389 = ORIENTED_EDGE ( 'NONE', *, *, #44196, .T. ) ;
#38390 = CARTESIAN_POINT ( 'NONE',  ( 1.909347346926324684, 3.346456692913386100, -0.03937007874015936021 ) ) ;
#38391 = CARTESIAN_POINT ( 'NONE',  ( 1.661821349926414282, 6.692913385826772199, 1.388203579611976712 ) ) ;
#38392 = DIRECTION ( 'NONE',  ( -0.2660368455666687892, 0.000000000000000000, -0.9639628606958549062 ) ) ;
#38393 = ADVANCED_FACE ( 'NONE', ( #17071 ), #11623, .T. ) ;
#38394 = DIRECTION ( 'NONE',  ( -0.01601477604151182663, 0.9998717552508123996, -0.000000000000000000 ) ) ;
#38395 = EDGE_CURVE ( 'NONE', #31182, #40680, #31424, .T. ) ;
#38396 = CARTESIAN_POINT ( 'NONE',  ( -0.5441960870438705689, 1.666377258251801941, -2.156834381528191180 ) ) ;
#38397 = CARTESIAN_POINT ( 'NONE',  ( 1.943616526632303110, 1.647544198063666476, -1.926374208805734956 ) ) ;
#38398 = VECTOR ( 'NONE', #20615, 39.37007874015748143 ) ;
#38399 = EDGE_CURVE ( 'NONE', #26794, #31047, #31403, .T. ) ;
#38400 = ORIENTED_EDGE ( 'NONE', *, *, #39152, .F. ) ;
#38401 = CARTESIAN_POINT ( 'NONE',  ( 0.000000000000000000, 1.574803149606302854, 0.000000000000000000 ) ) ;
#38402 = LINE ( 'NONE', #40113, #33298 ) ;
#38403 = VECTOR ( 'NONE', #11332, 39.37007874015748143 ) ;
#38404 = DIRECTION ( 'NONE',  ( -0.000000000000000000, 1.000000000000000000, -0.000000000000000000 ) ) ;
#38405 = VECTOR ( 'NONE', #35253, 39.37007874015748143 ) ;
#38406 = ORIENTED_EDGE ( 'NONE', *, *, #11063, .F. ) ;
#38407 = LINE ( 'NONE', #50218, #19050 ) ;
#38408 = CARTESIAN_POINT ( 'NONE',  ( -1.790681247139289889, 1.679220913509628543, -1.240985722462402352 ) ) ;
#38409 = VERTEX_POINT ( 'NONE', #25313 ) ;
#38410 = DIRECTION ( 'NONE',  ( 1.734723475976806848E-16, -0.000000000000000000, 1.000000000000000000 ) ) ;
#38411 = AXIS2_PLACEMENT_3D ( 'NONE', #16849, #48290, #12974 ) ;
#38413 = EDGE_CURVE ( 'NONE', #38226, #49191, #21449, .T. ) ;
#38412 = DIRECTION ( 'NONE',  ( 0.000000000000000000, 0.000000000000000000, -1.000000000000000000 ) ) ;
#38414 = VECTOR ( 'NONE', #41535, 39.37007874015748143 ) ;
#38415 = EDGE_LOOP ( 'NONE', ( #39548, #12703, #4949, #46555 ) ) ;
#38416 = CARTESIAN_POINT ( 'NONE',  ( 1.636583440222563857, 3.346456692913386100, 1.574803149606291974 ) ) ;
#38417 = ORIENTED_EDGE ( 'NONE', *, *, #5261, .F. ) ;
#38418 = CARTESIAN_POINT ( 'NONE',  ( -2.456292249654252302, 1.578478270180400322, -1.103389117635475536 ) ) ;
#38419 = CARTESIAN_POINT ( 'NONE',  ( -0.3486774197067339376, 3.267716535433071279, -1.889763779527552146 ) ) ;
#38420 = CARTESIAN_POINT ( 'NONE',  ( -1.712496953225537188, 3.267716535433071279, -0.3543307086614171930 ) ) ;
#38421 = CARTESIAN_POINT ( 'NONE',  ( 1.363819533518803029, 3.267716535433071279, -1.299212598425193210 ) ) ;
#38422 = DIRECTION ( 'NONE',  ( -1.000000000000000000, 0.000000000000000000, 0.000000000000000000 ) ) ;
#38423 = ORIENTED_EDGE ( 'NONE', *, *, #49477, .F. ) ;
#38424 = EDGE_CURVE ( 'NONE', #25218, #8605, #37465, .T. ) ;
#38425 = DIRECTION ( 'NONE',  ( -0.01601477604151182663, 0.9998717552508123996, -0.000000000000000000 ) ) ;
#38426 = ORIENTED_EDGE ( 'NONE', *, *, #33461, .T. ) ;
#38427 = ORIENTED_EDGE ( 'NONE', *, *, #42352, .T. ) ;
#38428 = LINE ( 'NONE', #18554, #21298 ) ;
#38429 = ORIENTED_EDGE ( 'NONE', *, *, #12503, .T. ) ;
#38430 = CARTESIAN_POINT ( 'NONE',  ( -1.166969139818015977, 0.000000000000000000, -0.7874015748031470974 ) ) ;
#38431 = CARTESIAN_POINT ( 'NONE',  ( 0.000000000000000000, 2.755905511811023612, -0.8858267716535433989 ) ) ;
#38432 = ORIENTED_EDGE ( 'NONE', *, *, #1243, .F. ) ;
#38433 = EDGE_CURVE ( 'NONE', #23949, #11818, #37205, .T. ) ;
#38434 = CARTESIAN_POINT ( 'NONE',  ( 0.000000000000000000, 3.267716535433071279, 0.1574803149606287811 ) ) ;
#38435 = EDGE_CURVE ( 'NONE', #9734, #24599, #20721, .T. ) ;
#38436 = DIRECTION ( 'NONE',  ( -0.000000000000000000, 0.000000000000000000, 1.000000000000000000 ) ) ;
#38437 = EDGE_CURVE ( 'NONE', #42646, #10879, #45297, .T. ) ;
#38438 = AXIS2_PLACEMENT_3D ( 'NONE', #50832, #35412, #31286 ) ;
#38439 = EDGE_CURVE ( 'NONE', #39932, #29652, #29957, .T. ) ;
#38440 = PLANE ( 'NONE',  #42827 ) ;
#38441 = MECHANICAL_DESIGN_GEOMETRIC_PRESENTATION_REPRESENTATION (  '', ( #14516 ), #11200 ) ;
#38442 = ORIENTED_EDGE ( 'NONE', *, *, #46054, .F. ) ;
#38443 = VERTEX_POINT ( 'NONE', #13957 ) ;
#38444 = AXIS2_PLACEMENT_3D ( 'NONE', #26257, #46601, #30898 ) ;
#38445 = CARTESIAN_POINT ( 'NONE',  ( 0.1525789431699052512, 1.677537385366203448, -2.244297798459045534 ) ) ;
#38446 = FACE_BOUND ( 'NONE', #44564, .T. ) ;
#38447 = ORIENTED_EDGE ( 'NONE', *, *, #18521, .T. ) ;
#38448 = AXIS2_PLACEMENT_3D ( 'NONE', #37234, #40592, #45447 ) ;
#38449 = DIRECTION ( 'NONE',  ( -0.000000000000000000, 1.000000000000000000, -0.000000000000000000 ) ) ;
#38450 = VECTOR ( 'NONE', #3196, 39.37007874015748143 ) ;
#38451 = ORIENTED_EDGE ( 'NONE', *, *, #37328, .T. ) ;
#38452 = EDGE_LOOP ( 'NONE', ( #41152, #28921, #17020, #39262 ) ) ;
#38453 = FACE_OUTER_BOUND ( 'NONE', #24234, .T. ) ;
#38454 = VECTOR ( 'NONE', #35565, 39.37007874015748143 ) ;
#38455 = CARTESIAN_POINT ( 'NONE',  ( -2.449433152083427156, 3.244423651327855485, -0.1574803149606298636 ) ) ;
#38456 = ORIENTED_EDGE ( 'NONE', *, *, #5511, .T. ) ;
#38457 = EDGE_CURVE ( 'NONE', #31511, #35836, #15144, .T. ) ;
#38458 = PLANE ( 'NONE',  #14709 ) ;
#38459 = VERTEX_POINT ( 'NONE', #38222 ) ;
#38460 = DIRECTION ( 'NONE',  ( -3.469446951953613696E-16, 0.000000000000000000, -1.000000000000000000 ) ) ;
#38461 = CARTESIAN_POINT ( 'NONE',  ( -0.8182917201112819283, 0.000000000000000000, -1.102362204724405492 ) ) ;
#38462 = ADVANCED_FACE ( 'NONE', ( #18336 ), #41328, .F. ) ;
#38463 = CARTESIAN_POINT ( 'NONE',  ( -1.442444474601640492, 0.004816277389180329341, -1.011116641508509995 ) ) ;
#38464 = EDGE_CURVE ( 'NONE', #30125, #49795, #29768, .T. ) ;
#38465 = ORIENTED_EDGE ( 'NONE', *, *, #7527, .F. ) ;
#38466 = ORIENTED_EDGE ( 'NONE', *, *, #17339, .F. ) ;
#38467 = DIRECTION ( 'NONE',  ( -3.469446951953613696E-16, 0.000000000000000000, -1.000000000000000000 ) ) ;
#38468 = LINE ( 'NONE', #6465, #50979 ) ;
#38469 = EDGE_CURVE ( 'NONE', #29102, #15326, #49281, .T. ) ;
#38470 = LINE ( 'NONE', #51025, #17585 ) ;
#38471 = DIRECTION ( 'NONE',  ( 1.000000000000000000, 0.000000000000000000, 0.000000000000000000 ) ) ;
#38472 = CARTESIAN_POINT ( 'NONE',  ( -2.165354330708661568, 1.574803149606301966, -0.01597875172474143637 ) ) ;
#38473 = DIRECTION ( 'NONE',  ( -1.288287287306305283E-16, 1.000000000000000000, 0.000000000000000000 ) ) ;
#38474 = VECTOR ( 'NONE', #10528, 39.37007874015748143 ) ;
#38475 = CARTESIAN_POINT ( 'NONE',  ( 2.734482843737263025, 2.755905511811027164, -1.115254632218672493 ) ) ;
#38476 = EDGE_LOOP ( 'NONE', ( #39706, #46597, #35213, #42103 ) ) ;
#38477 = VECTOR ( 'NONE', #45934, 39.37007874015748143 ) ;
#38478 = DIRECTION ( 'NONE',  ( -3.469446951953613696E-16, 0.000000000000000000, -1.000000000000000000 ) ) ;
#38479 = LINE ( 'NONE', #46185, #23603 ) ;
#38480 = VECTOR ( 'NONE', #13068, 39.37007874015748143 ) ;
#38481 = ORIENTED_EDGE ( 'NONE', *, *, #22560, .F. ) ;
#38482 = EDGE_LOOP ( 'NONE', ( #47991, #38417, #7813, #49113 ) ) ;
#38483 = CARTESIAN_POINT ( 'NONE',  ( -1.790900357307437352, 1.580792207208895128, -1.241130355818072406 ) ) ;
#38484 = DIRECTION ( 'NONE',  ( -0.000000000000000000, 1.000000000000000000, -0.000000000000000000 ) ) ;
#38485 = CONICAL_SURFACE ( 'NONE', #16216, 2.244934639244524632, 1.554780866114618743 ) ;
#38486 = ORIENTED_EDGE ( 'NONE', *, *, #22756, .F. ) ;
#38487 = VECTOR ( 'NONE', #9928, 39.37007874015748143 ) ;
#38488 = EDGE_LOOP ( 'NONE', ( #17138, #40426, #6710, #32746, #26247 ) ) ;
#38489 = CARTESIAN_POINT ( 'NONE',  ( 2.043634885149959057, 5.118110236220475784, 0.7157624142946238388 ) ) ;
#38490 = ORIENTED_EDGE ( 'NONE', *, *, #531, .T. ) ;
#38491 = DIRECTION ( 'NONE',  ( 1.734723475976806848E-16, -0.000000000000000000, 1.000000000000000000 ) ) ;
#38492 = DIRECTION ( 'NONE',  ( 1.734723475976806848E-16, 0.000000000000000000, 1.000000000000000000 ) ) ;
#38493 = EDGE_CURVE ( 'NONE', #23569, #12335, #10085, .T. ) ;
#38494 = ORIENTED_EDGE ( 'NONE', *, *, #39966, .F. ) ;
#38495 = EDGE_CURVE ( 'NONE', #552, #2219, #45671, .T. ) ;
#38496 = CARTESIAN_POINT ( 'NONE',  ( 1.091055626815042645, 3.346456692913386100, 1.062992125984246083 ) ) ;
#38497 = EDGE_CURVE ( 'NONE', #16641, #11793, #41039, .T. ) ;
#38498 = ORIENTED_EDGE ( 'NONE', *, *, #19963, .T. ) ;
#38499 = ORIENTED_EDGE ( 'NONE', *, *, #7554, .T. ) ;
#38500 = CARTESIAN_POINT ( 'NONE',  ( 2.122900538649399316, 1.653866144572175179, -2.052396120437094407 ) ) ;
#38501 = CARTESIAN_POINT ( 'NONE',  ( 1.236813753895252166, 1.640077341046696890, -2.681693691597563767 ) ) ;
#38502 = LINE ( 'NONE', #50305, #24017 ) ;
#38503 = DIRECTION ( 'NONE',  ( -0.1785568947986370392, 0.000000000000000000, 0.9839295885986295565 ) ) ;
#38504 = EDGE_CURVE ( 'NONE', #21474, #45901, #49781, .T. ) ;
#38505 = ORIENTED_EDGE ( 'NONE', *, *, #46841, .T. ) ;
#38506 = FACE_OUTER_BOUND ( 'NONE', #39745, .T. ) ;
#38507 = CARTESIAN_POINT ( 'NONE',  ( 0.8182917201112824834, 3.346456692913386100, 1.850393700787392293 ) ) ;
#38508 = DIRECTION ( 'NONE',  ( 1.734723475976806848E-16, -0.000000000000000000, 1.000000000000000000 ) ) ;
#38509 = AXIS2_PLACEMENT_3D ( 'NONE', #50911, #30600, #23597 ) ;
#38510 = ORIENTED_EDGE ( 'NONE', *, *, #26626, .F. ) ;
#38511 = CYLINDRICAL_SURFACE ( 'NONE', #9280, 2.165354330708661568 ) ;
#38512 = ORIENTED_EDGE ( 'NONE', *, *, #21228, .T. ) ;
#38513 = ORIENTED_EDGE ( 'NONE', *, *, #50160, .T. ) ;
#38514 = EDGE_CURVE ( 'NONE', #26233, #7688, #22217, .T. ) ;
#38515 = DIRECTION ( 'NONE',  ( 0.9639628606958512425, -1.160734090543304660E-16, 0.2660368455666826670 ) ) ;
#38516 = DIRECTION ( 'NONE',  ( -0.000000000000000000, 1.000000000000000000, -0.000000000000000000 ) ) ;
#38517 = ADVANCED_FACE ( 'NONE', ( #34594 ), #3341, .F. ) ;
#38518 = VECTOR ( 'NONE', #33638, 39.37007874015748143 ) ;
#38519 = CARTESIAN_POINT ( 'NONE',  ( 1.905671854841463730, 1.650492703781866632, 2.256015092822682089 ) ) ;
#38520 = DIRECTION ( 'NONE',  ( 1.734723475976806848E-16, 0.000000000000000000, 1.000000000000000000 ) ) ;
#38521 = ORIENTED_EDGE ( 'NONE', *, *, #35178, .F. ) ;
#38522 = ORIENTED_EDGE ( 'NONE', *, *, #24504, .F. ) ;
#38523 = PLANE ( 'NONE',  #9811 ) ;
#38524 = EDGE_CURVE ( 'NONE', #11129, #26516, #8309, .T. ) ;
#38525 = LINE ( 'NONE', #46233, #6154 ) ;
#38526 = ORIENTED_EDGE ( 'NONE', *, *, #3239, .F. ) ;
#38527 = LINE ( 'NONE', #26140, #49639 ) ;
#38528 = CARTESIAN_POINT ( 'NONE',  ( -1.152895553066196843, 6.692913385826772199, -1.833672301139088301 ) ) ;
#38529 = CARTESIAN_POINT ( 'NONE',  ( -0.3486774197067334380, 3.346456692913386100, 0.6299212598425164567 ) ) ;
#38530 = DIRECTION ( 'NONE',  ( 1.734723475976806848E-16, 0.000000000000000000, 1.000000000000000000 ) ) ;
#38531 = CARTESIAN_POINT ( 'NONE',  ( -0.6214413264104939882, 3.346456692913386100, 0.5905511811023582691 ) ) ;
#38532 = ORIENTED_EDGE ( 'NONE', *, *, #10267, .F. ) ;
#38533 = LINE ( 'NONE', #30779, #285 ) ;
#38534 = CARTESIAN_POINT ( 'NONE',  ( 0.7423782071083087075, 0.000000000000000000, -6.146657985744592735E-16 ) ) ;
#38535 = B_SPLINE_CURVE_WITH_KNOTS ( 'NONE', 3,
 ( #20868, #27138, #8738, #28607 ),
 .UNSPECIFIED., .F., .F.,
 ( 4, 4 ),
 ( 2.271247561980464994E-07, 0.002500295238063529428 ),
 .UNSPECIFIED. ) ;
#38536 = CARTESIAN_POINT ( 'NONE',  ( 0.07982360342473591996, 1.709180471932028711, 0.000000000000000000 ) ) ;
#38537 = ORIENTED_EDGE ( 'NONE', *, *, #7384, .T. ) ;
#38538 = LINE ( 'NONE', #3160, #30667 ) ;
#38539 = LINE ( 'NONE', #46496, #13820 ) ;
#38540 = DIRECTION ( 'NONE',  ( 1.000000000000000000, 0.000000000000000000, -3.469446951953613696E-16 ) ) ;
#38541 = VECTOR ( 'NONE', #47277, 39.37007874015748143 ) ;
#38542 = ORIENTED_EDGE ( 'NONE', *, *, #39947, .T. ) ;
#38543 = AXIS2_PLACEMENT_3D ( 'NONE', #1063, #16824, #48012 ) ;
#38544 = LINE ( 'NONE', #18411, #38265 ) ;
#38545 = EDGE_LOOP ( 'NONE', ( #39284, #8591, #37926, #30229 ) ) ;
#38546 = CARTESIAN_POINT ( 'NONE',  ( 0.000000000000000000, 3.267716535433071279, 1.220472440944875281 ) ) ;
#38547 = VERTEX_POINT ( 'NONE', #42581 ) ;
#38548 = DIRECTION ( 'NONE',  ( 1.734723475976806848E-16, -0.000000000000000000, 1.000000000000000000 ) ) ;
#38549 = ORIENTED_EDGE ( 'NONE', *, *, #22592, .F. ) ;
#38550 = CARTESIAN_POINT ( 'NONE',  ( -0.2492758785930729581, 1.703909341437327862, -2.220674960591680680 ) ) ;
#38551 = DIRECTION ( 'NONE',  ( 0.000000000000000000, 0.000000000000000000, -1.000000000000000000 ) ) ;
#38552 = CARTESIAN_POINT ( 'NONE',  ( -1.636583440222563635, 0.000000000000000000, 1.062992125984246083 ) ) ;
#38553 = ORIENTED_EDGE ( 'NONE', *, *, #14482, .F. ) ;
#38554 = EDGE_CURVE ( 'NONE', #22477, #50189, #23459, .T. ) ;
#38555 = EDGE_LOOP ( 'NONE', ( #1565, #37766, #34415, #14162 ) ) ;
#38556 = VERTEX_POINT ( 'NONE', #34346 ) ;
#38557 = CARTESIAN_POINT ( 'NONE',  ( -1.091055626815042645, 3.232777166330607521, 2.204724409448808764 ) ) ;
#38558 = CARTESIAN_POINT ( 'NONE',  ( -0.6214413264104945434, 3.346456692913386100, -1.732283464566922726 ) ) ;
#38559 = EDGE_CURVE ( 'NONE', #37038, #47957, #33636, .T. ) ;
#38560 = EDGE_LOOP ( 'NONE', ( #21681, #39395, #7364, #4736 ) ) ;
#38561 = DIRECTION ( 'NONE',  ( -0.01601477604151182663, 0.9998717552508123996, -0.000000000000000000 ) ) ;
#38562 = LINE ( 'NONE', #46274, #19356 ) ;
#38563 = CARTESIAN_POINT ( 'NONE',  ( -1.743268982565497449, 0.0004610889948519912205, -0.02902809809614041725 ) ) ;
#38564 = CONICAL_SURFACE ( 'NONE', #31146, 2.165354330708661568, 0.2617993877991570129 ) ;
#38565 = EDGE_CURVE ( 'NONE', #16345, #26927, #50772, .T. ) ;
#38566 = ORIENTED_EDGE ( 'NONE', *, *, #25284, .T. ) ;
#38567 = ORIENTED_EDGE ( 'NONE', *, *, #5701, .F. ) ;
#38568 = CARTESIAN_POINT ( 'NONE',  ( 0.8069532150559736161, 1.205361022782829114E-17, -2.010061882867131278 ) ) ;
#38569 = CARTESIAN_POINT ( 'NONE',  ( -0.3486774197067334380, 3.346456692913386100, 1.889763779527550369 ) ) ;
#38570 = FACE_OUTER_BOUND ( 'NONE', #36122, .T. ) ;
#38571 = EDGE_CURVE ( 'NONE', #36108, #41559, #50204, .T. ) ;
#38572 = ORIENTED_EDGE ( 'NONE', *, *, #22832, .F. ) ;
#38573 = DIRECTION ( 'NONE',  ( 1.000000000000000000, 0.000000000000000000, 0.000000000000000000 ) ) ;
#38574 = LINE ( 'NONE', #31326, #38450 ) ;
#38575 = VERTEX_POINT ( 'NONE', #22966 ) ;
#38576 = DIRECTION ( 'NONE',  ( -0.000000000000000000, -1.000000000000000000, -0.000000000000000000 ) ) ;
#38577 = EDGE_LOOP ( 'NONE', ( #43286, #21974, #7514, #44995 ) ) ;
#38578 = ORIENTED_EDGE ( 'NONE', *, *, #3603, .F. ) ;
#38579 = PLANE ( 'NONE',  #18016 ) ;
#38580 = PLANE ( 'NONE',  #26703 ) ;
#38581 = LINE ( 'NONE', #16990, #27216 ) ;
#38582 = EDGE_CURVE ( 'NONE', #21621, #5433, #47041, .T. ) ;
#38583 = CONICAL_SURFACE ( 'NONE', #23743, 2.165354330708661568, 0.2617993877991570129 ) ;
#38584 = CONICAL_SURFACE ( 'NONE', #16309, 2.165354330708661568, 0.2617993877991570129 ) ;
#38585 = CARTESIAN_POINT ( 'NONE',  ( 0.1067246931122726866, 0.02962905676920215767, 0.000000000000000000 ) ) ;
#38586 = DIRECTION ( 'NONE',  ( 1.734723475976806848E-16, 0.000000000000000000, 1.000000000000000000 ) ) ;
#38587 = EDGE_LOOP ( 'NONE', ( #23865, #16274, #39193 ) ) ;
#38588 = EDGE_CURVE ( 'NONE', #39237, #27835, #43330, .T. ) ;
#38589 = VECTOR ( 'NONE', #5159, 39.37007874015748143 ) ;
#38590 = ORIENTED_EDGE ( 'NONE', *, *, #9830, .F. ) ;
#38591 = CARTESIAN_POINT ( 'NONE',  ( -0.2198976605848039223, 1.205361022782829114E-17, -1.894256224240784103 ) ) ;
#38592 = CARTESIAN_POINT ( 'NONE',  ( -1.985260859929297572, 0.000000000000000000, 0.3149606299212578953 ) ) ;
#38593 = VECTOR ( 'NONE', #24223, 39.37007874015748143 ) ;
#38594 = DIRECTION ( 'NONE',  ( -1.000000000000000000, -0.000000000000000000, -0.000000000000000000 ) ) ;
#38595 = DIRECTION ( 'NONE',  ( 0.000000000000000000, 0.000000000000000000, 1.000000000000000000 ) ) ;
#38596 = ORIENTED_EDGE ( 'NONE', *, *, #10650, .T. ) ;
#38597 = CARTESIAN_POINT ( 'NONE',  ( -1.979793062125317471, 1.556934451446513545, 2.191257344206539504 ) ) ;
#38598 = AXIS2_PLACEMENT_3D ( 'NONE', #38286, #10899, #14780 ) ;
#38599 = EDGE_CURVE ( 'NONE', #44295, #13419, #34840, .T. ) ;
#38600 = DIRECTION ( 'NONE',  ( -3.469446951953613696E-16, 0.000000000000000000, -1.000000000000000000 ) ) ;
#38601 = ORIENTED_EDGE ( 'NONE', *, *, #7890, .T. ) ;
#38602 = DIRECTION ( 'NONE',  ( 0.4338837391175656699, 0.000000000000000000, -0.9009688679024154823 ) ) ;
#38603 = DIRECTION ( 'NONE',  ( -3.469446951953613696E-16, 0.000000000000000000, -1.000000000000000000 ) ) ;
#38604 = DIRECTION ( 'NONE',  ( -0.000000000000000000, 1.000000000000000000, -0.000000000000000000 ) ) ;
#38605 = PLANE ( 'NONE',  #3651 ) ;
#38606 = PLANE ( 'NONE',  #1096 ) ;
#38607 = DIRECTION ( 'NONE',  ( 1.000000000000000000, 0.000000000000000000, -3.469446951953613696E-16 ) ) ;
#38608 = ORIENTED_EDGE ( 'NONE', *, *, #23112, .T. ) ;
#38609 = DIRECTION ( 'NONE',  ( 1.734723475976806848E-16, -0.000000000000000000, 1.000000000000000000 ) ) ;
#38610 = EDGE_LOOP ( 'NONE', ( #33128, #47278, #10550, #28343 ) ) ;
#38611 = FACE_BOUND ( 'NONE', #44555, .T. ) ;
#38612 = DIRECTION ( 'NONE',  ( -0.000000000000000000, 1.000000000000000000, -0.000000000000000000 ) ) ;
#38613 = LINE ( 'NONE', #15370, #14458 ) ;
#38614 = VECTOR ( 'NONE', #10549, 39.37007874015748143 ) ;
#38615 = EDGE_LOOP ( 'NONE', ( #9941, #23317, #28176, #16169 ) ) ;
#38616 = ORIENTED_EDGE ( 'NONE', *, *, #49685, .T. ) ;
#38617 = FACE_OUTER_BOUND ( 'NONE', #19782, .T. ) ;
#38618 = CARTESIAN_POINT ( 'NONE',  ( 1.015142113812069091, 3.346456692913386100, -1.732283464566923614 ) ) ;
#38619 = ADVANCED_FACE ( 'NONE', ( #15219 ), #11094, .T. ) ;
#38620 = LINE ( 'NONE', #31124, #46434 ) ;
#38621 = VECTOR ( 'NONE', #33948, 39.37007874015748143 ) ;
#38622 = PLANE ( 'NONE',  #21119 ) ;
#38623 = DIRECTION ( 'NONE',  ( 0.000000000000000000, 0.000000000000000000, -1.000000000000000000 ) ) ;
#38624 = ADVANCED_FACE ( 'NONE', ( #19332 ), #2843, .F. ) ;
#38625 = DIRECTION ( 'NONE',  ( -0.9998717552508122886, -0.01601477604151181275, 0.000000000000000000 ) ) ;
#38626 = VECTOR ( 'NONE', #905, 39.37007874015748143 ) ;
#38627 = AXIS2_PLACEMENT_3D ( 'NONE', #40063, #4432, #20170 ) ;
#38628 = ORIENTED_EDGE ( 'NONE', *, *, #2967, .F. ) ;
#38629 = EDGE_CURVE ( 'NONE', #11828, #35927, #50033, .T. ) ;
#38630 = CARTESIAN_POINT ( 'NONE',  ( 1.091055626815042645, 0.000000000000000000, 0.9448818897637746295 ) ) ;
#38631 = DIRECTION ( 'NONE',  ( -1.000000000000000000, -0.000000000000000000, -0.000000000000000000 ) ) ;
#38632 = ADVANCED_FACE ( 'NONE', ( #11592 ), #31474, .F. ) ;
#38633 = AXIS2_PLACEMENT_3D ( 'NONE', #48380, #5055, #47354 ) ;
#38634 = LINE ( 'NONE', #42743, #45439 ) ;
#38635 = VERTEX_POINT ( 'NONE', #18844 ) ;
#38636 = CARTESIAN_POINT ( 'NONE',  ( -1.909828200256540987, 1.049866565067838042, 0.6722859868850896703 ) ) ;
#38637 = VERTEX_POINT ( 'NONE', #15719 ) ;
#38638 = ORIENTED_EDGE ( 'NONE', *, *, #17711, .F. ) ;
#38639 = VECTOR ( 'NONE', #22655, 39.37007874015748143 ) ;
#38640 = ADVANCED_FACE ( 'NONE', ( #7228 ), #31224, .F. ) ;
#38641 = VERTEX_POINT ( 'NONE', #11345 ) ;
#38642 = VERTEX_POINT ( 'NONE', #7470 ) ;
#38643 = CARTESIAN_POINT ( 'NONE',  ( -0.5272349255865267370, 0.000000000000000000, 2.905303903342410621 ) ) ;
#38644 = ADVANCED_FACE ( 'NONE', ( #27330 ), #7718, .T. ) ;
#38645 = LINE ( 'NONE', #7150, #49303 ) ;
#38646 = CARTESIAN_POINT ( 'NONE',  ( 1.670330979180827180, 3.346456692913386100, 1.377952755905504256 ) ) ;
#38647 = VECTOR ( 'NONE', #29019, 39.37007874015748143 ) ;
#38648 = EDGE_CURVE ( 'NONE', #739, #36398, #44597, .T. ) ;
#38649 = DIRECTION ( 'NONE',  ( -0.000000000000000000, 1.000000000000000000, -0.000000000000000000 ) ) ;
#38650 = DIRECTION ( 'NONE',  ( 0.9998717552508121775, 0.01601477604151182663, 0.000000000000000000 ) ) ;
#38651 = CARTESIAN_POINT ( 'NONE',  ( 2.951990591674676256, 1.447429260878886348, -0.08331184815398369470 ) ) ;
#38652 = VERTEX_POINT ( 'NONE', #24495 ) ;
#38653 = CARTESIAN_POINT ( 'NONE',  ( 1.426808618753927282, 0.05077261674489902399, -1.296082183384024811 ) ) ;
#38654 = CARTESIAN_POINT ( 'NONE',  ( 1.287906020515830141, 3.346456692913386100, -0.1968503937007883287 ) ) ;
#38655 = DIRECTION ( 'NONE',  ( -1.000000000000000000, 0.000000000000000000, -0.000000000000000000 ) ) ;
#38656 = ADVANCED_FACE ( 'NONE', ( #27842 ), #9003, .F. ) ;
#38657 = DIRECTION ( 'NONE',  ( -1.000000000000000000, 0.000000000000000000, 1.734723475976806848E-16 ) ) ;
#38658 = VECTOR ( 'NONE', #9932, 39.37007874015748143 ) ;
#38659 = VECTOR ( 'NONE', #10552, 39.37007874015748854 ) ;
#38660 = ORIENTED_EDGE ( 'NONE', *, *, #39737, .F. ) ;
#38661 = CARTESIAN_POINT ( 'NONE',  ( 0.9432913529151772947, 1.723010488186151878, -2.072188145589165753 ) ) ;
#38662 = FACE_OUTER_BOUND ( 'NONE', #31956, .T. ) ;
#38663 = ORIENTED_EDGE ( 'NONE', *, *, #37965, .T. ) ;
#38664 = LINE ( 'NONE', #39671, #15552 ) ;
#38665 = CARTESIAN_POINT ( 'NONE',  ( 0.04921259842519669359, 1.621581020286960051, 2.952755905511811108 ) ) ;
#38666 = AXIS2_PLACEMENT_3D ( 'NONE', #21, #4410, #46971 ) ;
#38667 = EDGE_CURVE ( 'NONE', #49919, #10750, #39984, .T. ) ;
#38668 = CARTESIAN_POINT ( 'NONE',  ( -1.636583440222564301, 3.267716535433071279, -1.574803149606293307 ) ) ;
#38669 = AXIS2_PLACEMENT_3D ( 'NONE', #23098, #46315, #19217 ) ;
#38670 = ORIENTED_EDGE ( 'NONE', *, *, #27877, .F. ) ;
#38671 = DIRECTION ( 'NONE',  ( 1.734723475976806848E-16, -0.000000000000000000, 1.000000000000000000 ) ) ;
#38672 = EDGE_CURVE ( 'NONE', #33027, #10178, #4089, .T. ) ;
#38673 = CARTESIAN_POINT ( 'NONE',  ( 1.636583440222563857, 3.346456692913386100, 1.259842519685033135 ) ) ;
#38674 = CARTESIAN_POINT ( 'NONE',  ( 0.08139965876239094178, 1.610780518492231694, 0.000000000000000000 ) ) ;
#38675 = DIRECTION ( 'NONE',  ( 1.000000000000000000, 0.000000000000000000, -3.469446951953613696E-16 ) ) ;
#38676 = LINE ( 'NONE', #11550, #3688 ) ;
#38677 = ORIENTED_EDGE ( 'NONE', *, *, #24290, .F. ) ;
#38678 = CARTESIAN_POINT ( 'NONE',  ( 0.000000000000000000, 3.267716535433071279, 0.9055118110236167750 ) ) ;
#38679 = ORIENTED_EDGE ( 'NONE', *, *, #13325, .T. ) ;
#38680 = ORIENTED_EDGE ( 'NONE', *, *, #17998, .F. ) ;
#38681 = CARTESIAN_POINT ( 'NONE',  ( 2.182111253630085290, 0.000000000000000000, 0.4330708661417287386 ) ) ;
#38682 = ORIENTED_EDGE ( 'NONE', *, *, #15739, .F. ) ;
#38683 = DIRECTION ( 'NONE',  ( 0.000000000000000000, -1.000000000000000000, 0.000000000000000000 ) ) ;
#38684 = DIRECTION ( 'NONE',  ( -0.000000000000000000, 1.000000000000000000, -0.000000000000000000 ) ) ;
#38685 = ORIENTED_EDGE ( 'NONE', *, *, #3106, .T. ) ;
#38686 = EDGE_CURVE ( 'NONE', #13181, #7908, #43586, .T. ) ;
#38687 = LINE ( 'NONE', #3308, #47867 ) ;
#38688 = CIRCLE ( 'NONE', #25484, 2.164630168518208109 ) ;
#38689 = CARTESIAN_POINT ( 'NONE',  ( -3.927031490892378253E-16, 0.000000000000000000, -1.889763779527552146 ) ) ;
#38690 = ADVANCED_FACE ( 'NONE', ( #12106 ), #48447, .F. ) ;
#38691 = FACE_OUTER_BOUND ( 'NONE', #31722, .T. ) ;
#38692 = EDGE_LOOP ( 'NONE', ( #22767, #44471, #19414, #29621 ) ) ;
#38693 = ORIENTED_EDGE ( 'NONE', *, *, #47592, .T. ) ;
#38694 = CARTESIAN_POINT ( 'NONE',  ( 0.5455278134075217666, 0.000000000000000000, 2.204724409448808764 ) ) ;
#38695 = FACE_BOUND ( 'NONE', #34909, .T. ) ;
#38696 = VERTEX_POINT ( 'NONE', #9254 ) ;
#38697 = VECTOR ( 'NONE', #46046, 39.37007874015748143 ) ;
#38698 = DIRECTION ( 'NONE',  ( -3.986037398843765983E-20, -1.000000000000000000, -1.160734090543304660E-16 ) ) ;
#38699 = ORIENTED_EDGE ( 'NONE', *, *, #3523, .F. ) ;
#38700 = ORIENTED_EDGE ( 'NONE', *, *, #14731, .T. ) ;
#38701 = AXIS2_PLACEMENT_3D ( 'NONE', #33737, #6358, #42470 ) ;
#38702 = CARTESIAN_POINT ( 'NONE',  ( 0.4696143004045484348, 3.267716535433071279, 1.850393700787392293 ) ) ;
#38703 = CARTESIAN_POINT ( 'NONE',  ( -2.438548951736694725, 3.267716535433071279, -0.1574803149606298636 ) ) ;
#38704 = VERTEX_POINT ( 'NONE', #8233 ) ;
#38705 = AXIS2_PLACEMENT_3D ( 'NONE', #29786, #6032, #5529 ) ;
#38706 = FACE_OUTER_BOUND ( 'NONE', #16153, .T. ) ;
#38707 = ORIENTED_EDGE ( 'NONE', *, *, #41574, .F. ) ;
#38708 = DIRECTION ( 'NONE',  ( -0.000000000000000000, 1.000000000000000000, -0.000000000000000000 ) ) ;
#38709 = CARTESIAN_POINT ( 'NONE',  ( -1.985260859929297572, 3.346456692913386100, 0.8645800689071783118 ) ) ;
#38710 = EDGE_CURVE ( 'NONE', #1008, #49945, #20088, .T. ) ;
#38711 = DIRECTION ( 'NONE',  ( -0.9998717552508121775, -0.01601477604151182316, 0.000000000000000000 ) ) ;
#38712 = ORIENTED_EDGE ( 'NONE', *, *, #41310, .F. ) ;
#38713 = ORIENTED_EDGE ( 'NONE', *, *, #44032, .T. ) ;
#38714 = DIRECTION ( 'NONE',  ( 1.734723475976806848E-16, -0.000000000000000000, 1.000000000000000000 ) ) ;
#38715 = CARTESIAN_POINT ( 'NONE',  ( -1.909347346926324906, 0.000000000000000000, -1.299212598425193210 ) ) ;
#38716 = CARTESIAN_POINT ( 'NONE',  ( -1.363819533518803473, 0.000000000000000000, -1.732283464566922726 ) ) ;
#38717 = DIRECTION ( 'NONE',  ( 0.000000000000000000, -1.000000000000000000, 0.000000000000000000 ) ) ;
#38718 = EDGE_CURVE ( 'NONE', #43660, #36491, #28092, .T. ) ;
#38719 = DIRECTION ( 'NONE',  ( 1.734723475976806848E-16, -0.000000000000000000, 1.000000000000000000 ) ) ;
#38720 = EDGE_CURVE ( 'NONE', #49994, #35361, #43839, .T. ) ;
#38721 = LINE ( 'NONE', #30469, #42482 ) ;
#38722 = VECTOR ( 'NONE', #34563, 39.37007874015748143 ) ;
#38723 = EDGE_CURVE ( 'NONE', #39358, #25903, #19833, .T. ) ;
#38724 = DIRECTION ( 'NONE',  ( -0.000000000000000000, 1.000000000000000000, -0.000000000000000000 ) ) ;
#38725 = VERTEX_POINT ( 'NONE', #32506 ) ;
#38726 = CARTESIAN_POINT ( 'NONE',  ( 0.000000000000000000, 3.267716535433071279, 0.5905511811023579360 ) ) ;
#38727 = LINE ( 'NONE', #26341, #9617 ) ;
#38728 = ORIENTED_EDGE ( 'NONE', *, *, #26359, .F. ) ;
#38729 = VERTEX_POINT ( 'NONE', #995 ) ;
#38730 = CARTESIAN_POINT ( 'NONE',  ( -0.6214413264104945434, 3.346456692913386100, 2.012537465693970962 ) ) ;
#38731 = DIRECTION ( 'NONE',  ( 0.000000000000000000, 0.000000000000000000, 1.000000000000000000 ) ) ;
#38732 = VERTEX_POINT ( 'NONE', #28867 ) ;
#38733 = EDGE_CURVE ( 'NONE', #7184, #40673, #43473, .T. ) ;
#38734 = DIRECTION ( 'NONE',  ( 1.558091277195102803E-17, -1.000000000000000000, 1.150229170499808965E-16 ) ) ;
#38735 = VERTEX_POINT ( 'NONE', #48200 ) ;
#38736 = CARTESIAN_POINT ( 'NONE',  ( -0.8942052331142547050, 3.346456692913386100, 0.6299212598425164567 ) ) ;
#38737 = VECTOR ( 'NONE', #11115, 39.37007874015748143 ) ;
#38738 = ORIENTED_EDGE ( 'NONE', *, *, #5321, .T. ) ;
#38739 = EDGE_CURVE ( 'NONE', #40626, #31520, #20064, .T. ) ;
#38740 = LINE ( 'NONE', #15238, #44938 ) ;
#38741 = CARTESIAN_POINT ( 'NONE',  ( -1.636583440222564301, 3.346456692913386100, -0.5118110236220466680 ) ) ;
#38742 = EDGE_CURVE ( 'NONE', #11117, #45160, #15971, .T. ) ;
#38743 = EDGE_CURVE ( 'NONE', #4494, #46953, #8741, .T. ) ;
#38744 = ORIENTED_EDGE ( 'NONE', *, *, #10183, .T. ) ;
#38745 = DIRECTION ( 'NONE',  ( -0.01601477604151182663, 0.9998717552508123996, -0.000000000000000000 ) ) ;
#38746 = VERTEX_POINT ( 'NONE', #47942 ) ;
#38747 = ORIENTED_EDGE ( 'NONE', *, *, #31430, .T. ) ;
#38748 = CARTESIAN_POINT ( 'NONE',  ( -0.07591351300297340121, 0.000000000000000000, 0.2755905511810995412 ) ) ;
#38749 = DIRECTION ( 'NONE',  ( 0.000000000000000000, 1.160734090543304660E-16, -1.000000000000000000 ) ) ;
#38750 = DIRECTION ( 'NONE',  ( 1.000000000000000000, 0.000000000000000000, 0.000000000000000000 ) ) ;
#38751 = ORIENTED_EDGE ( 'NONE', *, *, #12858, .F. ) ;
#38752 = CYLINDRICAL_SURFACE ( 'NONE', #14662, 2.165354330708661568 ) ;
#38753 = FACE_OUTER_BOUND ( 'NONE', #17386, .T. ) ;
#38754 = VECTOR ( 'NONE', #10440, 39.37007874015748143 ) ;
#38755 = ORIENTED_EDGE ( 'NONE', *, *, #33959, .F. ) ;
#38756 = CARTESIAN_POINT ( 'NONE',  ( 0.1968503937007873017, 3.346456692913386100, -1.574803149606293529 ) ) ;
#38757 = ORIENTED_EDGE ( 'NONE', *, *, #6132, .T. ) ;
#38758 = ORIENTED_EDGE ( 'NONE', *, *, #35548, .T. ) ;
#38759 = ORIENTED_EDGE ( 'NONE', *, *, #3612, .T. ) ;
#38760 = CARTESIAN_POINT ( 'NONE',  ( 1.091055626815042645, 3.346456692913386100, 0.3149606299212578953 ) ) ;
#38761 = VECTOR ( 'NONE', #38213, 39.37007874015748143 ) ;
#38762 = DIRECTION ( 'NONE',  ( 0.000000000000000000, 0.000000000000000000, -1.000000000000000000 ) ) ;
#38763 = AXIS2_PLACEMENT_3D ( 'NONE', #32108, #24605, #29234 ) ;
#38764 = CARTESIAN_POINT ( 'NONE',  ( -2.047355983664255863, 1.576684601009278319, 0.7169714724935087879 ) ) ;
#38765 = DIRECTION ( 'NONE',  ( 0.000000000000000000, 1.000000000000000000, 0.000000000000000000 ) ) ;
#38766 = ORIENTED_EDGE ( 'NONE', *, *, #20469, .T. ) ;
#38767 = ORIENTED_EDGE ( 'NONE', *, *, #40433, .T. ) ;
#38768 = CARTESIAN_POINT ( 'NONE',  ( -0.2810210260976235830, 1.616428356993893978, -2.939398529254692694 ) ) ;
#38769 = DIRECTION ( 'NONE',  ( -0.01601477604151182663, 0.9998717552508123996, -0.000000000000000000 ) ) ;
#38770 = VECTOR ( 'NONE', #12129, 39.37007874015748143 ) ;
#38771 = ORIENTED_EDGE ( 'NONE', *, *, #44327, .F. ) ;
#38772 = PLANE ( 'NONE',  #25799 ) ;
#38773 = CARTESIAN_POINT ( 'NONE',  ( -1.985260859929297572, 3.267716535433071279, 0.8645800689071783118 ) ) ;
#38774 = EDGE_CURVE ( 'NONE', #11918, #38951, #2807, .T. ) ;
#38775 = CARTESIAN_POINT ( 'NONE',  ( -0.2727639067037608278, 3.267716535433071279, 2.165354330708650465 ) ) ;
#38776 = ADVANCED_FACE ( 'NONE', ( #1252 ), #10018, .T. ) ;
#38777 = CARTESIAN_POINT ( 'NONE',  ( 1.929629134066521923, 1.574803149606302854, 0.9824921284572415425 ) ) ;
#38778 = LINE ( 'NONE', #2649, #35316 ) ;
#38779 = ORIENTED_EDGE ( 'NONE', *, *, #39861, .F. ) ;
#38780 = CARTESIAN_POINT ( 'NONE',  ( -0.3486774197067334935, 0.000000000000000000, 1.692913385826762873 ) ) ;
#38781 = DIRECTION ( 'NONE',  ( -0.9998717552508121775, -0.01601477604151182663, 0.000000000000000000 ) ) ;
#38783 = EDGE_CURVE ( 'NONE', #49887, #17928, #10268, .T. ) ;
#38782 = VERTEX_POINT ( 'NONE', #26017 ) ;
#38784 = DIRECTION ( 'NONE',  ( 1.000000000000000000, 0.000000000000000000, 0.000000000000000000 ) ) ;
#38785 = CARTESIAN_POINT ( 'NONE',  ( -2.030479360727987181, 0.8677437501918839891, -0.7281234607424019734 ) ) ;
#38786 = CARTESIAN_POINT ( 'NONE',  ( 0.5439123932328762123, 0.000000000000000000, -1.909459815214741729 ) ) ;
#38787 = B_SPLINE_CURVE_WITH_KNOTS ( 'NONE', 3,
 ( #43292, #27293, #23421, #39177 ),
 .UNSPECIFIED., .F., .F.,
 ( 4, 4 ),
 ( 0.01204075435466551991, 0.03073748598634059442 ),
 .UNSPECIFIED. ) ;
#38788 = ORIENTED_EDGE ( 'NONE', *, *, #50720, .F. ) ;
#38789 = DIRECTION ( 'NONE',  ( -3.469446951953613696E-16, 0.000000000000000000, -1.000000000000000000 ) ) ;
#38790 = ORIENTED_EDGE ( 'NONE', *, *, #5812, .F. ) ;
#38791 = FACE_OUTER_BOUND ( 'NONE', #34556, .T. ) ;
#38793 = ORIENTED_EDGE ( 'NONE', *, *, #26592, .F. ) ;
#38792 = ADVANCED_FACE ( 'NONE', ( #41765 ), #2014, .F. ) ;
#38794 = PLANE ( 'NONE',  #31198 ) ;
#38795 = ORIENTED_EDGE ( 'NONE', *, *, #12392, .F. ) ;
#38796 = AXIS2_PLACEMENT_3D ( 'NONE', #48133, #47357, #414 ) ;
#38797 = CARTESIAN_POINT ( 'NONE',  ( -0.2922236155267554092, 1.710885387309459160, -2.697863400512623855 ) ) ;
#38798 = ADVANCED_FACE ( 'NONE', ( #37141 ), #10786, .T. ) ;
#38799 = FACE_OUTER_BOUND ( 'NONE', #48683, .T. ) ;
#38800 = LINE ( 'NONE', #38552, #14488 ) ;
#38801 = AXIS2_PLACEMENT_3D ( 'NONE', #3946, #19678, #46273 ) ;
#38802 = EDGE_CURVE ( 'NONE', #36553, #19989, #17763, .T. ) ;
#38803 = ORIENTED_EDGE ( 'NONE', *, *, #19650, .T. ) ;
#38804 = EDGE_LOOP ( 'NONE', ( #48747, #30674, #34741, #11223 ) ) ;
#38805 = ORIENTED_EDGE ( 'NONE', *, *, #47966, .F. ) ;
#38806 = CARTESIAN_POINT ( 'NONE',  ( -0.5455278134075208785, 0.000000000000000000, 1.259842519685033357 ) ) ;
#38807 = CARTESIAN_POINT ( 'NONE',  ( -1.195183497228115035E-16, 3.346456692913386100, -1.259842519685035134 ) ) ;
#38809 = ORIENTED_EDGE ( 'NONE', *, *, #37710, .F. ) ;
#38808 = EDGE_CURVE ( 'NONE', #18704, #2485, #48702, .T. ) ;
#38810 = ORIENTED_EDGE ( 'NONE', *, *, #15642, .T. ) ;
#38811 = LINE ( 'NONE', #50368, #8278 ) ;
#38812 = CARTESIAN_POINT ( 'NONE',  ( 2.182111253630085290, 3.267716535433071279, -0.5118110236220471121 ) ) ;
#38813 = CARTESIAN_POINT ( 'NONE',  ( -1.172858943013145749, 5.905511811023623991, 1.867085387823100850 ) ) ;
#38814 = B_SPLINE_CURVE_WITH_KNOTS ( 'NONE', 3,
 ( #7906, #3274, #19772, #27777 ),
 .UNSPECIFIED., .F., .F.,
 ( 4, 4 ),
 ( 6.300333842480880930E-07, 0.002724228881262062436 ),
 .UNSPECIFIED. ) ;
#38815 = EDGE_CURVE ( 'NONE', #35947, #2241, #17264, .T. ) ;
#38816 = ORIENTED_EDGE ( 'NONE', *, *, #21830, .F. ) ;
#38817 = ORIENTED_EDGE ( 'NONE', *, *, #33795, .F. ) ;
#38818 = CARTESIAN_POINT ( 'NONE',  ( 2.734482843737263025, 1.663397001319319113, -1.115254632218672493 ) ) ;
#38819 = LINE ( 'NONE', #15317, #45558 ) ;
#38820 = LINE ( 'NONE', #45518, #16267 ) ;
#38821 = VERTEX_POINT ( 'NONE', #21894 ) ;
#38822 = CARTESIAN_POINT ( 'NONE',  ( -1.536664496436148184E-16, 3.346456692913386100, -1.771653543307081025 ) ) ;
#38823 = ORIENTED_EDGE ( 'NONE', *, *, #38514, .F. ) ;
#38824 = CARTESIAN_POINT ( 'NONE',  ( 2.947574761915768171, 1.666714435463287236, -0.1816379373804911379 ) ) ;
#38825 = ORIENTED_EDGE ( 'NONE', *, *, #18724, .T. ) ;
#38826 = ORIENTED_EDGE ( 'NONE', *, *, #9069, .T. ) ;
#38827 = FACE_OUTER_BOUND ( 'NONE', #537, .T. ) ;
#38828 = DIRECTION ( 'NONE',  ( 0.01601477604151182663, -0.9998717552508123996, 0.000000000000000000 ) ) ;
#38829 = DIRECTION ( 'NONE',  ( -0.000000000000000000, 1.000000000000000000, -0.000000000000000000 ) ) ;
#38830 = PLANE ( 'NONE',  #3831 ) ;
#38831 = CARTESIAN_POINT ( 'NONE',  ( 0.08139965876239094178, 1.610780518492231694, 0.000000000000000000 ) ) ;
#38832 = ORIENTED_EDGE ( 'NONE', *, *, #38906, .T. ) ;
#38833 = PRODUCT_DEFINITION_SHAPE ( 'NONE', 'NONE',  #51058 ) ;
#38834 = ORIENTED_EDGE ( 'NONE', *, *, #48596, .T. ) ;
#38835 = DIRECTION ( 'NONE',  ( -3.469446951953613696E-16, 0.000000000000000000, -1.000000000000000000 ) ) ;
#38836 = LINE ( 'NONE', #22335, #34211 ) ;
#38837 = AXIS2_PLACEMENT_3D ( 'NONE', #30145, #2526, #49461 ) ;
#38838 = VECTOR ( 'NONE', #30494, 39.37007874015748143 ) ;
#38839 = EDGE_CURVE ( 'NONE', #17350, #51046, #37652, .T. ) ;
#38840 = DIRECTION ( 'NONE',  ( 0.7818314824680221431, 0.000000000000000000, 0.6234898018587431423 ) ) ;
#38841 = PLANE ( 'NONE',  #6428 ) ;
#38842 = ORIENTED_EDGE ( 'NONE', *, *, #25570, .F. ) ;
#38843 = EDGE_CURVE ( 'NONE', #20385, #4443, #9511, .T. ) ;
#38844 = CARTESIAN_POINT ( 'NONE',  ( -1.901641471869980782, 6.692913385826772199, 1.079202499698819429 ) ) ;
#38845 = VECTOR ( 'NONE', #15745, 39.37007874015748143 ) ;
#38846 = CARTESIAN_POINT ( 'NONE',  ( 2.164823134740037069, 1.574803149606302854, -0.04796011690015113127 ) ) ;
#38847 = EDGE_CURVE ( 'NONE', #47095, #41290, #33021, .T. ) ;
#38848 = ORIENTED_EDGE ( 'NONE', *, *, #43267, .F. ) ;
#38849 = VECTOR ( 'NONE', #682, 39.37007874015748143 ) ;
#38850 = CARTESIAN_POINT ( 'NONE',  ( 0.8182917201112819283, 3.346456692913386100, -0.4724409448818889246 ) ) ;
#38851 = CARTESIAN_POINT ( 'NONE',  ( -1.232620761116185681, 6.692913385826772199, -1.780282403660753410 ) ) ;
#38852 = DIRECTION ( 'NONE',  ( 0.2225209339563041788, 0.000000000000000000, 0.9749279121818259508 ) ) ;
#38853 = FACE_OUTER_BOUND ( 'NONE', #13055, .T. ) ;
#38854 = FACE_OUTER_BOUND ( 'NONE', #8286, .T. ) ;
#38855 = DIRECTION ( 'NONE',  ( -1.000000000000000000, 0.000000000000000000, -0.000000000000000000 ) ) ;
#38856 = ORIENTED_EDGE ( 'NONE', *, *, #27488, .T. ) ;
#38857 = DIRECTION ( 'NONE',  ( -0.9998717552508122886, -0.01601477604151185785, 0.000000000000000000 ) ) ;
#38858 = ORIENTED_EDGE ( 'NONE', *, *, #32564, .T. ) ;
#38859 = FACE_OUTER_BOUND ( 'NONE', #43315, .T. ) ;
#38860 = CARTESIAN_POINT ( 'NONE',  ( -1.091055626815042645, 3.346456692913386100, 1.889763779527550147 ) ) ;
#38861 = EDGE_CURVE ( 'NONE', #37431, #13717, #25638, .T. ) ;
#38862 = CARTESIAN_POINT ( 'NONE',  ( 1.566245445154855531, 1.172985819482486924, -0.9842519685039369248 ) ) ;
#38863 = VERTEX_POINT ( 'NONE', #25256 ) ;
#38864 = ORIENTED_EDGE ( 'NONE', *, *, #47270, .F. ) ;
#38865 = DIRECTION ( 'NONE',  ( -0.000000000000000000, 0.000000000000000000, 1.000000000000000000 ) ) ;
#38866 = CARTESIAN_POINT ( 'NONE',  ( -1.530693736245496872, 1.574803149606302854, -1.531579597454065800 ) ) ;
#38867 = EDGE_CURVE ( 'NONE', #814, #5850, #32247, .T. ) ;
#38868 = DIRECTION ( 'NONE',  ( -0.000000000000000000, 0.000000000000000000, 1.000000000000000000 ) ) ;
#38869 = FACE_OUTER_BOUND ( 'NONE', #41599, .T. ) ;
#38870 = FACE_OUTER_BOUND ( 'NONE', #18127, .T. ) ;
#38871 = AXIS2_PLACEMENT_3D ( 'NONE', #6654, #22399, #936 ) ;
#38872 = CARTESIAN_POINT ( 'NONE',  ( -2.182111253630085290, 0.000000000000000000, 0.6299212598425164567 ) ) ;
#38873 = VECTOR ( 'NONE', #46033, 39.37007874015748143 ) ;
#38874 = ORIENTED_EDGE ( 'NONE', *, *, #20800, .T. ) ;
#38875 = ORIENTED_EDGE ( 'NONE', *, *, #28829, .F. ) ;
#38876 = CARTESIAN_POINT ( 'NONE',  ( 1.412396057062171639, 5.905511811023623991, 1.691415513056039321 ) ) ;
#38877 = CARTESIAN_POINT ( 'NONE',  ( -0.8942052331142547050, 3.346456692913386100, 0.9448818897637749625 ) ) ;
#38878 = VECTOR ( 'NONE', #45625, 39.37007874015748143 ) ;
#38879 = ORIENTED_EDGE ( 'NONE', *, *, #41590, .F. ) ;
#38880 = FACE_OUTER_BOUND ( 'NONE', #17376, .T. ) ;
#38881 = ORIENTED_EDGE ( 'NONE', *, *, #27947, .T. ) ;
#38882 = AXIS2_PLACEMENT_3D ( 'NONE', #19305, #50748, #23953 ) ;
#38883 = VERTEX_POINT ( 'NONE', #14140 ) ;
#38884 = EDGE_CURVE ( 'NONE', #2673, #13810, #916, .T. ) ;
#38885 = VECTOR ( 'NONE', #874, 39.37007874015748143 ) ;
#38886 = ORIENTED_EDGE ( 'NONE', *, *, #24977, .F. ) ;
#38887 = ORIENTED_EDGE ( 'NONE', *, *, #19963, .F. ) ;
#38888 = CARTESIAN_POINT ( 'NONE',  ( -0.2480359799030329715, 0.000000000000000000, 0.2799391584775194342 ) ) ;
#38889 = FACE_OUTER_BOUND ( 'NONE', #6047, .T. ) ;
#38890 = LINE ( 'NONE', #34768, #45015 ) ;
#38891 = CARTESIAN_POINT ( 'NONE',  ( 2.278027606577265107, 1.645963535160160696, -0.4694667435916627385 ) ) ;
#38892 = LINE ( 'NONE', #34271, #11562 ) ;
#38893 = DIRECTION ( 'NONE',  ( 0.000000000000000000, 1.000000000000000000, 0.000000000000000000 ) ) ;
#38894 = CARTESIAN_POINT ( 'NONE',  ( 2.620071330711824853, 0.9846937227970387063, -0.06840533695594305796 ) ) ;
#38895 = ORIENTED_EDGE ( 'NONE', *, *, #18843, .T. ) ;
#38896 = EDGE_CURVE ( 'NONE', #11695, #22651, #34028, .T. ) ;
#38897 = LINE ( 'NONE', #50212, #22522 ) ;
#38898 = DIRECTION ( 'NONE',  ( 1.000000000000000000, 0.000000000000000000, 0.000000000000000000 ) ) ;
#38899 = CARTESIAN_POINT ( 'NONE',  ( 1.748857742733975096, 1.746506983082525499, -2.379187494648852930 ) ) ;
#38900 = LINE ( 'NONE', #39154, #28983 ) ;
#38901 = EDGE_CURVE ( 'NONE', #32706, #33100, #48954, .T. ) ;
#38902 = VECTOR ( 'NONE', #8107, 39.37007874015748143 ) ;
#38903 = ORIENTED_EDGE ( 'NONE', *, *, #18349, .T. ) ;
#38904 = VECTOR ( 'NONE', #16340, 39.37007874015748143 ) ;
#38905 = LINE ( 'NONE', #18531, #33923 ) ;
#38906 = EDGE_CURVE ( 'NONE', #49994, #3958, #14395, .T. ) ;
#38907 = LINE ( 'NONE', #46870, #28580 ) ;
#38908 = ORIENTED_EDGE ( 'NONE', *, *, #17584, .T. ) ;
#38909 = CARTESIAN_POINT ( 'NONE',  ( -0.6214413264104945434, 3.346456692913386100, -0.7874015748031467643 ) ) ;
#38910 = EDGE_CURVE ( 'NONE', #5972, #27664, #29383, .T. ) ;
#38911 = CARTESIAN_POINT ( 'NONE',  ( 1.472219874544873131, 1.482402307789154161, 2.560030851058970214 ) ) ;
#38912 = VECTOR ( 'NONE', #38314, 39.37007874015748143 ) ;
#38913 = VECTOR ( 'NONE', #40727, 39.37007874015748143 ) ;
#38914 = CARTESIAN_POINT ( 'NONE',  ( -1.985260859929297794, 3.346456692913386100, 0.4330708661417290162 ) ) ;
#38915 = ORIENTED_EDGE ( 'NONE', *, *, #46856, .T. ) ;
#38916 = DIRECTION ( 'NONE',  ( 1.734723475976806848E-16, -0.000000000000000000, 1.000000000000000000 ) ) ;
#38917 = DIRECTION ( 'NONE',  ( -0.9998717552508121775, -0.01601477604151182316, 0.000000000000000000 ) ) ;
#38918 = AXIS2_PLACEMENT_3D ( 'NONE', #1833, #32317, #25076 ) ;
#38919 = LINE ( 'NONE', #3047, #2030 ) ;
#38920 = EDGE_CURVE ( 'NONE', #24951, #14359, #41013, .T. ) ;
#38921 = LINE ( 'NONE', #35812, #9485 ) ;
#38922 = VERTEX_POINT ( 'NONE', #5636 ) ;
#38923 = EDGE_LOOP ( 'NONE', ( #4972, #38429, #5202, #46534 ) ) ;
#38924 = ORIENTED_EDGE ( 'NONE', *, *, #34767, .T. ) ;
#38925 = CARTESIAN_POINT ( 'NONE',  ( -3.414809992080329023E-17, 0.000000000000000000, -0.1968503937007874405 ) ) ;
#38926 = VERTEX_POINT ( 'NONE', #23399 ) ;
#38927 = EDGE_CURVE ( 'NONE', #2445, #14797, #17432, .T. ) ;
#38928 = CARTESIAN_POINT ( 'NONE',  ( 1.751183565766393890, 0.5249316497054296038, -0.6949723510457602726 ) ) ;
#38929 = DIRECTION ( 'NONE',  ( -0.1342332658176667026, -1.150175664618034464E-16, 0.9909497617679331460 ) ) ;
#38930 = ORIENTED_EDGE ( 'NONE', *, *, #30409, .T. ) ;
#38931 = LINE ( 'NONE', #50487, #3317 ) ;
#38932 = ORIENTED_EDGE ( 'NONE', *, *, #21027, .F. ) ;
#38933 = EDGE_CURVE ( 'NONE', #22477, #20197, #27014, .T. ) ;
#38934 = PLANE ( 'NONE',  #988 ) ;
#38935 = ORIENTED_EDGE ( 'NONE', *, *, #49010, .F. ) ;
#38936 = VERTEX_POINT ( 'NONE', #2776 ) ;
#38937 = LINE ( 'NONE', #3826, #14999 ) ;
#38938 = ORIENTED_EDGE ( 'NONE', *, *, #4675, .F. ) ;
#38939 = EDGE_CURVE ( 'NONE', #35652, #18885, #10000, .T. ) ;
#38940 = VECTOR ( 'NONE', #44398, 39.37007874015748143 ) ;
#38941 = DIRECTION ( 'NONE',  ( 1.000000000000000000, 0.000000000000000000, 0.000000000000000000 ) ) ;
#38942 = EDGE_LOOP ( 'NONE', ( #26947, #38066, #41305, #37932 ) ) ;
#38943 = VERTEX_POINT ( 'NONE', #38158 ) ;
#38944 = CARTESIAN_POINT ( 'NONE',  ( 2.074656761899007051, 5.905511811023623991, -0.6223516566630625801 ) ) ;
#38945 = CONICAL_SURFACE ( 'NONE', #16703, 2.165354330708661568, 0.2617993877991570129 ) ;
#38946 = CARTESIAN_POINT ( 'NONE',  ( -1.636583440222563635, 0.000000000000000000, 1.259842519685033357 ) ) ;
#38947 = EDGE_CURVE ( 'NONE', #50130, #24742, #39738, .T. ) ;
#38948 = ORIENTED_EDGE ( 'NONE', *, *, #13447, .F. ) ;
#38949 = VECTOR ( 'NONE', #42988, 39.37007874015748854 ) ;
#38950 = DIRECTION ( 'NONE',  ( -0.9998717552508121775, -0.01601477604151182663, 0.000000000000000000 ) ) ;
#38951 = VERTEX_POINT ( 'NONE', #23149 ) ;
#38952 = CARTESIAN_POINT ( 'NONE',  ( -2.168245791271168343, 1.560742704294596495, -2.004968704497279486 ) ) ;
#38953 = AXIS2_PLACEMENT_3D ( 'NONE', #13020, #28238, #8632 ) ;
#38954 = DIRECTION ( 'NONE',  ( -0.9998717552508122886, -0.01601477604151185785, 0.000000000000000000 ) ) ;
#38955 = CARTESIAN_POINT ( 'NONE',  ( 0.9834642517162937025, 3.346456692913386100, -1.929133858267711110 ) ) ;
#38956 = EDGE_LOOP ( 'NONE', ( #19120, #36673, #21804, #7237 ) ) ;
#38957 = ORIENTED_EDGE ( 'NONE', *, *, #28475, .T. ) ;
#38958 = CARTESIAN_POINT ( 'NONE',  ( 0.8182917201112819283, 0.000000000000000000, -0.03937007874015881204 ) ) ;
#38959 = CARTESIAN_POINT ( 'NONE',  ( -2.951990591674674480, 1.673246673531018525, -0.08331184815402598032 ) ) ;
#38960 = CARTESIAN_POINT ( 'NONE',  ( 0.000000000000000000, 3.267716535433071279, 0.7874015748031454320 ) ) ;
#38961 = LINE ( 'NONE', #39982, #13603 ) ;
#38962 = CARTESIAN_POINT ( 'NONE',  ( 0.4696143004045483793, 3.267716535433071279, -1.629301903132388985E-16 ) ) ;
#38963 = ADVANCED_FACE ( 'NONE', ( #42518 ), #3792, .F. ) ;
#38964 = CARTESIAN_POINT ( 'NONE',  ( 0.8182917201112824834, 0.000000000000000000, 2.047244094488179567 ) ) ;
#38965 = ADVANCED_FACE ( 'NONE', ( #30400 ), #42766, .F. ) ;
#38966 = CARTESIAN_POINT ( 'NONE',  ( -1.712496953225537411, 3.267716535433071279, 5.941417334598190051E-16 ) ) ;
#38967 = ORIENTED_EDGE ( 'NONE', *, *, #5039, .F. ) ;
#38968 = CARTESIAN_POINT ( 'NONE',  ( -0.8942052331142552601, 0.000000000000000000, -0.9448818897637760728 ) ) ;
#38969 = ORIENTED_EDGE ( 'NONE', *, *, #39061, .T. ) ;
#38970 = ORIENTED_EDGE ( 'NONE', *, *, #17816, .T. ) ;
#38971 = DIRECTION ( 'NONE',  ( -0.000000000000000000, 1.000000000000000000, -0.000000000000000000 ) ) ;
#38972 = CARTESIAN_POINT ( 'NONE',  ( -1.166969139818015755, 0.000000000000000000, 0.2755905511810996522 ) ) ;
#38973 = ORIENTED_EDGE ( 'NONE', *, *, #9642, .F. ) ;
#38974 = VECTOR ( 'NONE', #12718, 39.37007874015748143 ) ;
#38975 = LINE ( 'NONE', #35107, #4012 ) ;
#38976 = ORIENTED_EDGE ( 'NONE', *, *, #34131, .T. ) ;
#38977 = CARTESIAN_POINT ( 'NONE',  ( -2.919426793319806368, 1.673754417692067564, 0.4451252810446391095 ) ) ;
#38978 = VECTOR ( 'NONE', #335, 39.37007874015748143 ) ;
#38979 = ORIENTED_EDGE ( 'NONE', *, *, #45239, .T. ) ;
#38980 = VECTOR ( 'NONE', #1110, 39.37007874015748143 ) ;
#38981 = VECTOR ( 'NONE', #33018, 39.37007874015748854 ) ;
#38982 = FACE_OUTER_BOUND ( 'NONE', #4686, .T. ) ;
#38983 = CYLINDRICAL_SURFACE ( 'NONE', #44545, 2.164630168518208109 ) ;
#38984 = EDGE_CURVE ( 'NONE', #35848, #2274, #38900, .T. ) ;
#38985 = ORIENTED_EDGE ( 'NONE', *, *, #33529, .F. ) ;
#38986 = AXIS2_PLACEMENT_3D ( 'NONE', #39151, #31155, #15154 ) ;
#38987 = DIRECTION ( 'NONE',  ( -0.9362348706397418674, -1.160734090543305153E-16, 0.3513748240813305279 ) ) ;
#38988 = EDGE_LOOP ( 'NONE', ( #27602, #31894, #34156, #998 ) ) ;
#38989 = EDGE_LOOP ( 'NONE', ( #31645, #41722, #11109, #7852 ) ) ;
#38990 = PLANE ( 'NONE',  #31761 ) ;
#38991 = CARTESIAN_POINT ( 'NONE',  ( -0.2727639067037607723, 3.346456692913386100, -1.732283464566922726 ) ) ;
#38992 = LINE ( 'NONE', #27363, #23532 ) ;
#38993 = ADVANCED_FACE ( 'NONE', ( #30907 ), #31410, .F. ) ;
#38994 = ORIENTED_EDGE ( 'NONE', *, *, #19717, .T. ) ;
#38995 = ADVANCED_FACE ( 'NONE', ( #46366 ), #26514, .F. ) ;
#38996 = CARTESIAN_POINT ( 'NONE',  ( -0.5662636741187642153, 0.000000000000000000, 1.648861433446455971 ) ) ;
#38997 = DIRECTION ( 'NONE',  ( -0.000000000000000000, 1.000000000000000000, -0.000000000000000000 ) ) ;
#38998 = EDGE_CURVE ( 'NONE', #49634, #40865, #14905, .T. ) ;
#38999 = VERTEX_POINT ( 'NONE', #50711 ) ;
#39000 = DIRECTION ( 'NONE',  ( 1.734723475976806848E-16, -0.000000000000000000, 1.000000000000000000 ) ) ;
#39001 = ADVANCED_FACE ( 'NONE', ( #10774 ), #26767, .F. ) ;
#39002 = VERTEX_POINT ( 'NONE', #7658 ) ;
#39003 = VERTEX_POINT ( 'NONE', #15415 ) ;
#39004 = DIRECTION ( 'NONE',  ( 0.4737115861740300304, 0.8184814127304661513, -0.3250930791930596864 ) ) ;
#39006 = EDGE_CURVE ( 'NONE', #30636, #22491, #31158, .T. ) ;
#39005 = ORIENTED_EDGE ( 'NONE', *, *, #21663, .T. ) ;
#39007 = DIRECTION ( 'NONE',  ( -0.9998717552508122886, -0.01601477604151181275, 0.000000000000000000 ) ) ;
#39008 = FACE_OUTER_BOUND ( 'NONE', #28665, .T. ) ;
#39009 = DIRECTION ( 'NONE',  ( -1.000000000000000000, 0.000000000000000000, 1.734723475976806848E-16 ) ) ;
#39010 = CARTESIAN_POINT ( 'NONE',  ( -1.738955188402737440, 0.000000000000000000, -0.1273587697465547175 ) ) ;
#39011 = EDGE_LOOP ( 'NONE', ( #3930, #22046, #34282, #580, #7168, #29086, #10871, #25842, #20595, #35237, #15449, #17821, #36461 ) ) ;
#39012 = ORIENTED_EDGE ( 'NONE', *, *, #15816, .F. ) ;
#39013 = VECTOR ( 'NONE', #33570, 39.37007874015748143 ) ;
#39014 = CARTESIAN_POINT ( 'NONE',  ( -1.790900357307437352, 1.580792207208895128, -1.241130355818072406 ) ) ;
#39015 = FACE_OUTER_BOUND ( 'NONE', #30251, .T. ) ;
#39016 = VECTOR ( 'NONE', #48336, 39.37007874015748143 ) ;
#39017 = VERTEX_POINT ( 'NONE', #19020 ) ;
#39018 = DIRECTION ( 'NONE',  ( -0.000000000000000000, 0.000000000000000000, 1.000000000000000000 ) ) ;
#39019 = CARTESIAN_POINT ( 'NONE',  ( 1.091055626815043311, 0.000000000000000000, 1.692913385826762873 ) ) ;
#39020 = VECTOR ( 'NONE', #42123, 39.37007874015748854 ) ;
#39021 = EDGE_CURVE ( 'NONE', #14542, #13249, #50462, .T. ) ;
#39022 = AXIS2_PLACEMENT_3D ( 'NONE', #33899, #41892, #18397 ) ;
#39023 = ADVANCED_FACE ( 'NONE', ( #35287 ), #50968, .F. ) ;
#39024 = DIRECTION ( 'NONE',  ( 0.000000000000000000, 1.000000000000000000, 0.000000000000000000 ) ) ;
#39025 = DIRECTION ( 'NONE',  ( -0.000000000000000000, 1.000000000000000000, -0.000000000000000000 ) ) ;
#39026 = CARTESIAN_POINT ( 'NONE',  ( -1.062992125984250968, 0.000000000000000000, 1.181102362204724088 ) ) ;
#39027 = VECTOR ( 'NONE', #15842, 39.37007874015748143 ) ;
#39028 = VERTEX_POINT ( 'NONE', #28293 ) ;
#39029 = EDGE_CURVE ( 'NONE', #10448, #10406, #1193, .T. ) ;
#39030 = LINE ( 'NONE', #10901, #7704 ) ;
#39031 = CARTESIAN_POINT ( 'NONE',  ( 1.014069264286642014, 0.4235180831842794702, 1.062992125984251635 ) ) ;
#39032 = VERTEX_POINT ( 'NONE', #4813 ) ;
#39033 = PLANE ( 'NONE',  #996 ) ;
#39034 = DIRECTION ( 'NONE',  ( -3.469446951953613696E-16, 0.000000000000000000, -1.000000000000000000 ) ) ;
#39035 = CARTESIAN_POINT ( 'NONE',  ( 0.000000000000000000, 6.692913385826772199, 0.000000000000000000 ) ) ;
#39036 = ORIENTED_EDGE ( 'NONE', *, *, #43911, .F. ) ;
#39037 = ORIENTED_EDGE ( 'NONE', *, *, #9405, .F. ) ;
#39038 = DIRECTION ( 'NONE',  ( 0.000000000000000000, 1.160734090543304660E-16, -1.000000000000000000 ) ) ;
#39039 = ORIENTED_EDGE ( 'NONE', *, *, #15467, .F. ) ;
#39040 = CARTESIAN_POINT ( 'NONE',  ( 1.636583440222563857, 3.346456692913386100, -0.5118110236220471121 ) ) ;
#39041 = ORIENTED_EDGE ( 'NONE', *, *, #15350, .T. ) ;
#39042 = CARTESIAN_POINT ( 'NONE',  ( 0.8182917201112824834, 3.346456692913386100, 1.220472440944875281 ) ) ;
#39043 = FACE_OUTER_BOUND ( 'NONE', #23400, .T. ) ;
#39044 = DIRECTION ( 'NONE',  ( 0.000000000000000000, 1.000000000000000000, 0.000000000000000000 ) ) ;
#39045 = ORIENTED_EDGE ( 'NONE', *, *, #8838, .F. ) ;
#39046 = VECTOR ( 'NONE', #26942, 39.37007874015748143 ) ;
#39047 = ORIENTED_EDGE ( 'NONE', *, *, #18813, .F. ) ;
#39048 = VERTEX_POINT ( 'NONE', #48140 ) ;
#39049 = CARTESIAN_POINT ( 'NONE',  ( 0.000000000000000000, 6.692913385826772199, -2.086614173228346303 ) ) ;
#39050 = CARTESIAN_POINT ( 'NONE',  ( 1.636583440222563857, 3.346456692913386100, 1.062992125984245639 ) ) ;
#39051 = ORIENTED_EDGE ( 'NONE', *, *, #19669, .T. ) ;
#39052 = VERTEX_POINT ( 'NONE', #24178 ) ;
#39053 = VECTOR ( 'NONE', #41153, 39.37007874015748143 ) ;
#39054 = DIRECTION ( 'NONE',  ( -0.000000000000000000, 1.000000000000000000, -0.000000000000000000 ) ) ;
#39055 = DIRECTION ( 'NONE',  ( -1.000000000000000000, 0.000000000000000000, -0.000000000000000000 ) ) ;
#39056 = FACE_OUTER_BOUND ( 'NONE', #43033, .T. ) ;
#39057 = CIRCLE ( 'NONE', #30000, 2.106299212598425008 ) ;
#39058 = CIRCLE ( 'NONE', #20936, 2.106299212598425008 ) ;
#39059 = ORIENTED_EDGE ( 'NONE', *, *, #33232, .T. ) ;
#39060 = ORIENTED_EDGE ( 'NONE', *, *, #41891, .F. ) ;
#39061 = EDGE_CURVE ( 'NONE', #20081, #13474, #39409, .T. ) ;
#39062 = FACE_OUTER_BOUND ( 'NONE', #35707, .T. ) ;
#39063 = LINE ( 'NONE', #34444, #39825 ) ;
#39064 = LINE ( 'NONE', #50875, #3083 ) ;
#39065 = ADVANCED_FACE ( 'NONE', ( #15909 ), #44039, .F. ) ;
#39066 = ORIENTED_EDGE ( 'NONE', *, *, #22085, .F. ) ;
#39067 = CARTESIAN_POINT ( 'NONE',  ( 0.1067246931122726866, 0.02962905676920215767, 0.000000000000000000 ) ) ;
#39068 = EDGE_CURVE ( 'NONE', #29618, #22693, #12818, .T. ) ;
#39069 = CARTESIAN_POINT ( 'NONE',  ( -2.454875160333845674, 3.346456692913386100, -0.3543307086614173040 ) ) ;
#39070 = CONICAL_SURFACE ( 'NONE', #6089, 3.033577403570480779, 1.554780866114618743 ) ;
#39071 = ORIENTED_EDGE ( 'NONE', *, *, #22145, .T. ) ;
#39072 = FACE_OUTER_BOUND ( 'NONE', #38577, .T. ) ;
#39073 = VERTEX_POINT ( 'NONE', #40446 ) ;
#39074 = ORIENTED_EDGE ( 'NONE', *, *, #50978, .F. ) ;
#39075 = CARTESIAN_POINT ( 'NONE',  ( 0.5455278134075212115, 3.267716535433071279, -0.6299212598425181220 ) ) ;
#39076 = LINE ( 'NONE', #7083, #32479 ) ;
#39077 = CARTESIAN_POINT ( 'NONE',  ( -1.636583440222563635, 3.346456692913386100, 1.062992125984246083 ) ) ;
#39078 = CARTESIAN_POINT ( 'NONE',  ( -2.024313280741415255, 1.050020262844681751, -0.04164981208090088455 ) ) ;
#39079 = FACE_OUTER_BOUND ( 'NONE', #23483, .T. ) ;
#39080 = VERTEX_POINT ( 'NONE', #8681 ) ;
#39081 = VERTEX_POINT ( 'NONE', #12553 ) ;
#39082 = EDGE_CURVE ( 'NONE', #11815, #10495, #21277, .T. ) ;
#39083 = ORIENTED_EDGE ( 'NONE', *, *, #28070, .F. ) ;
#39084 = DIRECTION ( 'NONE',  ( -1.000000000000000000, 0.000000000000000000, 1.734723475976806848E-16 ) ) ;
#39085 = LINE ( 'NONE', #23332, #13568 ) ;
#39086 = EDGE_CURVE ( 'NONE', #29782, #2720, #36315, .T. ) ;
#39087 = ADVANCED_FACE ( 'NONE', ( #16691 ), #12303, .F. ) ;
#39088 = CARTESIAN_POINT ( 'NONE',  ( 1.015142113812069313, 0.000000000000000000, 0.7874015748031454320 ) ) ;
#39089 = CARTESIAN_POINT ( 'NONE',  ( 0.000000000000000000, 1.574803149606302854, 0.000000000000000000 ) ) ;
#39090 = ORIENTED_EDGE ( 'NONE', *, *, #41295, .T. ) ;
#39091 = VECTOR ( 'NONE', #9186, 39.37007874015748143 ) ;
#39092 = EDGE_CURVE ( 'NONE', #1553, #13738, #36566, .T. ) ;
#39093 = DIRECTION ( 'NONE',  ( 0.000000000000000000, 0.000000000000000000, 1.000000000000000000 ) ) ;
#39094 = EDGE_CURVE ( 'NONE', #30018, #50731, #35541, .T. ) ;
#39095 = CIRCLE ( 'NONE', #16846, 2.165354330708661568 ) ;
#39096 = CARTESIAN_POINT ( 'NONE',  ( -1.166969139818015977, 3.267716535433071279, 4.048737525165546155E-16 ) ) ;
#39097 = AXIS2_PLACEMENT_3D ( 'NONE', #32650, #13273, #5521 ) ;
#39098 = VECTOR ( 'NONE', #2846, 39.37007874015748143 ) ;
#39099 = ORIENTED_EDGE ( 'NONE', *, *, #21913, .F. ) ;
#39100 = CARTESIAN_POINT ( 'NONE',  ( 0.000000000000000000, 3.267716535433071279, 1.102362204724403938 ) ) ;
#39101 = CARTESIAN_POINT ( 'NONE',  ( -0.8182917201112819283, 0.000000000000000000, -1.732283464566922726 ) ) ;
#39102 = DIRECTION ( 'NONE',  ( 1.000000000000000000, -0.000000000000000000, 0.000000000000000000 ) ) ;
#39103 = FACE_OUTER_BOUND ( 'NONE', #15171, .T. ) ;
#39104 = CARTESIAN_POINT ( 'NONE',  ( -2.889674983507169337, 1.205361022782829114E-17, -0.6090712660038032356 ) ) ;
#39105 = LINE ( 'NONE', #27470, #26712 ) ;
#39106 = VECTOR ( 'NONE', #23467, 39.37007874015748143 ) ;
#39107 = ORIENTED_EDGE ( 'NONE', *, *, #31488, .F. ) ;
#39108 = CARTESIAN_POINT ( 'NONE',  ( 0.07982360342473591996, 1.709180471932028711, 0.000000000000000000 ) ) ;
#39109 = ORIENTED_EDGE ( 'NONE', *, *, #4694, .T. ) ;
#39110 = CARTESIAN_POINT ( 'NONE',  ( 2.106197740627112402, 3.346456692913386100, 0.02067487291359298290 ) ) ;
#39111 = FACE_OUTER_BOUND ( 'NONE', #30382, .T. ) ;
#39112 = LINE ( 'NONE', #3743, #44946 ) ;
#39113 = ORIENTED_EDGE ( 'NONE', *, *, #11989, .T. ) ;
#39114 = ORIENTED_EDGE ( 'NONE', *, *, #10361, .F. ) ;
#39115 = CARTESIAN_POINT ( 'NONE',  ( -1.030301126714985971, 0.000000000000000000, -1.501813316714599500 ) ) ;
#39116 = CARTESIAN_POINT ( 'NONE',  ( 0.2727639067037602172, 3.346456692913386100, -1.929133858267710000 ) ) ;
#39117 = ORIENTED_EDGE ( 'NONE', *, *, #50439, .F. ) ;
#39118 = LINE ( 'NONE', #46334, #2765 ) ;
#39119 = DIRECTION ( 'NONE',  ( -0.01601477604151182663, 0.9998717552508123996, -0.000000000000000000 ) ) ;
#39120 = DIRECTION ( 'NONE',  ( 0.9510565162951545304, 0.000000000000000000, -0.3090169943749447867 ) ) ;
#39121 = DIRECTION ( 'NONE',  ( 1.000000000000000000, 0.000000000000000000, 0.000000000000000000 ) ) ;
#39122 = VERTEX_POINT ( 'NONE', #31669 ) ;
#39123 = LINE ( 'NONE', #38630, #28732 ) ;
#39124 = LINE ( 'NONE', #6876, #12563 ) ;
#39125 = LINE ( 'NONE', #3764, #19072 ) ;
#39126 = EDGE_CURVE ( 'NONE', #50130, #29859, #49544, .T. ) ;
#39127 = APPLICATION_CONTEXT ( 'automotive_design' ) ;
#39128 = VECTOR ( 'NONE', #46055, 39.37007874015748143 ) ;
#39129 = VERTEX_POINT ( 'NONE', #28039 ) ;
#39130 = EDGE_CURVE ( 'NONE', #1872, #47459, #8937, .T. ) ;
#39131 = LINE ( 'NONE', #4025, #10903 ) ;
#39132 = VECTOR ( 'NONE', #13199, 39.37007874015748143 ) ;
#39133 = ORIENTED_EDGE ( 'NONE', *, *, #47084, .T. ) ;
#39134 = ORIENTED_EDGE ( 'NONE', *, *, #36311, .T. ) ;
#39135 = DIRECTION ( 'NONE',  ( 0.3090169943749582204, 1.288287287306305283E-16, -0.9510565162951500895 ) ) ;
#39136 = EDGE_CURVE ( 'NONE', #6492, #34811, #29218, .T. ) ;
#39137 = VECTOR ( 'NONE', #24765, 39.37007874015748143 ) ;
#39138 = ORIENTED_EDGE ( 'NONE', *, *, #48765, .T. ) ;
#39139 = ORIENTED_EDGE ( 'NONE', *, *, #17978, .T. ) ;
#39140 = FACE_OUTER_BOUND ( 'NONE', #10191, .T. ) ;
#39141 = EDGE_LOOP ( 'NONE', ( #44903, #35136, #1613, #49242 ) ) ;
#39142 = AXIS2_PLACEMENT_3D ( 'NONE', #12061, #7677, #34798 ) ;
#39143 = DIRECTION ( 'NONE',  ( 0.000000000000000000, 0.000000000000000000, 1.000000000000000000 ) ) ;
#39144 = LINE ( 'NONE', #30641, #17031 ) ;
#39145 = CARTESIAN_POINT ( 'NONE',  ( -2.932638728931780125, 1.673548413681422042, 0.3475908556737793420 ) ) ;
#39146 = EDGE_CURVE ( 'NONE', #35538, #4542, #23659, .T. ) ;
#39147 = CARTESIAN_POINT ( 'NONE',  ( 0.5455278134075208785, 0.000000000000000000, -1.574803149606293529 ) ) ;
#39148 = LINE ( 'NONE', #6896, #26956 ) ;
#39149 = FACE_OUTER_BOUND ( 'NONE', #26937, .T. ) ;
#39150 = ORIENTED_EDGE ( 'NONE', *, *, #25225, .T. ) ;
#39151 = CARTESIAN_POINT ( 'NONE',  ( 1.363819533518803251, 0.000000000000000000, 0.5905511811023579360 ) ) ;
#39152 = EDGE_CURVE ( 'NONE', #37360, #28099, #4296, .T. ) ;
#39153 = DIRECTION ( 'NONE',  ( 1.000000000000000000, -0.000000000000000000, 0.000000000000000000 ) ) ;
#39154 = CARTESIAN_POINT ( 'NONE',  ( 2.755905511811024056, 2.913385826771657250, 1.023622047244094446 ) ) ;
#39155 = ORIENTED_EDGE ( 'NONE', *, *, #1075, .T. ) ;
#39156 = DIRECTION ( 'NONE',  ( 0.000000000000000000, -1.000000000000000000, 0.000000000000000000 ) ) ;
#39157 = CARTESIAN_POINT ( 'NONE',  ( -0.6214413264104939882, 3.267716535433071279, 0.7874015748031456541 ) ) ;
#39158 = ORIENTED_EDGE ( 'NONE', *, *, #18280, .T. ) ;
#39159 = DIRECTION ( 'NONE',  ( 0.000000000000000000, 1.000000000000000000, 0.000000000000000000 ) ) ;
#39160 = FACE_OUTER_BOUND ( 'NONE', #3793, .T. ) ;
#39161 = VECTOR ( 'NONE', #34651, 39.37007874015748143 ) ;
#39162 = VECTOR ( 'NONE', #32456, 39.37007874015748143 ) ;
#39163 = AXIS2_PLACEMENT_3D ( 'NONE', #23213, #35356, #30718 ) ;
#39164 = LINE ( 'NONE', #2789, #41393 ) ;
#39165 = VERTEX_POINT ( 'NONE', #420 ) ;
#39166 = CARTESIAN_POINT ( 'NONE',  ( 2.110884035022549732, 1.741711621820001943, -0.9557545615714394538 ) ) ;
#39167 = AXIS2_PLACEMENT_3D ( 'NONE', #24126, #4507, #28500 ) ;
#39168 = FACE_OUTER_BOUND ( 'NONE', #50438, .T. ) ;
#39169 = CARTESIAN_POINT ( 'NONE',  ( 0.000000000000000000, 3.346456692913386100, 0.000000000000000000 ) ) ;
#39170 = CARTESIAN_POINT ( 'NONE',  ( 2.623503965249849301, 1.661669217907264740, 1.355882097269874187 ) ) ;
#39171 = VERTEX_POINT ( 'NONE', #43776 ) ;
#39172 = AXIS2_PLACEMENT_3D ( 'NONE', #10161, #22045, #33926 ) ;
#39173 = VERTEX_POINT ( 'NONE', #8429 ) ;
#39174 = ORIENTED_EDGE ( 'NONE', *, *, #43604, .T. ) ;
#39175 = DIRECTION ( 'NONE',  ( 1.000000000000000000, -0.000000000000000000, 0.000000000000000000 ) ) ;
#39176 = ORIENTED_EDGE ( 'NONE', *, *, #48007, .T. ) ;
#39177 = CARTESIAN_POINT ( 'NONE',  ( -0.9914495361339012991, 1.703811331058339373, 2.781765111341808705 ) ) ;
#39178 = PLANE ( 'NONE',  #7122 ) ;
#39179 = ORIENTED_EDGE ( 'NONE', *, *, #17622, .F. ) ;
#39180 = CARTESIAN_POINT ( 'NONE',  ( -2.009899395340762229, 3.346456692913386100, -0.6299212598425177889 ) ) ;
#39181 = ORIENTED_EDGE ( 'NONE', *, *, #9405, .T. ) ;
#39182 = DIRECTION ( 'NONE',  ( 1.000000000000000000, -0.000000000000000000, 0.000000000000000000 ) ) ;
#39183 = ADVANCED_FACE ( 'NONE', ( #39923 ), #4556, .F. ) ;
#39184 = ORIENTED_EDGE ( 'NONE', *, *, #24809, .T. ) ;
#39186 = EDGE_LOOP ( 'NONE', ( #46884, #1780, #35596, #30320, #5251, #34222, #50355, #11507, #11596, #3512, #6316 ) ) ;
#39185 = EDGE_CURVE ( 'NONE', #41776, #50744, #6079, .T. ) ;
#39187 = CARTESIAN_POINT ( 'NONE',  ( 0.9218113296639885990, 0.000000000000000000, -1.800737481590852118 ) ) ;
#39188 = VERTEX_POINT ( 'NONE', #1446 ) ;
#39189 = EDGE_CURVE ( 'NONE', #1162, #13413, #32710, .T. ) ;
#39190 = CARTESIAN_POINT ( 'NONE',  ( 3.335048530465896514E-16, 3.346456692913386100, 2.493791675044291445 ) ) ;
#39192 = ORIENTED_EDGE ( 'NONE', *, *, #23578, .F. ) ;
#39191 = ADVANCED_FACE ( 'NONE', ( #29057 ), #5079, .T. ) ;
#39193 = ORIENTED_EDGE ( 'NONE', *, *, #43069, .F. ) ;
#39194 = LINE ( 'NONE', #46905, #43787 ) ;
#39195 = AXIS2_PLACEMENT_3D ( 'NONE', #156, #15907, #7412 ) ;
#39196 = DIRECTION ( 'NONE',  ( 0.000000000000000000, -1.000000000000000000, 0.000000000000000000 ) ) ;
#39197 = AXIS2_PLACEMENT_3D ( 'NONE', #34731, #23101, #38855 ) ;
#39198 = EDGE_LOOP ( 'NONE', ( #25032, #25403, #28953, #46707 ) ) ;
#39199 = DIRECTION ( 'NONE',  ( -0.7071067811865466846, 0.000000000000000000, 0.7071067811865483499 ) ) ;
#39200 = CONICAL_SURFACE ( 'NONE', #27652, 1.850107469027523210, 0.6386652850508578450 ) ;
#39201 = ORIENTED_EDGE ( 'NONE', *, *, #2908, .T. ) ;
#39202 = FACE_OUTER_BOUND ( 'NONE', #50200, .T. ) ;
#39203 = CARTESIAN_POINT ( 'NONE',  ( 0.000000000000000000, 0.000000000000000000, 0.000000000000000000 ) ) ;
#39204 = EDGE_CURVE ( 'NONE', #24648, #4720, #29320, .T. ) ;
#39205 = AXIS2_PLACEMENT_3D ( 'NONE', #42853, #3884, #11874 ) ;
#39206 = CARTESIAN_POINT ( 'NONE',  ( -2.165668409223900692, 1.578950121022790531, 1.109510278747024348 ) ) ;
#39207 = ORIENTED_EDGE ( 'NONE', *, *, #38802, .T. ) ;
#39208 = EDGE_LOOP ( 'NONE', ( #5319, #21366, #49441, #28370 ) ) ;
#39209 = VECTOR ( 'NONE', #50361, 39.37007874015748143 ) ;
#39210 = CARTESIAN_POINT ( 'NONE',  ( -0.3486774197067340486, 3.267716535433071279, -1.456692913385822630 ) ) ;
#39211 = FACE_OUTER_BOUND ( 'NONE', #38304, .T. ) ;
#39212 = CARTESIAN_POINT ( 'NONE',  ( 1.441853549388196321, 3.346456692913386100, 1.535433070866133898 ) ) ;
#39213 = EDGE_CURVE ( 'NONE', #31389, #24633, #9453, .T. ) ;
#39214 = CARTESIAN_POINT ( 'NONE',  ( 1.485598995959308333, -1.845608808797952187E-16, 1.625606721701626345 ) ) ;
#39215 = CARTESIAN_POINT ( 'NONE',  ( 0.08139965876239094178, 1.610780518492231694, 0.000000000000000000 ) ) ;
#39216 = LINE ( 'NONE', #6972, #10320 ) ;
#39217 = VERTEX_POINT ( 'NONE', #5830 ) ;
#39218 = LINE ( 'NONE', #31736, #15186 ) ;
#39219 = ORIENTED_EDGE ( 'NONE', *, *, #5649, .T. ) ;
#39220 = DIRECTION ( 'NONE',  ( 1.734723475976806848E-16, 0.000000000000000000, 1.000000000000000000 ) ) ;
#39221 = ORIENTED_EDGE ( 'NONE', *, *, #31887, .F. ) ;
#39222 = EDGE_CURVE ( 'NONE', #50189, #7253, #13834, .T. ) ;
#39223 = DIRECTION ( 'NONE',  ( -1.000000000000000000, 0.000000000000000000, -0.000000000000000000 ) ) ;
#39224 = CARTESIAN_POINT ( 'NONE',  ( -0.8182917201112819283, 3.346456692913386100, 2.047244094488179567 ) ) ;
#39225 = EDGE_LOOP ( 'NONE', ( #21125, #23877, #14247, #18440, #6675 ) ) ;
#39226 = B_SPLINE_CURVE_WITH_KNOTS ( 'NONE', 3,
 ( #26008, #5877, #29113, #29885 ),
 .UNSPECIFIED., .F., .F.,
 ( 4, 4 ),
 ( 2.220043001603228065E-07, 0.002500468287160468196 ),
 .UNSPECIFIED. ) ;
#39227 = AXIS2_PLACEMENT_3D ( 'NONE', #24817, #29454, #41083 ) ;
#39228 = LINE ( 'NONE', #35872, #23788 ) ;
#39229 = VECTOR ( 'NONE', #46912, 39.37007874015748143 ) ;
#39230 = ORIENTED_EDGE ( 'NONE', *, *, #21845, .F. ) ;
#39231 = PLANE ( 'NONE',  #28733 ) ;
#39232 = VECTOR ( 'NONE', #12265, 39.37007874015748143 ) ;
#39233 = ORIENTED_EDGE ( 'NONE', *, *, #39839, .T. ) ;
#39234 = LINE ( 'NONE', #27603, #19441 ) ;
#39235 = CARTESIAN_POINT ( 'NONE',  ( 0.002207914879453961969, 6.692913385826772199, 0.04916304461325451958 ) ) ;
#39236 = VECTOR ( 'NONE', #47790, 39.37007874015748143 ) ;
#39237 = VERTEX_POINT ( 'NONE', #17959 ) ;
#39238 = AXIS2_PLACEMENT_3D ( 'NONE', #3503, #31380, #47074 ) ;
#39239 = DIRECTION ( 'NONE',  ( 1.000000000000000000, -0.000000000000000000, 0.000000000000000000 ) ) ;
#39240 = ORIENTED_EDGE ( 'NONE', *, *, #25009, .F. ) ;
#39241 = ORIENTED_EDGE ( 'NONE', *, *, #28047, .F. ) ;
#39242 = LINE ( 'NONE', #31255, #37568 ) ;
#39243 = DIRECTION ( 'NONE',  ( -0.9810236935216818388, 0.000000000000000000, 0.1938878870612536220 ) ) ;
#39244 = PLANE ( 'NONE',  #13682 ) ;
#39245 = EDGE_CURVE ( 'NONE', #8994, #16391, #44798, .T. ) ;
#39246 = EDGE_LOOP ( 'NONE', ( #27358, #37479, #18512, #15520 ) ) ;
#39247 = FACE_OUTER_BOUND ( 'NONE', #26346, .T. ) ;
#39248 = CARTESIAN_POINT ( 'NONE',  ( -2.952069331832154919, 5.118110236220475784, 1.181102362204724310 ) ) ;
#39249 = EDGE_CURVE ( 'NONE', #28752, #28376, #36404, .T. ) ;
#39250 = EDGE_CURVE ( 'NONE', #7930, #49632, #2473, .T. ) ;
#39251 = ORIENTED_EDGE ( 'NONE', *, *, #23139, .T. ) ;
#39252 = CARTESIAN_POINT ( 'NONE',  ( -0.07591351300297366489, 3.346456692913386100, -2.244094488188968395 ) ) ;
#39253 = ORIENTED_EDGE ( 'NONE', *, *, #32920, .T. ) ;
#39254 = ORIENTED_EDGE ( 'NONE', *, *, #39477, .F. ) ;
#39255 = SHAPE_DEFINITION_REPRESENTATION ( #42939, #8330 ) ;
#39256 = VERTEX_POINT ( 'NONE', #45051 ) ;
#39257 = CARTESIAN_POINT ( 'NONE',  ( 0.5455278134075217666, 3.346456692913386100, 1.574803149606291974 ) ) ;
#39258 = DIRECTION ( 'NONE',  ( 1.000000000000000000, -0.000000000000000000, 0.000000000000000000 ) ) ;
#39260 = DIRECTION ( 'NONE',  ( 1.734723475976806848E-16, 0.000000000000000000, 1.000000000000000000 ) ) ;
#39259 = AXIS2_PLACEMENT_3D ( 'NONE', #30273, #26888, #38530 ) ;
#39261 = CARTESIAN_POINT ( 'NONE',  ( -1.091055626815042201, 3.267716535433071279, 1.892679809432643650E-16 ) ) ;
#39262 = ORIENTED_EDGE ( 'NONE', *, *, #47556, .F. ) ;
#39263 = ORIENTED_EDGE ( 'NONE', *, *, #23584, .T. ) ;
#39264 = AXIS2_PLACEMENT_3D ( 'NONE', #20942, #21456, #25072 ) ;
#39265 = FACE_OUTER_BOUND ( 'NONE', #50538, .T. ) ;
#39266 = VECTOR ( 'NONE', #8987, 39.37007874015748143 ) ;
#39267 = CARTESIAN_POINT ( 'NONE',  ( -2.951990591674674480, 1.673246673531018525, -0.08331184815402598032 ) ) ;
#39268 = ORIENTED_EDGE ( 'NONE', *, *, #8882, .F. ) ;
#39269 = CARTESIAN_POINT ( 'NONE',  ( 2.889674983507178219, 1.665813060096536402, -0.6090712660037608250 ) ) ;
#39270 = PLANE ( 'NONE',  #23485 ) ;
#39271 = AXIS2_PLACEMENT_3D ( 'NONE', #27426, #15567, #26924 ) ;
#39272 = CARTESIAN_POINT ( 'NONE',  ( -1.528548437492483814, 1.596993453424210063, 2.526376101412316721 ) ) ;
#39273 = VECTOR ( 'NONE', #30326, 39.37007874015748143 ) ;
#39274 = ADVANCED_FACE ( 'NONE', ( #48388 ), #41708, .F. ) ;
#39275 = LINE ( 'NONE', #39529, #18434 ) ;
#39276 = CARTESIAN_POINT ( 'NONE',  ( 1.357666866036842945, 1.736795568944660362, 2.368301409647881162 ) ) ;
#39277 = CARTESIAN_POINT ( 'NONE',  ( -1.909347346926324906, 0.000000000000000000, -0.6692913385826758654 ) ) ;
#39278 = VECTOR ( 'NONE', #36467, 39.37007874015748854 ) ;
#39279 = ORIENTED_EDGE ( 'NONE', *, *, #35642, .F. ) ;
#39280 = CARTESIAN_POINT ( 'NONE',  ( 0.1067246931122726866, 0.02962905676920215767, 0.000000000000000000 ) ) ;
#39281 = LINE ( 'NONE', #16562, #41718 ) ;
#39282 = ORIENTED_EDGE ( 'NONE', *, *, #43620, .F. ) ;
#39283 = EDGE_CURVE ( 'NONE', #38635, #43930, #44546, .T. ) ;
#39284 = ORIENTED_EDGE ( 'NONE', *, *, #36399, .T. ) ;
#39285 = DIRECTION ( 'NONE',  ( -3.469446951953613696E-16, 0.000000000000000000, -1.000000000000000000 ) ) ;
#39286 = DIRECTION ( 'NONE',  ( -0.3513748240813305279, 0.000000000000000000, -0.9362348706397418674 ) ) ;
#39287 = CARTESIAN_POINT ( 'NONE',  ( 1.528548638510035307, 1.743074481295564082, 2.526375981309921581 ) ) ;
#39288 = VERTEX_POINT ( 'NONE', #5318 ) ;
#39289 = B_SPLINE_CURVE_WITH_KNOTS ( 'NONE', 3,
 ( #15802, #3687, #33049, #48729 ),
 .UNSPECIFIED., .F., .F.,
 ( 4, 4 ),
 ( 0.0001991432653589252772, 0.002699267682809819522 ),
 .UNSPECIFIED. ) ;
#39290 = ADVANCED_FACE ( 'NONE', ( #14085 ), #1956, .F. ) ;
#39291 = VERTEX_POINT ( 'NONE', #17449 ) ;
#39292 = PLANE ( 'NONE',  #49298 ) ;
#39293 = ORIENTED_EDGE ( 'NONE', *, *, #9728, .T. ) ;
#39294 = DIRECTION ( 'NONE',  ( 8.741157232058247392E-17, -1.000000000000000000, -7.636919086868415696E-17 ) ) ;
#39295 = ORIENTED_EDGE ( 'NONE', *, *, #25228, .T. ) ;
#39296 = EDGE_CURVE ( 'NONE', #11113, #20686, #21071, .T. ) ;
#39297 = LINE ( 'NONE', #4184, #20219 ) ;
#39298 = CARTESIAN_POINT ( 'NONE',  ( 0.000000000000000000, 3.346456692913386100, 0.000000000000000000 ) ) ;
#39299 = PLANE ( 'NONE',  #31811 ) ;
#39300 = VECTOR ( 'NONE', #1449, 39.37007874015748143 ) ;
#39301 = VERTEX_POINT ( 'NONE', #13327 ) ;
#39302 = ORIENTED_EDGE ( 'NONE', *, *, #39340, .T. ) ;
#39303 = ORIENTED_EDGE ( 'NONE', *, *, #31984, .F. ) ;
#39304 = CARTESIAN_POINT ( 'NONE',  ( -0.2727639067037602727, 0.000000000000000000, 0.5905511811023582691 ) ) ;
#39305 = AXIS2_PLACEMENT_3D ( 'NONE', #49209, #13632, #18011 ) ;
#39306 = DIRECTION ( 'NONE',  ( -0.000000000000000000, -1.000000000000000000, -0.000000000000000000 ) ) ;
#39307 = ORIENTED_EDGE ( 'NONE', *, *, #18648, .T. ) ;
#39308 = ORIENTED_EDGE ( 'NONE', *, *, #37965, .F. ) ;
#39309 = PLANE ( 'NONE',  #38801 ) ;
#39310 = CARTESIAN_POINT ( 'NONE',  ( 1.015142113812069313, 0.000000000000000000, -0.1574803149606301411 ) ) ;
#39311 = DIRECTION ( 'NONE',  ( -1.000000000000000000, 0.000000000000000000, 1.734723475976806848E-16 ) ) ;
#39312 = EDGE_CURVE ( 'NONE', #7739, #43163, #21329, .T. ) ;
#39313 = ORIENTED_EDGE ( 'NONE', *, *, #21062, .T. ) ;
#39314 = CARTESIAN_POINT ( 'NONE',  ( 2.919426793319799707, 2.755905511811027164, 0.4451252810446823527 ) ) ;
#39315 = LINE ( 'NONE', #31835, #30766 ) ;
#39316 = AXIS2_PLACEMENT_3D ( 'NONE', #24607, #40610, #49066 ) ;
#39317 = DIRECTION ( 'NONE',  ( -0.000000000000000000, 1.000000000000000000, -0.000000000000000000 ) ) ;
#39318 = EDGE_CURVE ( 'NONE', #35864, #12600, #25702, .T. ) ;
#39319 = EDGE_CURVE ( 'NONE', #17488, #22117, #20735, .T. ) ;
#39320 = EDGE_LOOP ( 'NONE', ( #36289, #18963, #49668, #3753 ) ) ;
#39321 = DIRECTION ( 'NONE',  ( -0.9998717552508121775, -0.01601477604151182316, 0.000000000000000000 ) ) ;
#39322 = DIRECTION ( 'NONE',  ( 0.000000000000000000, 0.000000000000000000, -1.000000000000000000 ) ) ;
#39323 = ORIENTED_EDGE ( 'NONE', *, *, #37368, .F. ) ;
#39324 = EDGE_CURVE ( 'NONE', #1994, #1350, #25444, .T. ) ;
#39325 = CARTESIAN_POINT ( 'NONE',  ( -1.363819533518803473, 3.346456692913386100, 1.605145679676863057 ) ) ;
#39326 = ORIENTED_EDGE ( 'NONE', *, *, #44447, .T. ) ;
#39327 = ORIENTED_EDGE ( 'NONE', *, *, #29572, .F. ) ;
#39328 = DIRECTION ( 'NONE',  ( -0.000000000000000000, 1.000000000000000000, -0.000000000000000000 ) ) ;
#39329 = DIRECTION ( 'NONE',  ( -0.4338837391175526803, 0.000000000000000000, -0.9009688679024218105 ) ) ;
#39330 = DIRECTION ( 'NONE',  ( 0.000000000000000000, -1.000000000000000000, 0.000000000000000000 ) ) ;
#39331 = CARTESIAN_POINT ( 'NONE',  ( 0.07982360342473591996, 1.709180471932028711, 0.000000000000000000 ) ) ;
#39332 = CARTESIAN_POINT ( 'NONE',  ( 0.5484938309455573702, 0.5249316497054296038, -1.802438616747610745 ) ) ;
#39333 = ORIENTED_EDGE ( 'NONE', *, *, #42965, .F. ) ;
#39334 = ORIENTED_EDGE ( 'NONE', *, *, #2724, .F. ) ;
#39335 = VERTEX_POINT ( 'NONE', #6602 ) ;
#39336 = CARTESIAN_POINT ( 'NONE',  ( 2.950518648759354434, 1.765226948982748123, -0.1160872037111668892 ) ) ;
#39337 = DIRECTION ( 'NONE',  ( 0.3513748240813434620, 0.000000000000000000, -0.9362348706397368714 ) ) ;
#39338 = AXIS2_PLACEMENT_3D ( 'NONE', #28621, #13394, #32779 ) ;
#39339 = AXIS2_PLACEMENT_3D ( 'NONE', #10472, #49161, #1705 ) ;
#39340 = EDGE_CURVE ( 'NONE', #42191, #44778, #2161, .T. ) ;
#39341 = FACE_OUTER_BOUND ( 'NONE', #50084, .T. ) ;
#39342 = FACE_OUTER_BOUND ( 'NONE', #45003, .T. ) ;
#39343 = CONICAL_SURFACE ( 'NONE', #17097, 2.244934639244524632, 1.554780866114618743 ) ;
#39344 = ORIENTED_EDGE ( 'NONE', *, *, #46406, .F. ) ;
#39345 = DIRECTION ( 'NONE',  ( 0.000000000000000000, -1.000000000000000000, 0.000000000000000000 ) ) ;
#39346 = DIRECTION ( 'NONE',  ( -3.469446951953613696E-16, 0.000000000000000000, -1.000000000000000000 ) ) ;
#39347 = EDGE_CURVE ( 'NONE', #44408, #28725, #10722, .T. ) ;
#39348 = VERTEX_POINT ( 'NONE', #50162 ) ;
#39349 = DIRECTION ( 'NONE',  ( 0.000000000000000000, -1.000000000000000000, 0.000000000000000000 ) ) ;
#39350 = ADVANCED_FACE ( 'NONE', ( #3478 ), #23338, .F. ) ;
#39351 = FACE_OUTER_BOUND ( 'NONE', #42665, .T. ) ;
#39352 = FACE_OUTER_BOUND ( 'NONE', #28168, .T. ) ;
#39354 = EDGE_CURVE ( 'NONE', #34110, #11339, #3218, .T. ) ;
#39353 = ORIENTED_EDGE ( 'NONE', *, *, #21433, .T. ) ;
#39355 = LINE ( 'NONE', #3735, #44073 ) ;
#39356 = CARTESIAN_POINT ( 'NONE',  ( -0.3486774197067338266, 3.267716535433071279, 1.209717811016578585E-16 ) ) ;
#39357 = DIRECTION ( 'NONE',  ( 0.000000000000000000, 0.000000000000000000, -1.000000000000000000 ) ) ;
#39358 = VERTEX_POINT ( 'NONE', #11479 ) ;
#39359 = LINE ( 'NONE', #8884, #20566 ) ;
#39360 = B_SPLINE_CURVE_WITH_KNOTS ( 'NONE', 3,
 ( #5036, #20782, #36541, #16918 ),
 .UNSPECIFIED., .F., .F.,
 ( 4, 4 ),
 ( 0.03514866506299903909, 0.03730642777952080519 ),
 .UNSPECIFIED. ) ;
#39361 = VERTEX_POINT ( 'NONE', #18966 ) ;
#39362 = VECTOR ( 'NONE', #47167, 39.37007874015748143 ) ;
#39363 = DIRECTION ( 'NONE',  ( -0.3513748240813434620, -1.086579671787963332E-16, 0.9362348706397368714 ) ) ;
#39364 = CARTESIAN_POINT ( 'NONE',  ( 1.015142113812069091, 3.226129038349118794, -2.244094488188969283 ) ) ;
#39365 = CARTESIAN_POINT ( 'NONE',  ( -2.182111253630085734, 0.000000000000000000, -0.9448818897637762948 ) ) ;
#39366 = EDGE_CURVE ( 'NONE', #15591, #50954, #34225, .T. ) ;
#39367 = EDGE_LOOP ( 'NONE', ( #3564, #1800, #20367, #21521 ) ) ;
#39368 = ORIENTED_EDGE ( 'NONE', *, *, #5595, .F. ) ;
#39369 = DIRECTION ( 'NONE',  ( -1.000000000000000000, 0.000000000000000000, -0.000000000000000000 ) ) ;
#39370 = LINE ( 'NONE', #4254, #18856 ) ;
#39371 = B_SPLINE_CURVE_WITH_KNOTS ( 'NONE', 3,
 ( #15217, #18085, #2841, #18595 ),
 .UNSPECIFIED., .F., .F.,
 ( 4, 4 ),
 ( 0.01297872134738276700, 0.03074049562890820986 ),
 .UNSPECIFIED. ) ;
#39372 = VERTEX_POINT ( 'NONE', #26459 ) ;
#39373 = LINE ( 'NONE', #47331, #20896 ) ;
#39374 = FACE_OUTER_BOUND ( 'NONE', #8938, .T. ) ;
#39375 = EDGE_CURVE ( 'NONE', #46139, #8923, #7602, .T. ) ;
#39376 = LINE ( 'NONE', #23885, #24446 ) ;
#39377 = EDGE_CURVE ( 'NONE', #22056, #48706, #50408, .T. ) ;
#39378 = PLANE ( 'NONE',  #20668 ) ;
#39379 = EDGE_LOOP ( 'NONE', ( #967, #33730, #33088, #30949 ) ) ;
#39380 = ORIENTED_EDGE ( 'NONE', *, *, #17841, .T. ) ;
#39381 = DIRECTION ( 'NONE',  ( -0.000000000000000000, 1.000000000000000000, -0.000000000000000000 ) ) ;
#39382 = AXIS2_PLACEMENT_3D ( 'NONE', #26657, #18417, #14035 ) ;
#39383 = CONICAL_SURFACE ( 'NONE', #17129, 3.483074324928249421, 1.244861948955335196 ) ;
#39384 = ADVANCED_FACE ( 'NONE', ( #49908 ), #14338, .F. ) ;
#39385 = EDGE_CURVE ( 'NONE', #21759, #17096, #27212, .T. ) ;
#39386 = DIRECTION ( 'NONE',  ( -3.469446951953613696E-16, 0.000000000000000000, -1.000000000000000000 ) ) ;
#39387 = ORIENTED_EDGE ( 'NONE', *, *, #27211, .T. ) ;
#39388 = EDGE_CURVE ( 'NONE', #22792, #26280, #18214, .T. ) ;
#39389 = DIRECTION ( 'NONE',  ( -3.469446951953613696E-16, 0.000000000000000000, -1.000000000000000000 ) ) ;
#39390 = ORIENTED_EDGE ( 'NONE', *, *, #21188, .F. ) ;
#39392 = ORIENTED_EDGE ( 'NONE', *, *, #10847, .F. ) ;
#39391 = AXIS2_PLACEMENT_3D ( 'NONE', #48234, #28646, #44393 ) ;
#39393 = CARTESIAN_POINT ( 'NONE',  ( -0.5354483489059734813, 0.01294997333450623005, -1.755169374176263730 ) ) ;
#39394 = ORIENTED_EDGE ( 'NONE', *, *, #23973, .T. ) ;
#39395 = ORIENTED_EDGE ( 'NONE', *, *, #15196, .T. ) ;
#39396 = LINE ( 'NONE', #20279, #44216 ) ;
#39397 = VECTOR ( 'NONE', #45909, 39.37007874015748143 ) ;
#39398 = ORIENTED_EDGE ( 'NONE', *, *, #19205, .F. ) ;
#39400 = CARTESIAN_POINT ( 'NONE',  ( 2.559055118110236560, 0.000000000000000000, -4.133858267716535195 ) ) ;
#39399 = CONICAL_SURFACE ( 'NONE', #35274, 2.165354330708661568, 0.2617993877991570129 ) ;
#39401 = FACE_OUTER_BOUND ( 'NONE', #42592, .T. ) ;
#39402 = CARTESIAN_POINT ( 'NONE',  ( 1.661821349926414282, 6.692913385826772199, 1.388203579611976712 ) ) ;
#39403 = CARTESIAN_POINT ( 'NONE',  ( 1.287906020515829919, 0.000000000000000000, -1.574803149606294417 ) ) ;
#39404 = LINE ( 'NONE', #4807, #5564 ) ;
#39405 = CARTESIAN_POINT ( 'NONE',  ( -2.061297163897529483, 3.346456692913386100, 0.4330708661417290162 ) ) ;
#39406 = ORIENTED_EDGE ( 'NONE', *, *, #9976, .T. ) ;
#39407 = DIRECTION ( 'NONE',  ( -3.469446951953613696E-16, 0.000000000000000000, -1.000000000000000000 ) ) ;
#39408 = CARTESIAN_POINT ( 'NONE',  ( 0.3664524127070866721, 2.755905511811024056, 0.07483588040983164824 ) ) ;
#39409 = LINE ( 'NONE', #20295, #27316 ) ;
#39410 = VERTEX_POINT ( 'NONE', #34721 ) ;
#39411 = CARTESIAN_POINT ( 'NONE',  ( 0.000000000000000000, 1.574803149606302854, -2.165354330708661568 ) ) ;
#39412 = ADVANCED_FACE ( 'NONE', ( #30597 ), #15097, .T. ) ;
#39413 = DIRECTION ( 'NONE',  ( -0.000000000000000000, 1.000000000000000000, -0.000000000000000000 ) ) ;
#39414 = ORIENTED_EDGE ( 'NONE', *, *, #6780, .T. ) ;
#39415 = DIRECTION ( 'NONE',  ( -0.000000000000000000, 1.000000000000000000, -0.000000000000000000 ) ) ;
#39416 = CIRCLE ( 'NONE', #46821, 0.3740157480314960647 ) ;
#39417 = CARTESIAN_POINT ( 'NONE',  ( 2.258212185701618857, 1.750938538929015076, -1.549600192960912004 ) ) ;
#39418 = EDGE_CURVE ( 'NONE', #39032, #28119, #22590, .T. ) ;
#39419 = DIRECTION ( 'NONE',  ( -0.7818314824680221431, 0.000000000000000000, -0.6234898018587431423 ) ) ;
#39420 = VECTOR ( 'NONE', #15078, 39.37007874015748143 ) ;
#39421 = DIRECTION ( 'NONE',  ( -0.000000000000000000, 0.000000000000000000, 1.000000000000000000 ) ) ;
#39422 = ORIENTED_EDGE ( 'NONE', *, *, #40814, .F. ) ;
#39423 = CARTESIAN_POINT ( 'NONE',  ( 2.105931235793975009, 3.267716535433071279, -0.03937007874015936021 ) ) ;
#39424 = CARTESIAN_POINT ( 'NONE',  ( 0.1067246931122726866, 0.02962905676920215767, 0.000000000000000000 ) ) ;
#39425 = AXIS2_PLACEMENT_3D ( 'NONE', #14281, #2419, #26164 ) ;
#39426 = CARTESIAN_POINT ( 'NONE',  ( -2.952069331832154919, 5.118110236220475784, 1.181102362204724310 ) ) ;
#39427 = CARTESIAN_POINT ( 'NONE',  ( -1.636583440222564301, 0.000000000000000000, -1.456692913385822186 ) ) ;
#39428 = ORIENTED_EDGE ( 'NONE', *, *, #26663, .F. ) ;
#39429 = VECTOR ( 'NONE', #13119, 39.37007874015748143 ) ;
#39430 = ORIENTED_EDGE ( 'NONE', *, *, #7322, .T. ) ;
#39431 = VERTEX_POINT ( 'NONE', #46807 ) ;
#39432 = DIRECTION ( 'NONE',  ( 1.000000000000000000, -0.000000000000000000, 0.000000000000000000 ) ) ;
#39433 = EDGE_LOOP ( 'NONE', ( #23894, #34950, #38432, #3685 ) ) ;
#39434 = CARTESIAN_POINT ( 'NONE',  ( 0.000000000000000000, 2.362204724409439294, 0.000000000000000000 ) ) ;
#39435 = EDGE_CURVE ( 'NONE', #8967, #9639, #26711, .T. ) ;
#39436 = AXIS2_PLACEMENT_3D ( 'NONE', #41016, #29124, #36628 ) ;
#39437 = CARTESIAN_POINT ( 'NONE',  ( 2.106197740627111514, 0.000000000000000000, -0.9842519685039348154 ) ) ;
#39438 = ORIENTED_EDGE ( 'NONE', *, *, #12415, .F. ) ;
#39439 = LINE ( 'NONE', #3818, #19009 ) ;
#39440 = ADVANCED_FACE ( 'NONE', ( #41963 ), #26213, .F. ) ;
#39441 = ORIENTED_EDGE ( 'NONE', *, *, #12904, .T. ) ;
#39442 = FACE_OUTER_BOUND ( 'NONE', #16402, .T. ) ;
#39443 = EDGE_CURVE ( 'NONE', #16050, #39976, #30090, .T. ) ;
#39444 = LINE ( 'NONE', #2871, #28093 ) ;
#39445 = ORIENTED_EDGE ( 'NONE', *, *, #1533, .T. ) ;
#39446 = EDGE_LOOP ( 'NONE', ( #15741, #27504, #47740, #11646 ) ) ;
#39447 = EDGE_CURVE ( 'NONE', #1681, #37048, #22344, .T. ) ;
#39448 = DIRECTION ( 'NONE',  ( -0.000000000000000000, 1.000000000000000000, -0.000000000000000000 ) ) ;
#39449 = EDGE_LOOP ( 'NONE', ( #28497, #19869, #291, #22210 ) ) ;
#39450 = CARTESIAN_POINT ( 'NONE',  ( 2.168245791271197209, 1.466194936398640181, -2.004968704497248400 ) ) ;
#39451 = ORIENTED_EDGE ( 'NONE', *, *, #2847, .T. ) ;
#39452 = ORIENTED_EDGE ( 'NONE', *, *, #48484, .T. ) ;
#39453 = CARTESIAN_POINT ( 'NONE',  ( 2.803166786255866239, 1.450263284045836709, 0.9280585611840251881 ) ) ;
#39454 = CARTESIAN_POINT ( 'NONE',  ( -0.2906532981117672110, 1.205361022782829114E-17, 1.877244666688175245 ) ) ;
#39455 = ORIENTED_EDGE ( 'NONE', *, *, #72, .F. ) ;
#39456 = AXIS2_PLACEMENT_3D ( 'NONE', #11609, #15731, #46937 ) ;
#39457 = DIRECTION ( 'NONE',  ( 1.734723475976806848E-16, -0.000000000000000000, 1.000000000000000000 ) ) ;
#39458 = VERTEX_POINT ( 'NONE', #27973 ) ;
#39459 = FACE_OUTER_BOUND ( 'NONE', #16324, .T. ) ;
#39460 = DIRECTION ( 'NONE',  ( -0.01601477604151182663, 0.9998717552508123996, -0.000000000000000000 ) ) ;
#39461 = VECTOR ( 'NONE', #28008, 39.37007874015748143 ) ;
#39462 = AXIS2_PLACEMENT_3D ( 'NONE', #10797, #49489, #13920 ) ;
#39463 = DIRECTION ( 'NONE',  ( -0.000000000000000000, 1.000000000000000000, -0.000000000000000000 ) ) ;
#39464 = CIRCLE ( 'NONE', #28783, 2.246510896728926010 ) ;
#39465 = ORIENTED_EDGE ( 'NONE', *, *, #42715, .T. ) ;
#39466 = ORIENTED_EDGE ( 'NONE', *, *, #12256, .T. ) ;
#39467 = CARTESIAN_POINT ( 'NONE',  ( 0.5433595661824232037, 1.502645338999371249, 2.902377712497140827 ) ) ;
#39468 = DIRECTION ( 'NONE',  ( 1.000000000000000000, 0.000000000000000000, 0.000000000000000000 ) ) ;
#39469 = B_SPLINE_CURVE_WITH_KNOTS ( 'NONE', 3,
 ( #32957, #13318, #29051, #21320 ),
 .UNSPECIFIED., .F., .F.,
 ( 4, 4 ),
 ( 6.049486680839438895E-07, 0.0005306152659298648405 ),
 .UNSPECIFIED. ) ;
#39470 = DIRECTION ( 'NONE',  ( 1.000000000000000000, 0.000000000000000000, 0.000000000000000000 ) ) ;
#39471 = AXIS2_PLACEMENT_3D ( 'NONE', #31940, #40452, #16956 ) ;
#39472 = DIRECTION ( 'NONE',  ( -0.9510565162951500895, 0.000000000000000000, -0.3090169943749582204 ) ) ;
#39473 = DIRECTION ( 'NONE',  ( -1.000000000000000000, 0.000000000000000000, 0.000000000000000000 ) ) ;
#39474 = DIRECTION ( 'NONE',  ( -3.986037398843765983E-20, -1.000000000000000000, -1.160734090543304660E-16 ) ) ;
#39475 = EDGE_LOOP ( 'NONE', ( #29899, #12951, #11442, #18503 ) ) ;
#39476 = DIRECTION ( 'NONE',  ( -3.469446951953613696E-16, 0.000000000000000000, -1.000000000000000000 ) ) ;
#39477 = EDGE_CURVE ( 'NONE', #15126, #3065, #35227, .T. ) ;
#39478 = EDGE_LOOP ( 'NONE', ( #14240, #12362, #43323, #28764 ) ) ;
#39479 = FACE_OUTER_BOUND ( 'NONE', #1065, .T. ) ;
#39480 = EDGE_CURVE ( 'NONE', #18622, #19884, #35477, .T. ) ;
#39481 = EDGE_LOOP ( 'NONE', ( #42947, #34755, #37522, #49123 ) ) ;
#39482 = EDGE_CURVE ( 'NONE', #4093, #39165, #8365, .T. ) ;
#39483 = CARTESIAN_POINT ( 'NONE',  ( -1.166969139818015755, 0.000000000000000000, 0.9055118110236167750 ) ) ;
#39484 = DIRECTION ( 'NONE',  ( 1.734723475976806848E-16, 0.000000000000000000, 1.000000000000000000 ) ) ;
#39485 = CONICAL_SURFACE ( 'NONE', #12296, 3.033577403570480779, 1.554780866114618743 ) ;
#39486 = ORIENTED_EDGE ( 'NONE', *, *, #25084, .T. ) ;
#39487 = LINE ( 'NONE', #15488, #14736 ) ;
#39488 = EDGE_LOOP ( 'NONE', ( #31453, #47150, #31560, #26922 ) ) ;
#39489 = DIRECTION ( 'NONE',  ( 0.000000000000000000, 1.000000000000000000, 0.000000000000000000 ) ) ;
#39490 = VERTEX_POINT ( 'NONE', #28225 ) ;
#39491 = AXIS2_PLACEMENT_3D ( 'NONE', #10374, #1858, #49055 ) ;
#39492 = VECTOR ( 'NONE', #3208, 39.37007874015748143 ) ;
#39493 = DIRECTION ( 'NONE',  ( 0.01601477604151182663, -0.9998717552508123996, 0.000000000000000000 ) ) ;
#39494 = CARTESIAN_POINT ( 'NONE',  ( -1.166969139818015977, 3.346456692913386100, 1.732283464566920950 ) ) ;
#39495 = EDGE_CURVE ( 'NONE', #14359, #24862, #39856, .T. ) ;
#39496 = VECTOR ( 'NONE', #19225, 39.37007874015748143 ) ;
#39497 = ORIENTED_EDGE ( 'NONE', *, *, #25629, .T. ) ;
#39498 = CARTESIAN_POINT ( 'NONE',  ( 0.04921259842519667277, 1.720031199985617265, 2.952755905511811108 ) ) ;
#39499 = ORIENTED_EDGE ( 'NONE', *, *, #25364, .T. ) ;
#39500 = VERTEX_POINT ( 'NONE', #12751 ) ;
#39501 = ADVANCED_FACE ( 'NONE', ( #36251 ), #43968, .F. ) ;
#39502 = CARTESIAN_POINT ( 'NONE',  ( 0.8182917201112817063, 0.000000000000000000, -2.244094488188969283 ) ) ;
#39503 = CARTESIAN_POINT ( 'NONE',  ( -1.843283979527560623, 1.678378384481335139, -1.157773721536293765 ) ) ;
#39504 = CARTESIAN_POINT ( 'NONE',  ( 0.000000000000000000, 0.000000000000000000, 0.000000000000000000 ) ) ;
#39505 = VECTOR ( 'NONE', #39102, 39.37007874015748143 ) ;
#39506 = ORIENTED_EDGE ( 'NONE', *, *, #39873, .T. ) ;
#39507 = CARTESIAN_POINT ( 'NONE',  ( 1.909347346926324684, 3.346456692913386100, 0.1574803149606280872 ) ) ;
#39508 = DIRECTION ( 'NONE',  ( 0.000000000000000000, 1.000000000000000000, 0.000000000000000000 ) ) ;
#39509 = EDGE_LOOP ( 'NONE', ( #34144, #32784, #42391, #38465 ) ) ;
#39510 = CARTESIAN_POINT ( 'NONE',  ( -0.5455278134075214336, 0.000000000000000000, 0.1181102362204703021 ) ) ;
#39511 = ORIENTED_EDGE ( 'NONE', *, *, #5843, .T. ) ;
#39512 = VERTEX_POINT ( 'NONE', #24109 ) ;
#39513 = PRODUCT_CONTEXT ( 'NONE', #2865, 'mechanical' ) ;
#39514 = B_SPLINE_CURVE_WITH_KNOTS ( 'NONE', 3,
 ( #35486, #4755, #32132, #4499 ),
 .UNSPECIFIED., .F., .F.,
 ( 4, 4 ),
 ( 0.0003353342934138906894, 0.04951278680019933348 ),
 .UNSPECIFIED. ) ;
#39515 = ADVANCED_FACE ( 'NONE', ( #24369 ), #40118, .F. ) ;
#39516 = ORIENTED_EDGE ( 'NONE', *, *, #16268, .T. ) ;
#39517 = CARTESIAN_POINT ( 'NONE',  ( 0.000000000000000000, 3.267716535433071279, 0.7480314960629874665 ) ) ;
#39518 = CARTESIAN_POINT ( 'NONE',  ( 1.883550378546972937, 5.905511811023623991, -1.069467267250421072 ) ) ;
#39519 = FACE_OUTER_BOUND ( 'NONE', #245, .T. ) ;
#39520 = CARTESIAN_POINT ( 'NONE',  ( -0.3486774197067340486, 0.000000000000000000, 0.1181102362204703021 ) ) ;
#39521 = VERTEX_POINT ( 'NONE', #7856 ) ;
#39522 = ORIENTED_EDGE ( 'NONE', *, *, #5994, .T. ) ;
#39523 = FILL_AREA_STYLE_COLOUR ( '', #12276 ) ;
#39524 = CARTESIAN_POINT ( 'NONE',  ( 0.07982360342473591996, 1.709180471932028711, 0.000000000000000000 ) ) ;
#39525 = ORIENTED_EDGE ( 'NONE', *, *, #50499, .T. ) ;
#39526 = CARTESIAN_POINT ( 'NONE',  ( 2.889674983507178219, 1.764288196056212454, -0.6090712660037608250 ) ) ;
#39527 = CARTESIAN_POINT ( 'NONE',  ( 0.7423782071083092626, 0.000000000000000000, 1.889763779527550369 ) ) ;
#39528 = VECTOR ( 'NONE', #21185, 39.37007874015748143 ) ;
#39529 = CARTESIAN_POINT ( 'NONE',  ( -0.07591351300297277671, 3.346456692913386100, 1.732283464566921172 ) ) ;
#39530 = CARTESIAN_POINT ( 'NONE',  ( 2.755905511811024056, 2.913385826771657250, 1.023622047244094446 ) ) ;
#39531 = DIRECTION ( 'NONE',  ( -0.000000000000000000, -0.000000000000000000, 1.000000000000000000 ) ) ;
#39532 = ORIENTED_EDGE ( 'NONE', *, *, #43031, .T. ) ;
#39533 = CARTESIAN_POINT ( 'NONE',  ( 2.074049943651431693, 6.692913385826772199, 0.6221544894624241318 ) ) ;
#39534 = PRESENTATION_STYLE_ASSIGNMENT (( #43650 ) ) ;
#39535 = EDGE_CURVE ( 'NONE', #26405, #4443, #32315, .T. ) ;
#39536 = AXIS2_PLACEMENT_3D ( 'NONE', #4248, #28501, #11997 ) ;
#39537 = VERTEX_POINT ( 'NONE', #16373 ) ;
#39538 = EDGE_CURVE ( 'NONE', #5108, #4189, #4491, .T. ) ;
#39539 = ORIENTED_EDGE ( 'NONE', *, *, #36403, .F. ) ;
#39540 = DIRECTION ( 'NONE',  ( 1.000000000000000000, 0.000000000000000000, -3.469446951953613696E-16 ) ) ;
#39541 = LINE ( 'NONE', #20426, #4740 ) ;
#39542 = DIRECTION ( 'NONE',  ( 0.000000000000000000, 0.000000000000000000, -1.000000000000000000 ) ) ;
#39543 = ADVANCED_FACE ( 'NONE', ( #8872 ), #8618, .F. ) ;
#39544 = EDGE_LOOP ( 'NONE', ( #18636, #45056, #44623, #37505 ) ) ;
#39545 = EDGE_CURVE ( 'NONE', #16076, #31910, #5110, .T. ) ;
#39546 = EDGE_LOOP ( 'NONE', ( #14710, #28569, #14883, #49771, #9656, #35068, #3903, #44527, #41434, #41566, #13266 ) ) ;
#39547 = CARTESIAN_POINT ( 'NONE',  ( 0.5567409167160404238, 0.02445386360714798396, -1.832321260915883210 ) ) ;
#39548 = ORIENTED_EDGE ( 'NONE', *, *, #29598, .T. ) ;
#39549 = DIRECTION ( 'NONE',  ( 0.000000000000000000, 1.160734090543304660E-16, -1.000000000000000000 ) ) ;
#39550 = VERTEX_POINT ( 'NONE', #32380 ) ;
#39551 = PLANE ( 'NONE',  #23527 ) ;
#39552 = CARTESIAN_POINT ( 'NONE',  ( 0.7381027496705272473, 1.730766751998747521, -2.859439394060913298 ) ) ;
#39553 = DIRECTION ( 'NONE',  ( -1.000000000000000000, 0.000000000000000000, -0.000000000000000000 ) ) ;
#39554 = EDGE_CURVE ( 'NONE', #17224, #45778, #43459, .T. ) ;
#39555 = AXIS2_PLACEMENT_3D ( 'NONE', #393, #31640, #43495 ) ;
#39556 = B_SPLINE_CURVE_WITH_KNOTS ( 'NONE', 3,
 ( #4501, #47571, #32389, #48082 ),
 .UNSPECIFIED., .F., .F.,
 ( 4, 4 ),
 ( 0.01260738023649243464, 0.03073908182205475209 ),
 .UNSPECIFIED. ) ;
#39557 = ORIENTED_EDGE ( 'NONE', *, *, #23402, .T. ) ;
#39558 = EDGE_LOOP ( 'NONE', ( #41311, #49851, #50498, #41069 ) ) ;
#39559 = VERTEX_POINT ( 'NONE', #15602 ) ;
#39560 = DIRECTION ( 'NONE',  ( 0.8865472742777344983, 0.000000000000000000, 0.4626380123495249519 ) ) ;
#39561 = CARTESIAN_POINT ( 'NONE',  ( -1.353990537516116754, 3.244463339810032210, 2.047244094488179567 ) ) ;
#39562 = VERTEX_POINT ( 'NONE', #23594 ) ;
#39563 = VERTEX_POINT ( 'NONE', #24626 ) ;
#39564 = EDGE_CURVE ( 'NONE', #38926, #14656, #5167, .T. ) ;
#39565 = CARTESIAN_POINT ( 'NONE',  ( -1.882988517681399188, 6.692913385826772199, 1.069164917025788863 ) ) ;
#39566 = PLANE ( 'NONE',  #36824 ) ;
#39567 = CARTESIAN_POINT ( 'NONE',  ( -1.091055626815042201, 3.346456692913386100, 0.7480314960629874665 ) ) ;
#39568 = CONICAL_SURFACE ( 'NONE', #21450, 2.244934639244524632, 1.554780866114618743 ) ;
#39569 = EDGE_LOOP ( 'NONE', ( #48250, #12494, #33947, #22047 ) ) ;
#39570 = VERTEX_POINT ( 'NONE', #47049 ) ;
#39571 = VECTOR ( 'NONE', #46538, 39.37007874015748143 ) ;
#39572 = CARTESIAN_POINT ( 'NONE',  ( 0.2727639067037606613, 3.267716535433071279, -4.731699523581610974E-17 ) ) ;
#39573 = DIRECTION ( 'NONE',  ( -1.000000000000000000, -0.000000000000000000, -0.000000000000000000 ) ) ;
#39574 = ADVANCED_FACE ( 'NONE', ( #47563 ), #11722, .F. ) ;
#39575 = CARTESIAN_POINT ( 'NONE',  ( -0.8942052331142547050, 3.267716535433071279, 0.1181102362204705658 ) ) ;
#39576 = ORIENTED_EDGE ( 'NONE', *, *, #2216, .T. ) ;
#39577 = FACE_OUTER_BOUND ( 'NONE', #1079, .T. ) ;
#39578 = DIRECTION ( 'NONE',  ( -0.000000000000000000, 1.000000000000000000, -0.000000000000000000 ) ) ;
#39579 = ORIENTED_EDGE ( 'NONE', *, *, #35425, .F. ) ;
#39580 = CARTESIAN_POINT ( 'NONE',  ( 0.07982360342473591996, 1.709180471932028711, 0.000000000000000000 ) ) ;
#39581 = ORIENTED_EDGE ( 'NONE', *, *, #49471, .F. ) ;
#39582 = ORIENTED_EDGE ( 'NONE', *, *, #13621, .F. ) ;
#39583 = AXIS2_PLACEMENT_3D ( 'NONE', #24321, #11677, #40068 ) ;
#39584 = DIRECTION ( 'NONE',  ( -1.105928667600727183E-16, 1.000000000000000000, 6.607616187506045307E-17 ) ) ;
#39585 = CARTESIAN_POINT ( 'NONE',  ( -0.5455278134075208785, 0.000000000000000000, 0.9448818897637749625 ) ) ;
#39586 = ADVANCED_FACE ( 'NONE', ( #3986 ), #23853, .F. ) ;
#39587 = LINE ( 'NONE', #39077, #23096 ) ;
#39588 = CARTESIAN_POINT ( 'NONE',  ( 0.000000000000000000, 3.346456692913386100, -2.952755905511811552 ) ) ;
#39589 = CARTESIAN_POINT ( 'NONE',  ( 0.5110594979943910987, 0.000000000000000000, -1.666798357583575418 ) ) ;
#39590 = ORIENTED_EDGE ( 'NONE', *, *, #38629, .T. ) ;
#39591 = ORIENTED_EDGE ( 'NONE', *, *, #32436, .F. ) ;
#39592 = EDGE_CURVE ( 'NONE', #9076, #41777, #13517, .T. ) ;
#39593 = ORIENTED_EDGE ( 'NONE', *, *, #16845, .T. ) ;
#39594 = DIRECTION ( 'NONE',  ( 0.000000000000000000, -1.000000000000000000, 0.000000000000000000 ) ) ;
#39595 = FACE_OUTER_BOUND ( 'NONE', #7092, .T. ) ;
#39596 = ADVANCED_FACE ( 'NONE', ( #5767 ), #21771, .F. ) ;
#39597 = DIRECTION ( 'NONE',  ( 1.000000000000000000, -0.000000000000000000, 0.000000000000000000 ) ) ;
#39598 = LINE ( 'NONE', #4996, #14641 ) ;
#39599 = ORIENTED_EDGE ( 'NONE', *, *, #24436, .T. ) ;
#39600 = CARTESIAN_POINT ( 'NONE',  ( -2.182111253630085290, 3.346456692913386100, -0.1968503937007880511 ) ) ;
#39601 = CARTESIAN_POINT ( 'NONE',  ( 0.000000000000000000, 3.267716535433071279, 0.3149606299212578953 ) ) ;
#39602 = EDGE_CURVE ( 'NONE', #44569, #713, #25131, .T. ) ;
#39603 = VECTOR ( 'NONE', #39916, 39.37007874015748143 ) ;
#39604 = VERTEX_POINT ( 'NONE', #40883 ) ;
#39605 = DIRECTION ( 'NONE',  ( -1.000000000000000000, 0.000000000000000000, -0.000000000000000000 ) ) ;
#39606 = VECTOR ( 'NONE', #3964, 39.37007874015748143 ) ;
#39607 = CARTESIAN_POINT ( 'NONE',  ( 2.867773316779195447, 1.763947033723992641, -0.7050287376752004675 ) ) ;
#39608 = CARTESIAN_POINT ( 'NONE',  ( 2.919426793319799707, 1.764751637901927905, 0.4451252810446822417 ) ) ;
#39609 = EDGE_LOOP ( 'NONE', ( #4954, #49509, #16890, #33361 ) ) ;
#39610 = LINE ( 'NONE', #4239, #48979 ) ;
#39611 = CARTESIAN_POINT ( 'NONE',  ( 1.091055626815042645, 0.000000000000000000, 0.4330708661417287386 ) ) ;
#39612 = EDGE_CURVE ( 'NONE', #25030, #16032, #13009, .T. ) ;
#39613 = DIRECTION ( 'NONE',  ( 0.000000000000000000, -1.000000000000000000, 0.000000000000000000 ) ) ;
#39614 = EDGE_LOOP ( 'NONE', ( #16518, #9172, #29072, #39960 ) ) ;
#39615 = DIRECTION ( 'NONE',  ( 1.000000000000000000, 0.000000000000000000, 0.000000000000000000 ) ) ;
#39616 = VECTOR ( 'NONE', #35568, 39.37007874015748143 ) ;
#39617 = DIRECTION ( 'NONE',  ( 0.000000000000000000, 0.000000000000000000, -1.000000000000000000 ) ) ;
#39618 = VERTEX_POINT ( 'NONE', #37528 ) ;
#39619 = CARTESIAN_POINT ( 'NONE',  ( 1.363819533518803029, 0.000000000000000000, -1.732283464566923170 ) ) ;
#39620 = CARTESIAN_POINT ( 'NONE',  ( -1.166969139818016199, 3.267716535433071279, 1.535433070866133232 ) ) ;
#39621 = PLANE ( 'NONE',  #9849 ) ;
#39622 = CARTESIAN_POINT ( 'NONE',  ( -0.5455278134075214336, 0.000000000000000000, -0.8267716535433049518 ) ) ;
#39623 = ORIENTED_EDGE ( 'NONE', *, *, #44063, .F. ) ;
#39624 = VERTEX_POINT ( 'NONE', #17137 ) ;
#39625 = CARTESIAN_POINT ( 'NONE',  ( -1.843472447131334624, 1.579950168977349412, -1.157898127912315944 ) ) ;
#39626 = DIRECTION ( 'NONE',  ( 1.000000000000000000, 0.000000000000000000, 0.000000000000000000 ) ) ;
#39627 = EDGE_LOOP ( 'NONE', ( #1913, #25990, #43658, #2458 ) ) ;
#39628 = CARTESIAN_POINT ( 'NONE',  ( 0.2727639067037604392, 3.346456692913386100, -0.9842519685039348154 ) ) ;
#39629 = PLANE ( 'NONE',  #23573 ) ;
#39630 = LINE ( 'NONE', #4258, #31858 ) ;
#39631 = DIRECTION ( 'NONE',  ( 1.000000000000000000, 0.000000000000000000, 0.000000000000000000 ) ) ;
#39632 = ORIENTED_EDGE ( 'NONE', *, *, #44479, .F. ) ;
#39633 = VERTEX_POINT ( 'NONE', #20744 ) ;
#39634 = CARTESIAN_POINT ( 'NONE',  ( 1.062992125984252079, 0.5905511811023621549, 1.014069264286641792 ) ) ;
#39635 = LINE ( 'NONE', #12274, #29884 ) ;
#39636 = ADVANCED_FACE ( 'NONE', ( #37273 ), #36758, .F. ) ;
#39637 = CARTESIAN_POINT ( 'NONE',  ( 1.091055626815042645, 3.267716535433071279, 1.259842519685033357 ) ) ;
#39638 = DIRECTION ( 'NONE',  ( 1.734723475976806848E-16, 0.000000000000000000, 1.000000000000000000 ) ) ;
#39639 = FACE_BOUND ( 'NONE', #27429, .T. ) ;
#39640 = ORIENTED_EDGE ( 'NONE', *, *, #22020, .T. ) ;
#39641 = CARTESIAN_POINT ( 'NONE',  ( 2.734482843737263025, 1.761870738172414796, -1.115254632218672493 ) ) ;
#39642 = ORIENTED_EDGE ( 'NONE', *, *, #32727, .F. ) ;
#39643 = ORIENTED_EDGE ( 'NONE', *, *, #31398, .F. ) ;
#39644 = CARTESIAN_POINT ( 'NONE',  ( -2.733043338785845690E-17, 0.000000000000000000, 1.338302322423841889E-16 ) ) ;
#39645 = EDGE_CURVE ( 'NONE', #2869, #25971, #45487, .T. ) ;
#39646 = VECTOR ( 'NONE', #39473, 39.37007874015748143 ) ;
#39647 = VECTOR ( 'NONE', #10538, 39.37007874015748143 ) ;
#39648 = ADVANCED_FACE ( 'NONE', ( #25381 ), #28741, .F. ) ;
#39649 = EDGE_CURVE ( 'NONE', #41521, #28822, #5249, .T. ) ;
#39650 = ORIENTED_EDGE ( 'NONE', *, *, #12575, .T. ) ;
#39651 = ORIENTED_EDGE ( 'NONE', *, *, #1965, .T. ) ;
#39652 = LINE ( 'NONE', #47097, #23613 ) ;
#39653 = ORIENTED_EDGE ( 'NONE', *, *, #47301, .T. ) ;
#39654 = ADVANCED_FACE ( 'NONE', ( #33149 ), #29252, .F. ) ;
#39655 = CONICAL_SURFACE ( 'NONE', #62, 2.244934639244524632, 1.554780866114618743 ) ;
#39656 = CARTESIAN_POINT ( 'NONE',  ( -1.068075307999487578, 1.574803149606302854, 1.883606783264637485 ) ) ;
#39657 = CARTESIAN_POINT ( 'NONE',  ( 0.002207914879453961969, 6.692913385826772199, 0.04916304461325451958 ) ) ;
#39658 = DIRECTION ( 'NONE',  ( 0.9998717552508121775, 0.01601477604151182663, 0.000000000000000000 ) ) ;
#39659 = PLANE ( 'NONE',  #16541 ) ;
#39660 = DIRECTION ( 'NONE',  ( -0.000000000000000000, 1.000000000000000000, -0.000000000000000000 ) ) ;
#39661 = DIRECTION ( 'NONE',  ( 0.000000000000000000, -1.000000000000000000, 0.000000000000000000 ) ) ;
#39662 = ORIENTED_EDGE ( 'NONE', *, *, #16059, .F. ) ;
#39663 = CARTESIAN_POINT ( 'NONE',  ( 0.000000000000000000, 3.267716535433071279, 1.535433070866133898 ) ) ;
#39664 = CARTESIAN_POINT ( 'NONE',  ( -1.439733046521776583, 3.346456692913386100, -1.259842519685034468 ) ) ;
#39665 = DIRECTION ( 'NONE',  ( -0.000000000000000000, 1.000000000000000000, -0.000000000000000000 ) ) ;
#39666 = EDGE_CURVE ( 'NONE', #2104, #13220, #48581, .T. ) ;
#39667 = ORIENTED_EDGE ( 'NONE', *, *, #18228, .T. ) ;
#39668 = CARTESIAN_POINT ( 'NONE',  ( 1.363819533518803029, 0.000000000000000000, -1.299212598425193210 ) ) ;
#39669 = LINE ( 'NONE', #47882, #40124 ) ;
#39670 = EDGE_LOOP ( 'NONE', ( #45304, #27555, #19607, #19311, #12554 ) ) ;
#39671 = CARTESIAN_POINT ( 'NONE',  ( 1.909347346926324018, 3.346456692913386100, -0.8893194486674360633 ) ) ;
#39672 = CARTESIAN_POINT ( 'NONE',  ( 2.867773316779195447, 1.449472587384593725, -0.7050287376752005786 ) ) ;
#39673 = EDGE_CURVE ( 'NONE', #21081, #40619, #1380, .T. ) ;
#39674 = LINE ( 'NONE', #24704, #32625 ) ;
#39675 = EDGE_CURVE ( 'NONE', #10342, #34149, #1119, .T. ) ;
#39676 = CARTESIAN_POINT ( 'NONE',  ( -2.362204724409448620, 1.172985819482487146, -3.149606299212598604 ) ) ;
#39677 = CIRCLE ( 'NONE', #1752, 2.106299212598425008 ) ;
#39678 = ORIENTED_EDGE ( 'NONE', *, *, #22081, .F. ) ;
#39679 = LINE ( 'NONE', #28308, #47000 ) ;
#39680 = DIRECTION ( 'NONE',  ( 1.000000000000000000, -0.000000000000000000, 0.000000000000000000 ) ) ;
#39681 = VECTOR ( 'NONE', #40953, 39.37007874015748143 ) ;
#39682 = AXIS2_PLACEMENT_3D ( 'NONE', #45954, #38249, #7942 ) ;
#39683 = DIRECTION ( 'NONE',  ( -0.9998717552508122886, -0.01601477604151180928, 0.000000000000000000 ) ) ;
#39684 = LINE ( 'NONE', #27795, #46554 ) ;
#39685 = VERTEX_POINT ( 'NONE', #36502 ) ;
#39686 = VERTEX_POINT ( 'NONE', #9382 ) ;
#39687 = ORIENTED_EDGE ( 'NONE', *, *, #20683, .F. ) ;
#39688 = CARTESIAN_POINT ( 'NONE',  ( 1.319349709118413205, 0.000000000000000000, 1.584915398547334764 ) ) ;
#39689 = ORIENTED_EDGE ( 'NONE', *, *, #24784, .T. ) ;
#39690 = CARTESIAN_POINT ( 'NONE',  ( 0.7381027496705270252, 1.632310643118564997, -2.859439394060913298 ) ) ;
#39691 = VECTOR ( 'NONE', #41299, 39.37007874015748143 ) ;
#39692 = CARTESIAN_POINT ( 'NONE',  ( 0.2430652128771959297, 1.574803149606302854, -2.151668812760857641 ) ) ;
#39693 = VERTEX_POINT ( 'NONE', #21261 ) ;
#39694 = DIRECTION ( 'NONE',  ( 0.000000000000000000, -1.000000000000000000, 0.000000000000000000 ) ) ;
#39695 = AXIS2_PLACEMENT_3D ( 'NONE', #37654, #9513, #25257 ) ;
#39696 = VERTEX_POINT ( 'NONE', #37019 ) ;
#39697 = DIRECTION ( 'NONE',  ( -1.000000000000000000, 0.000000000000000000, -0.000000000000000000 ) ) ;
#39698 = CARTESIAN_POINT ( 'NONE',  ( 2.100227814008711835, 1.653522055412836700, -2.076109931251913565 ) ) ;
#39699 = ORIENTED_EDGE ( 'NONE', *, *, #39319, .F. ) ;
#39700 = CARTESIAN_POINT ( 'NONE',  ( 1.091055626815042423, 3.346456692913386100, -1.259842519685035134 ) ) ;
#39701 = VERTEX_POINT ( 'NONE', #1634 ) ;
#39702 = B_SPLINE_CURVE_WITH_KNOTS ( 'NONE', 3,
 ( #44860, #16756, #5383, #48205 ),
 .UNSPECIFIED., .F., .F.,
 ( 4, 4 ),
 ( 2.220059668071660630E-07, 0.002500468552710426520 ),
 .UNSPECIFIED. ) ;
#39703 = CARTESIAN_POINT ( 'NONE',  ( 1.015142113812069091, 0.000000000000000000, -1.417322834645664331 ) ) ;
#39704 = EDGE_CURVE ( 'NONE', #6926, #26859, #43919, .T. ) ;
#39705 = EDGE_CURVE ( 'NONE', #2996, #30054, #17384, .T. ) ;
#39706 = ORIENTED_EDGE ( 'NONE', *, *, #32283, .T. ) ;
#39707 = VERTEX_POINT ( 'NONE', #29517 ) ;
#39708 = DIRECTION ( 'NONE',  ( -3.469446951953613696E-16, 0.000000000000000000, -1.000000000000000000 ) ) ;
#39709 = EDGE_CURVE ( 'NONE', #9214, #1425, #45233, .T. ) ;
#39710 = CARTESIAN_POINT ( 'NONE',  ( 2.066011418817629952, 0.01968689263637172018, 0.2301982101820274906 ) ) ;
#39711 = ORIENTED_EDGE ( 'NONE', *, *, #3413, .F. ) ;
#39712 = LINE ( 'NONE', #8475, #39429 ) ;
#39713 = ORIENTED_EDGE ( 'NONE', *, *, #39768, .F. ) ;
#39714 = DIRECTION ( 'NONE',  ( 1.000000000000000000, 0.000000000000000000, -3.469446951953613696E-16 ) ) ;
#39715 = AXIS2_PLACEMENT_3D ( 'NONE', #10065, #9813, #41556 ) ;
#39716 = DIRECTION ( 'NONE',  ( 1.000000000000000000, 0.000000000000000000, 0.000000000000000000 ) ) ;
#39717 = VECTOR ( 'NONE', #39386, 39.37007874015748143 ) ;
#39718 = DIRECTION ( 'NONE',  ( -1.000000000000000000, -0.000000000000000000, -0.000000000000000000 ) ) ;
#39719 = ORIENTED_EDGE ( 'NONE', *, *, #26152, .T. ) ;
#39720 = ORIENTED_EDGE ( 'NONE', *, *, #21417, .T. ) ;
#39721 = VECTOR ( 'NONE', #7872, 39.37007874015748143 ) ;
#39722 = LINE ( 'NONE', #43833, #3052 ) ;
#39723 = DIRECTION ( 'NONE',  ( -3.469446951953613696E-16, 0.000000000000000000, -1.000000000000000000 ) ) ;
#39724 = LINE ( 'NONE', #40242, #42302 ) ;
#39725 = VECTOR ( 'NONE', #17237, 39.37007874015748143 ) ;
#39726 = EDGE_CURVE ( 'NONE', #2108, #29370, #45997, .T. ) ;
#39727 = DIRECTION ( 'NONE',  ( -5.207613805428889878E-18, -1.000000000000000000, 1.159565308550899675E-16 ) ) ;
#39728 = DIRECTION ( 'NONE',  ( -0.000000000000000000, 1.000000000000000000, -0.000000000000000000 ) ) ;
#39729 = AXIS2_PLACEMENT_3D ( 'NONE', #31804, #11660, #31545 ) ;
#39730 = EDGE_CURVE ( 'NONE', #46927, #29618, #41645, .T. ) ;
#39731 = CARTESIAN_POINT ( 'NONE',  ( -1.439733046521776139, 0.000000000000000000, 1.259842519685033357 ) ) ;
#39732 = VERTEX_POINT ( 'NONE', #46493 ) ;
#39733 = CARTESIAN_POINT ( 'NONE',  ( -1.695772546416001836, 1.594396608463251486, -2.417756147381374010 ) ) ;
#39734 = EDGE_CURVE ( 'NONE', #43301, #48914, #2654, .T. ) ;
#39735 = ORIENTED_EDGE ( 'NONE', *, *, #36057, .T. ) ;
#39736 = LINE ( 'NONE', #27338, #45675 ) ;
#39737 = EDGE_CURVE ( 'NONE', #9639, #39686, #25718, .T. ) ;
#39738 = B_SPLINE_CURVE_WITH_KNOTS ( 'NONE', 3,
 ( #30653, #7414, #6903, #18529 ),
 .UNSPECIFIED., .F., .F.,
 ( 4, 4 ),
 ( 8.019549856696441979E-05, 0.0001436088897228033647 ),
 .UNSPECIFIED. ) ;
#39739 = VERTEX_POINT ( 'NONE', #6540 ) ;
#39740 = CARTESIAN_POINT ( 'NONE',  ( 0.5465852118371267165, 0.5227683204652883164, -2.165491180797212589 ) ) ;
#39741 = CARTESIAN_POINT ( 'NONE',  ( -1.514466370293032549, 5.905511811023623991, 2.534789744887398388 ) ) ;
#39742 = CARTESIAN_POINT ( 'NONE',  ( 1.770012363201889594, 3.346456692913386100, -1.141732283464564013 ) ) ;
#39743 = ORIENTED_EDGE ( 'NONE', *, *, #4490, .F. ) ;
#39744 = CARTESIAN_POINT ( 'NONE',  ( -1.977278193622379332, 1.577807025067274882, -0.8986486843887250275 ) ) ;
#39745 = EDGE_LOOP ( 'NONE', ( #50097, #13968, #9597, #49182 ) ) ;
#39746 = DIRECTION ( 'NONE',  ( -0.000000000000000000, 1.000000000000000000, -0.000000000000000000 ) ) ;
#39747 = VERTEX_POINT ( 'NONE', #6279 ) ;
#39748 = DIRECTION ( 'NONE',  ( -0.000000000000000000, 1.000000000000000000, -0.000000000000000000 ) ) ;
#39749 = FACE_OUTER_BOUND ( 'NONE', #7089, .T. ) ;
#39750 = AXIS2_PLACEMENT_3D ( 'NONE', #7510, #19622, #27622 ) ;
#39751 = VECTOR ( 'NONE', #9798, 39.37007874015748143 ) ;
#39752 = CARTESIAN_POINT ( 'NONE',  ( 1.929629134066521701, 6.692913385826772199, 0.9824921284572420976 ) ) ;
#39753 = ORIENTED_EDGE ( 'NONE', *, *, #31071, .T. ) ;
#39754 = EDGE_LOOP ( 'NONE', ( #15191, #48528, #8004, #43885 ) ) ;
#39755 = LINE ( 'NONE', #4650, #27611 ) ;
#39756 = DIRECTION ( 'NONE',  ( -0.000000000000000000, 1.000000000000000000, -0.000000000000000000 ) ) ;
#39757 = FACE_BOUND ( 'NONE', #20904, .T. ) ;
#39758 = VECTOR ( 'NONE', #8693, 39.37007874015748143 ) ;
#39759 = ORIENTED_EDGE ( 'NONE', *, *, #4123, .T. ) ;
#39760 = DIRECTION ( 'NONE',  ( 0.9998717552508121775, 0.01601477604151182663, 0.000000000000000000 ) ) ;
#39761 = CARTESIAN_POINT ( 'NONE',  ( 2.600183657057279607, 5.905511811023623991, 1.399218491554162336 ) ) ;
#39762 = VERTEX_POINT ( 'NONE', #10405 ) ;
#39763 = LINE ( 'NONE', #4144, #22475 ) ;
#39764 = EDGE_CURVE ( 'NONE', #31670, #36537, #22029, .T. ) ;
#39765 = ADVANCED_FACE ( 'NONE', ( #18404 ), #34160, .F. ) ;
#39766 = ORIENTED_EDGE ( 'NONE', *, *, #24074, .T. ) ;
#39767 = ORIENTED_EDGE ( 'NONE', *, *, #14425, .T. ) ;
#39768 = EDGE_CURVE ( 'NONE', #28846, #35081, #3455, .T. ) ;
#39769 = ORIENTED_EDGE ( 'NONE', *, *, #4111, .T. ) ;
#39770 = DIRECTION ( 'NONE',  ( 0.9510565162951500895, 0.000000000000000000, 0.3090169943749582204 ) ) ;
#39771 = CARTESIAN_POINT ( 'NONE',  ( 0.8013550346897827525, 1.731743580627177925, -2.841982872583248998 ) ) ;
#39772 = B_SPLINE_CURVE_WITH_KNOTS ( 'NONE', 3,
 ( #37898, #2519, #46606, #30134 ),
 .UNSPECIFIED., .F., .F.,
 ( 4, 4 ),
 ( 0.01111952476426258593, 0.03073605569767426729 ),
 .UNSPECIFIED. ) ;
#39773 = CARTESIAN_POINT ( 'NONE',  ( -1.091055626815042645, 3.346456692913386100, 1.692913385826762873 ) ) ;
#39774 = DIRECTION ( 'NONE',  ( -0.000000000000000000, 1.000000000000000000, -0.000000000000000000 ) ) ;
#39775 = ORIENTED_EDGE ( 'NONE', *, *, #37803, .T. ) ;
#39776 = ORIENTED_EDGE ( 'NONE', *, *, #16701, .F. ) ;
#39777 = CARTESIAN_POINT ( 'NONE',  ( -2.084291548511494785, 5.905511811023623991, 0.6254821886024592992 ) ) ;
#39778 = PLANE ( 'NONE',  #38666 ) ;
#39779 = DIRECTION ( 'NONE',  ( -0.000000000000000000, 1.000000000000000000, -0.000000000000000000 ) ) ;
#39780 = VERTEX_POINT ( 'NONE', #26894 ) ;
#39781 = CARTESIAN_POINT ( 'NONE',  ( -1.486187880958815377, 3.346456692913386100, -1.574803149606293307 ) ) ;
#39782 = PLANE ( 'NONE',  #20657 ) ;
#39783 = VECTOR ( 'NONE', #40024, 39.37007874015748143 ) ;
#39784 = ADVANCED_FACE ( 'NONE', ( #46244 ), #26397, .F. ) ;
#39785 = LINE ( 'NONE', #20416, #42447 ) ;
#39786 = LINE ( 'NONE', #43646, #11855 ) ;
#39787 = LINE ( 'NONE', #20155, #2166 ) ;
#39788 = ORIENTED_EDGE ( 'NONE', *, *, #45555, .F. ) ;
#39789 = PLANE ( 'NONE',  #5277 ) ;
#39790 = LENGTH_MEASURE_WITH_UNIT ( LENGTH_MEASURE( 0.02539999999999999897 ), #4685 );
#39791 = EDGE_CURVE ( 'NONE', #3695, #4193, #6782, .T. ) ;
#39792 = VECTOR ( 'NONE', #15074, 39.37007874015748143 ) ;
#39793 = ORIENTED_EDGE ( 'NONE', *, *, #20707, .T. ) ;
#39794 = VECTOR ( 'NONE', #29756, 39.37007874015748143 ) ;
#39795 = ORIENTED_EDGE ( 'NONE', *, *, #44790, .F. ) ;
#39796 = VECTOR ( 'NONE', #6207, 39.37007874015748143 ) ;
#39797 = LINE ( 'NONE', #8042, #43871 ) ;
#39798 = CARTESIAN_POINT ( 'NONE',  ( 0.5455278134075213226, 3.267716535433071279, -9.463399047163224412E-17 ) ) ;
#39799 = CARTESIAN_POINT ( 'NONE',  ( 2.121469926805689354, 1.574803149606302854, -0.4337334748181394528 ) ) ;
#39800 = ORIENTED_EDGE ( 'NONE', *, *, #25290, .T. ) ;
#39801 = ORIENTED_EDGE ( 'NONE', *, *, #9588, .T. ) ;
#39802 = CARTESIAN_POINT ( 'NONE',  ( 0.000000000000000000, 3.267716535433071279, -0.3149606299212596716 ) ) ;
#39803 = VERTEX_POINT ( 'NONE', #42645 ) ;
#39804 = DIRECTION ( 'NONE',  ( -3.469446951953613696E-16, 0.000000000000000000, -1.000000000000000000 ) ) ;
#39805 = EDGE_LOOP ( 'NONE', ( #31208, #2830, #35970, #35479 ) ) ;
#39806 = DIRECTION ( 'NONE',  ( 0.000000000000000000, 0.000000000000000000, -1.000000000000000000 ) ) ;
#39807 = CARTESIAN_POINT ( 'NONE',  ( 0.1450362469327826365, 1.574803149606302854, -2.160491579385212191 ) ) ;
#39808 = CARTESIAN_POINT ( 'NONE',  ( -1.166969139818015977, 0.000000000000000000, -1.732283464566922726 ) ) ;
#39809 = VERTEX_POINT ( 'NONE', #34409 ) ;
#39810 = ORIENTED_EDGE ( 'NONE', *, *, #17814, .T. ) ;
#39811 = ORIENTED_EDGE ( 'NONE', *, *, #33757, .F. ) ;
#39812 = PLANE ( 'NONE',  #14993 ) ;
#39813 = CARTESIAN_POINT ( 'NONE',  ( 0.000000000000000000, 3.267716535433071279, 0.4330708661417287386 ) ) ;
#39814 = ORIENTED_EDGE ( 'NONE', *, *, #28818, .F. ) ;
#39815 = ORIENTED_EDGE ( 'NONE', *, *, #621, .T. ) ;
#39816 = CARTESIAN_POINT ( 'NONE',  ( -0.3486774197067334380, 3.267716535433071279, 1.889763779527550369 ) ) ;
#39817 = DIRECTION ( 'NONE',  ( -0.000000000000000000, 1.000000000000000000, -0.000000000000000000 ) ) ;
#39818 = CARTESIAN_POINT ( 'NONE',  ( 2.052631463899901920, 3.267716535433071279, -0.4724409448818889246 ) ) ;
#39819 = ORIENTED_EDGE ( 'NONE', *, *, #4548, .T. ) ;
#39820 = CARTESIAN_POINT ( 'NONE',  ( 0.002207914879453961535, -5.712274067634378313E-18, 0.04916304461325374242 ) ) ;
#39821 = DIRECTION ( 'NONE',  ( 0.000000000000000000, 0.000000000000000000, -1.000000000000000000 ) ) ;
#39822 = CARTESIAN_POINT ( 'NONE',  ( -0.1450934409768894484, 5.905511811023623991, 2.161127057262024920 ) ) ;
#39823 = VERTEX_POINT ( 'NONE', #38290 ) ;
#39824 = DIRECTION ( 'NONE',  ( 0.000000000000000000, 0.000000000000000000, -1.000000000000000000 ) ) ;
#39825 = VECTOR ( 'NONE', #11445, 39.37007874015748143 ) ;
#39826 = CARTESIAN_POINT ( 'NONE',  ( -0.7514907335614920969, 0.005366325807348728584, -1.673910055625482451 ) ) ;
#39827 = EDGE_CURVE ( 'NONE', #6728, #49076, #22785, .T. ) ;
#39828 = VERTEX_POINT ( 'NONE', #3157 ) ;
#39829 = EDGE_CURVE ( 'NONE', #33976, #3507, #8822, .T. ) ;
#39830 = DIRECTION ( 'NONE',  ( -3.469446951953613696E-16, 0.000000000000000000, -1.000000000000000000 ) ) ;
#39831 = ORIENTED_EDGE ( 'NONE', *, *, #14475, .F. ) ;
#39832 = ORIENTED_EDGE ( 'NONE', *, *, #16059, .T. ) ;
#39833 = PLANE ( 'NONE',  #35335 ) ;
#39834 = CARTESIAN_POINT ( 'NONE',  ( -1.363819533518803473, 0.000000000000000000, -1.929133858267710000 ) ) ;
#39835 = ADVANCED_FACE ( 'NONE', ( #10905 ), #33987, .T. ) ;
#39836 = VECTOR ( 'NONE', #15013, 39.37007874015748143 ) ;
#39837 = VECTOR ( 'NONE', #6400, 39.37007874015748143 ) ;
#39838 = DIRECTION ( 'NONE',  ( 1.241861098869884156E-16, 1.000000000000000000, 3.427318860986280993E-17 ) ) ;
#39839 = EDGE_CURVE ( 'NONE', #36136, #47107, #34709, .T. ) ;
#39840 = CARTESIAN_POINT ( 'NONE',  ( 0.3546377434558362074, 1.615156926475952881, 2.229828021450985798 ) ) ;
#39841 = EDGE_CURVE ( 'NONE', #45101, #26202, #7036, .T. ) ;
#39842 = PLANE ( 'NONE',  #50971 ) ;
#39843 = EDGE_LOOP ( 'NONE', ( #41051, #35379, #4535, #10200 ) ) ;
#39844 = ORIENTED_EDGE ( 'NONE', *, *, #2535, .T. ) ;
#39845 = VECTOR ( 'NONE', #7161, 39.37007874015748143 ) ;
#39846 = ORIENTED_EDGE ( 'NONE', *, *, #18290, .F. ) ;
#39847 = DIRECTION ( 'NONE',  ( 1.000000000000000000, 0.000000000000000000, -3.469446951953613696E-16 ) ) ;
#39848 = DIRECTION ( 'NONE',  ( -0.000000000000000000, 1.000000000000000000, -0.000000000000000000 ) ) ;
#39849 = ADVANCED_FACE ( 'NONE', ( #17555 ), #26063, .F. ) ;
#39850 = DIRECTION ( 'NONE',  ( -3.469446951953613696E-16, 0.000000000000000000, -1.000000000000000000 ) ) ;
#39851 = DIRECTION ( 'NONE',  ( -0.1342332658176667304, -1.160734090543304907E-16, 0.9909497617679332571 ) ) ;
#39852 = CARTESIAN_POINT ( 'NONE',  ( 0.000000000000000000, 3.267716535433071279, 0.1574803149606286423 ) ) ;
#39853 = VERTEX_POINT ( 'NONE', #49001 ) ;
#39854 = DIRECTION ( 'NONE',  ( -0.000000000000000000, -1.000000000000000000, -0.000000000000000000 ) ) ;
#39855 = ADVANCED_FACE ( 'NONE', ( #29163 ), #1293, .F. ) ;
#39856 = LINE ( 'NONE', #4748, #33138 ) ;
#39857 = ORIENTED_EDGE ( 'NONE', *, *, #2853, .F. ) ;
#39858 = DIRECTION ( 'NONE',  ( -0.000000000000000000, 1.000000000000000000, -0.000000000000000000 ) ) ;
#39859 = CARTESIAN_POINT ( 'NONE',  ( 1.363819533518803251, 0.000000000000000000, -0.3543307086614178592 ) ) ;
#39860 = DIRECTION ( 'NONE',  ( 1.000000000000000000, 0.000000000000000000, 0.000000000000000000 ) ) ;
#39861 = EDGE_CURVE ( 'NONE', #12697, #42646, #26207, .T. ) ;
#39862 = ORIENTED_EDGE ( 'NONE', *, *, #41634, .T. ) ;
#39863 = CARTESIAN_POINT ( 'NONE',  ( 0.000000000000000000, 1.574803149606302854, 0.000000000000000000 ) ) ;
#39864 = CARTESIAN_POINT ( 'NONE',  ( 2.298322628623565400, 1.462353850267382738, 1.853847351054373371 ) ) ;
#39865 = CARTESIAN_POINT ( 'NONE',  ( -2.688839661887661325, 1.574817859957791999, -0.07149372627020672555 ) ) ;
#39866 = VECTOR ( 'NONE', #19118, 39.37007874015748143 ) ;
#39867 = VERTEX_POINT ( 'NONE', #18070 ) ;
#39868 = AXIS2_PLACEMENT_3D ( 'NONE', #32196, #24948, #47885 ) ;
#39869 = CARTESIAN_POINT ( 'NONE',  ( 0.8182917201112819283, 3.346456692913386100, 0.4724409448818868706 ) ) ;
#39870 = DIRECTION ( 'NONE',  ( -1.000000000000000000, 0.000000000000000000, 1.734723475976806848E-16 ) ) ;
#39871 = VERTEX_POINT ( 'NONE', #45403 ) ;
#39872 = CARTESIAN_POINT ( 'NONE',  ( -0.5455278134075208785, 3.346456692913386100, 1.062992125984246083 ) ) ;
#39873 = EDGE_CURVE ( 'NONE', #23012, #15854, #44900, .T. ) ;
#39874 = VECTOR ( 'NONE', #31980, 39.37007874015748143 ) ;
#39875 = VECTOR ( 'NONE', #28477, 39.37007874015748143 ) ;
#39876 = FACE_OUTER_BOUND ( 'NONE', #26293, .T. ) ;
#39877 = CARTESIAN_POINT ( 'NONE',  ( -1.675546303352015709, 1.681065010344670041, 1.399148864732502995 ) ) ;
#39878 = DIRECTION ( 'NONE',  ( 1.000000000000000000, 0.000000000000000000, -3.469446951953613696E-16 ) ) ;
#39879 = ORIENTED_EDGE ( 'NONE', *, *, #15908, .T. ) ;
#39880 = ORIENTED_EDGE ( 'NONE', *, *, #16760, .T. ) ;
#39881 = DIRECTION ( 'NONE',  ( -3.469446951953613696E-16, 0.000000000000000000, -1.000000000000000000 ) ) ;
#39882 = VECTOR ( 'NONE', #42202, 39.37007874015748143 ) ;
#39883 = DIRECTION ( 'NONE',  ( -3.469446951953613696E-16, 0.000000000000000000, -1.000000000000000000 ) ) ;
#39884 = ORIENTED_EDGE ( 'NONE', *, *, #1271, .T. ) ;
#39885 = CARTESIAN_POINT ( 'NONE',  ( 1.091055626815042645, 0.000000000000000000, -0.3149606299212596716 ) ) ;
#39886 = LINE ( 'NONE', #27744, #34324 ) ;
#39887 = FACE_OUTER_BOUND ( 'NONE', #36227, .T. ) ;
#39888 = DIRECTION ( 'NONE',  ( -0.01601477604151182663, 0.9998717552508123996, -0.000000000000000000 ) ) ;
#39889 = VERTEX_POINT ( 'NONE', #25552 ) ;
#39890 = ORIENTED_EDGE ( 'NONE', *, *, #2655, .F. ) ;
#39891 = DIRECTION ( 'NONE',  ( -1.729310098865080642E-17, 1.000000000000000000, 1.276627980444840260E-16 ) ) ;
#39892 = DIRECTION ( 'NONE',  ( -0.000000000000000000, 1.000000000000000000, -0.000000000000000000 ) ) ;
#39893 = LINE ( 'NONE', #43747, #18925 ) ;
#39894 = FACE_OUTER_BOUND ( 'NONE', #17317, .T. ) ;
#39895 = FACE_BOUND ( 'NONE', #26697, .T. ) ;
#39896 = ORIENTED_EDGE ( 'NONE', *, *, #32335, .F. ) ;
#39897 = CARTESIAN_POINT ( 'NONE',  ( 1.771435203777392386, 1.736274727556916808, 1.475617711110977615 ) ) ;
#39898 = ORIENTED_EDGE ( 'NONE', *, *, #18195, .T. ) ;
#39899 = EDGE_LOOP ( 'NONE', ( #6801, #31735, #46231, #3686 ) ) ;
#39900 = CARTESIAN_POINT ( 'NONE',  ( 2.491402175429654253, 1.758084086496218612, -1.585592796919505609 ) ) ;
#39901 = ADVANCED_FACE ( 'NONE', ( #20915 ), #28906, .T. ) ;
#39902 = EDGE_CURVE ( 'NONE', #45331, #33133, #17990, .T. ) ;
#39903 = ORIENTED_EDGE ( 'NONE', *, *, #45021, .F. ) ;
#39904 = ORIENTED_EDGE ( 'NONE', *, *, #36468, .T. ) ;
#39905 = DIRECTION ( 'NONE',  ( -1.000000000000000000, 0.000000000000000000, 1.734723475976806848E-16 ) ) ;
#39906 = EDGE_CURVE ( 'NONE', #12681, #18049, #32244, .T. ) ;
#39907 = VERTEX_POINT ( 'NONE', #13179 ) ;
#39908 = AXIS2_PLACEMENT_3D ( 'NONE', #15641, #41809, #18311 ) ;
#39909 = VECTOR ( 'NONE', #37196, 39.37007874015748143 ) ;
#39910 = VECTOR ( 'NONE', #34043, 39.37007874015748143 ) ;
#39911 = CARTESIAN_POINT ( 'NONE',  ( 0.2727639067037604947, 0.000000000000000000, -0.7874015748031473194 ) ) ;
#39912 = CARTESIAN_POINT ( 'NONE',  ( 0.8013550346330908791, 1.633286922350572379, -2.841982872598894705 ) ) ;
#39913 = CARTESIAN_POINT ( 'NONE',  ( -0.4433489891367859981, 5.905511811023623991, 2.167441310503416041 ) ) ;
#39914 = VECTOR ( 'NONE', #22306, 39.37007874015748143 ) ;
#39915 = CIRCLE ( 'NONE', #1997, 2.165354330708661568 ) ;
#39916 = DIRECTION ( 'NONE',  ( -3.469446951953613696E-16, 0.000000000000000000, -1.000000000000000000 ) ) ;
#39917 = LINE ( 'NONE', #43519, #37715 ) ;
#39918 = LINE ( 'NONE', #1189, #44332 ) ;
#39919 = VECTOR ( 'NONE', #6722, 39.37007874015748143 ) ;
#39920 = ORIENTED_EDGE ( 'NONE', *, *, #21141, .F. ) ;
#39921 = DIRECTION ( 'NONE',  ( 1.734723475976806848E-16, 0.000000000000000000, 1.000000000000000000 ) ) ;
#39922 = LINE ( 'NONE', #19019, #15281 ) ;
#39923 = FACE_OUTER_BOUND ( 'NONE', #15600, .T. ) ;
#39924 = ORIENTED_EDGE ( 'NONE', *, *, #37414, .F. ) ;
#39925 = FACE_OUTER_BOUND ( 'NONE', #23243, .T. ) ;
#39926 = DIRECTION ( 'NONE',  ( 0.000000000000000000, 1.000000000000000000, 0.000000000000000000 ) ) ;
#39927 = ORIENTED_EDGE ( 'NONE', *, *, #49519, .T. ) ;
#39928 = CARTESIAN_POINT ( 'NONE',  ( 0.2727639067037604947, 0.000000000000000000, -0.4724409448818886470 ) ) ;
#39929 = EDGE_CURVE ( 'NONE', #47107, #20029, #21686, .T. ) ;
#39930 = DIRECTION ( 'NONE',  ( 0.000000000000000000, 0.000000000000000000, 1.000000000000000000 ) ) ;
#39931 = CARTESIAN_POINT ( 'NONE',  ( -1.122047244094487750, 0.5314960629921255952, 1.062992125984251413 ) ) ;
#39932 = VERTEX_POINT ( 'NONE', #2063 ) ;
#39933 = ORIENTED_EDGE ( 'NONE', *, *, #21921, .T. ) ;
#39934 = CARTESIAN_POINT ( 'NONE',  ( 0.8182917201112821504, 3.267716535433071279, -1.419509857074483539E-16 ) ) ;
#39935 = ADVANCED_FACE ( 'NONE', ( #2317 ), #9557, .F. ) ;
#39936 = CARTESIAN_POINT ( 'NONE',  ( 0.3699615006857430166, 0.000000000000000000, 0.02732463576302828281 ) ) ;
#39937 = LINE ( 'NONE', #1208, #5308 ) ;
#39938 = DIRECTION ( 'NONE',  ( -0.6910626489868685329, 1.288287287306305776E-16, 0.7227948638273880011 ) ) ;
#39939 = EDGE_CURVE ( 'NONE', #18246, #27191, #41068, .T. ) ;
#39940 = B_SPLINE_CURVE_WITH_KNOTS ( 'NONE', 3,
 ( #44375, #48722, #29137, #36906 ),
 .UNSPECIFIED., .F., .F.,
 ( 4, 4 ),
 ( 2.220417365849702369E-07, 0.01713232808254949724 ),
 .UNSPECIFIED. ) ;
#39941 = PRODUCT_DEFINITION_FORMATION_WITH_SPECIFIED_SOURCE ( 'ANY', '', #35980, .NOT_KNOWN. ) ;
#39942 = ORIENTED_EDGE ( 'NONE', *, *, #49143, .F. ) ;
#39943 = VERTEX_POINT ( 'NONE', #33063 ) ;
#39944 = AXIS2_PLACEMENT_3D ( 'NONE', #29826, #41700, #6337 ) ;
#39945 = CARTESIAN_POINT ( 'NONE',  ( 1.223349603905365068, 0.04751384826852676074, 1.475034436811822669 ) ) ;
#39946 = ORIENTED_EDGE ( 'NONE', *, *, #2313, .F. ) ;
#39947 = EDGE_CURVE ( 'NONE', #30279, #18986, #49262, .T. ) ;
#39948 = AXIS2_PLACEMENT_3D ( 'NONE', #9973, #38113, #10484 ) ;
#39949 = LINE ( 'NONE', #30935, #38454 ) ;
#39950 = ORIENTED_EDGE ( 'NONE', *, *, #5922, .F. ) ;
#39951 = EDGE_CURVE ( 'NONE', #46754, #37143, #32811, .T. ) ;
#39952 = AXIS2_PLACEMENT_3D ( 'NONE', #1256, #1762, #28616 ) ;
#39953 = CARTESIAN_POINT ( 'NONE',  ( 0.7423782071083084855, 3.346456692913386100, -2.034117492951036166 ) ) ;
#39954 = ORIENTED_EDGE ( 'NONE', *, *, #2477, .T. ) ;
#39955 = DIRECTION ( 'NONE',  ( 0.000000000000000000, 0.000000000000000000, -1.000000000000000000 ) ) ;
#39956 = CARTESIAN_POINT ( 'NONE',  ( 2.932638728931774352, 1.447899366913586672, 0.3475908556738225297 ) ) ;
#39957 = CONICAL_SURFACE ( 'NONE', #17705, 2.165354330708661568, 0.2617993877991570129 ) ;
#39958 = VERTEX_POINT ( 'NONE', #49507 ) ;
#39959 = DIRECTION ( 'NONE',  ( -0.000000000000000000, 1.000000000000000000, -0.000000000000000000 ) ) ;
#39960 = ORIENTED_EDGE ( 'NONE', *, *, #43118, .F. ) ;
#39961 = EDGE_CURVE ( 'NONE', #19788, #25553, #46800, .T. ) ;
#39962 = DIRECTION ( 'NONE',  ( -0.000000000000000000, 1.000000000000000000, -0.000000000000000000 ) ) ;
#39963 = EDGE_LOOP ( 'NONE', ( #38832, #33928, #10619, #48680 ) ) ;
#39964 = VERTEX_POINT ( 'NONE', #17055 ) ;
#39965 = EDGE_CURVE ( 'NONE', #37644, #39618, #17307, .T. ) ;
#39966 = EDGE_CURVE ( 'NONE', #18328, #37294, #30335, .T. ) ;
#39967 = LINE ( 'NONE', #4094, #10820 ) ;
#39968 = EDGE_CURVE ( 'NONE', #20299, #8395, #22448, .T. ) ;
#39969 = PLANE ( 'NONE',  #6461 ) ;
#39970 = EDGE_LOOP ( 'NONE', ( #46542, #48424, #29440, #7969 ) ) ;
#39971 = DIRECTION ( 'NONE',  ( -0.01601477604151182663, 0.9998717552508123996, -0.000000000000000000 ) ) ;
#39972 = VERTEX_POINT ( 'NONE', #11077 ) ;
#39973 = DIRECTION ( 'NONE',  ( -0.000000000000000000, 1.000000000000000000, -0.000000000000000000 ) ) ;
#39974 = CARTESIAN_POINT ( 'NONE',  ( -0.5455278134075211005, 3.267716535433071279, 9.463399047163218249E-17 ) ) ;
#39975 = LINE ( 'NONE', #4606, #34636 ) ;
#39976 = VERTEX_POINT ( 'NONE', #42065 ) ;
#39977 = ORIENTED_EDGE ( 'NONE', *, *, #39068, .T. ) ;
#39978 = CARTESIAN_POINT ( 'NONE',  ( 0.000000000000000000, 0.000000000000000000, 0.000000000000000000 ) ) ;
#39979 = DIRECTION ( 'NONE',  ( 1.734723475976806848E-16, -0.000000000000000000, 1.000000000000000000 ) ) ;
#39980 = FACE_OUTER_BOUND ( 'NONE', #11489, .T. ) ;
#39981 = VECTOR ( 'NONE', #46801, 39.37007874015748143 ) ;
#39982 = CARTESIAN_POINT ( 'NONE',  ( 0.8069532150559727279, 5.905511811023623991, -2.010061882867130834 ) ) ;
#39983 = VECTOR ( 'NONE', #35243, 39.37007874015748143 ) ;
#39984 = LINE ( 'NONE', #47687, #44599 ) ;
#39985 = DIRECTION ( 'NONE',  ( -0.000000000000000000, 1.000000000000000000, -0.000000000000000000 ) ) ;
#39986 = ORIENTED_EDGE ( 'NONE', *, *, #26950, .T. ) ;
#39987 = ADVANCED_FACE ( 'NONE', ( #26562 ), #50017, .F. ) ;
#39988 = CARTESIAN_POINT ( 'NONE',  ( 0.000000000000000000, 3.267716535433071279, 0.2755905511810996522 ) ) ;
#39989 = AXIS2_PLACEMENT_3D ( 'NONE', #42868, #15760, #46963 ) ;
#39990 = ORIENTED_EDGE ( 'NONE', *, *, #12328, .T. ) ;
#39991 = DIRECTION ( 'NONE',  ( 1.000000000000000000, 0.000000000000000000, 0.000000000000000000 ) ) ;
#39992 = ORIENTED_EDGE ( 'NONE', *, *, #39245, .F. ) ;
#39993 = ADVANCED_FACE ( 'NONE', ( #50758 ), #2570, .T. ) ;
#39994 = CARTESIAN_POINT ( 'NONE',  ( 1.015142113812069313, 3.267716535433071279, -0.1574803149606301411 ) ) ;
#39995 = DIRECTION ( 'NONE',  ( -0.000000000000000000, 1.000000000000000000, -0.000000000000000000 ) ) ;
#39996 = EDGE_CURVE ( 'NONE', #9706, #26586, #24281, .T. ) ;
#39997 = PLANE ( 'NONE',  #44868 ) ;
#39998 =( BOUNDED_CURVE ( )  B_SPLINE_CURVE ( 3, ( #41902, #34163, #38785, #49849 ),
 .UNSPECIFIED., .F., .F. ) 
 B_SPLINE_CURVE_WITH_KNOTS ( ( 4, 4 ),
 ( 0.2938456066950616563, 0.7568805744475686215 ),
 .UNSPECIFIED. ) 
 CURVE ( )  GEOMETRIC_REPRESENTATION_ITEM ( )  RATIONAL_B_SPLINE_CURVE ( ( 1.000000000000000000, 0.9822128812423629451, 0.9822128812423629451, 1.000000000000000000 ) ) 
 REPRESENTATION_ITEM ( '' )  );
#39999 = ORIENTED_EDGE ( 'NONE', *, *, #1851, .F. ) ;
#40000 = EDGE_CURVE ( 'NONE', #32953, #36796, #3131, .T. ) ;
#40001 = CARTESIAN_POINT ( 'NONE',  ( -2.153807523435208093, -5.072058324879254713E-17, 0.2420910006175685525 ) ) ;
#40002 = EDGE_CURVE ( 'NONE', #37788, #49027, #18316, .T. ) ;
#40003 = FACE_BOUND ( 'NONE', #46343, .T. ) ;
#40004 = ORIENTED_EDGE ( 'NONE', *, *, #26626, .T. ) ;
#40005 = DIRECTION ( 'NONE',  ( 1.000000000000000000, 0.000000000000000000, 0.000000000000000000 ) ) ;
#40006 = EDGE_LOOP ( 'NONE', ( #10663, #43743, #12279, #36414 ) ) ;
#40007 = PLANE ( 'NONE',  #1320 ) ;
#40008 = CARTESIAN_POINT ( 'NONE',  ( -0.5455278134075214336, 0.000000000000000000, -1.771653543307081025 ) ) ;
#40009 = CARTESIAN_POINT ( 'NONE',  ( 1.363819533518803251, 3.267716535433071279, 0.7874015748031454320 ) ) ;
#40010 = AXIS2_PLACEMENT_3D ( 'NONE', #32767, #48446, #13133 ) ;
#40011 = EDGE_LOOP ( 'NONE', ( #50259, #7048, #8721, #46618, #31009 ) ) ;
#40012 = ORIENTED_EDGE ( 'NONE', *, *, #5828, .T. ) ;
#40013 = AXIS2_PLACEMENT_3D ( 'NONE', #13229, #44693, #3119 ) ;
#40014 = CARTESIAN_POINT ( 'NONE',  ( 1.287906020515830141, 3.346456692913386100, 0.7480314960629872445 ) ) ;
#40015 = FACE_OUTER_BOUND ( 'NONE', #15456, .T. ) ;
#40016 = CARTESIAN_POINT ( 'NONE',  ( 0.000000000000000000, 3.267716535433071279, -0.7874015748031470974 ) ) ;
#40017 = EDGE_CURVE ( 'NONE', #17176, #30581, #12582, .T. ) ;
#40018 = CIRCLE ( 'NONE', #46585, 2.246510896728926010 ) ;
#40019 = EDGE_CURVE ( 'NONE', #41514, #272, #18576, .T. ) ;
#40020 = DIRECTION ( 'NONE',  ( 1.000000000000000000, -0.000000000000000000, 0.000000000000000000 ) ) ;
#40021 = DIRECTION ( 'NONE',  ( -6.394449067488625930E-17, -1.000000000000000000, 9.687176266499597757E-17 ) ) ;
#40022 = ORIENTED_EDGE ( 'NONE', *, *, #5295, .F. ) ;
#40023 = ADVANCED_FACE ( 'NONE', ( #49759 ), #31204, .F. ) ;
#40024 = DIRECTION ( 'NONE',  ( 0.000000000000000000, -1.000000000000000000, -0.000000000000000000 ) ) ;
#40025 = VECTOR ( 'NONE', #2234, 39.37007874015748143 ) ;
#40026 = EDGE_CURVE ( 'NONE', #49387, #42296, #3077, .T. ) ;
#40027 = ORIENTED_EDGE ( 'NONE', *, *, #730, .T. ) ;
#40028 = VERTEX_POINT ( 'NONE', #3580 ) ;
#40029 = PRODUCT_CONTEXT ( 'NONE', #49646, 'mechanical' ) ;
#40030 = VERTEX_POINT ( 'NONE', #50262 ) ;
#40031 = DIRECTION ( 'NONE',  ( 0.000000000000000000, 0.000000000000000000, 1.000000000000000000 ) ) ;
#40032 = FACE_OUTER_BOUND ( 'NONE', #20843, .T. ) ;
#40033 = CARTESIAN_POINT ( 'NONE',  ( -0.5455278134075208785, 0.000000000000000000, 0.9448818897637749625 ) ) ;
#40034 = CYLINDRICAL_SURFACE ( 'NONE', #23871, 2.165354330708661568 ) ;
#40035 = ORIENTED_EDGE ( 'NONE', *, *, #7, .T. ) ;
#40036 = ORIENTED_EDGE ( 'NONE', *, *, #43911, .T. ) ;
#40037 = DIRECTION ( 'NONE',  ( 1.734723475976806848E-16, 0.000000000000000000, 1.000000000000000000 ) ) ;
#40038 = CARTESIAN_POINT ( 'NONE',  ( -0.6214413264104939882, 3.346456692913386100, 1.732283464566921172 ) ) ;
#40039 = CARTESIAN_POINT ( 'NONE',  ( -0.2727639067037608278, 0.000000000000000000, -0.6692913385826758654 ) ) ;
#40040 = LINE ( 'NONE', #19383, #27608 ) ;
#40041 = DIRECTION ( 'NONE',  ( 1.734723475976806848E-16, 0.000000000000000000, 1.000000000000000000 ) ) ;
#40042 = DIRECTION ( 'NONE',  ( -0.000000000000000000, 0.000000000000000000, 1.000000000000000000 ) ) ;
#40043 = CARTESIAN_POINT ( 'NONE',  ( 0.000000000000000000, 3.267716535433071279, 0.000000000000000000 ) ) ;
#40044 = PLANE ( 'NONE',  #37627 ) ;
#40045 = ORIENTED_EDGE ( 'NONE', *, *, #37478, .F. ) ;
#40046=STYLED_ITEM('',(#51080),#23876);
#40047 = DIRECTION ( 'NONE',  ( 0.000000000000000000, -1.000000000000000000, 0.000000000000000000 ) ) ;
#40048 = CARTESIAN_POINT ( 'NONE',  ( -0.2727639067037607723, 3.346456692913386100, -1.102362204724405714 ) ) ;
#40049 = VECTOR ( 'NONE', #25205, 39.37007874015748143 ) ;
#40050 = ORIENTED_EDGE ( 'NONE', *, *, #13134, .T. ) ;
#40051 = AXIS2_PLACEMENT_3D ( 'NONE', #47587, #36023, #8135 ) ;
#40052 = EDGE_LOOP ( 'NONE', ( #21714, #26864, #22826, #13896, #135, #31045, #16181, #41915, #42316, #7638, #44965, #27032, #29267, #24080, #48665, #43035, #5807, #30149, #13513, #10854, #15030, #25174, #49376, #38834 ) ) ;
#40053 = DIRECTION ( 'NONE',  ( 1.000000000000000000, -0.000000000000000000, 0.000000000000000000 ) ) ;
#40054 = DIRECTION ( 'NONE',  ( -0.9362348706397417564, 0.000000000000000000, 0.3513748240813304724 ) ) ;
#40055 = DIRECTION ( 'NONE',  ( -0.000000000000000000, 1.000000000000000000, -0.000000000000000000 ) ) ;
#40056 = EDGE_CURVE ( 'NONE', #17956, #18819, #30452, .T. ) ;
#40057 = VECTOR ( 'NONE', #17365, 39.37007874015748143 ) ;
#40058 = ORIENTED_EDGE ( 'NONE', *, *, #50443, .T. ) ;
#40059 = EDGE_CURVE ( 'NONE', #39624, #5523, #22200, .T. ) ;
#40060 = AXIS2_PLACEMENT_3D ( 'NONE', #50242, #14427, #25786 ) ;
#40061 = EDGE_CURVE ( 'NONE', #50100, #22884, #10573, .T. ) ;
#40062 = ORIENTED_EDGE ( 'NONE', *, *, #34627, .T. ) ;
#40063 = CARTESIAN_POINT ( 'NONE',  ( -0.8182917201112814842, 0.000000000000000000, 1.220472440944875281 ) ) ;
#40064 = ORIENTED_EDGE ( 'NONE', *, *, #21321, .F. ) ;
#40065 = DIRECTION ( 'NONE',  ( 1.734723475976806848E-16, 0.000000000000000000, 1.000000000000000000 ) ) ;
#40066 = ORIENTED_EDGE ( 'NONE', *, *, #16524, .T. ) ;
#40067 = DIRECTION ( 'NONE',  ( 1.734723475976806848E-16, -0.000000000000000000, 1.000000000000000000 ) ) ;
#40068 = DIRECTION ( 'NONE',  ( -1.000000000000000000, 0.000000000000000000, -0.000000000000000000 ) ) ;
#40069 = CARTESIAN_POINT ( 'NONE',  ( 0.000000000000000000, 3.267716535433071279, 0.000000000000000000 ) ) ;
#40070 = VERTEX_POINT ( 'NONE', #42567 ) ;
#40071 = ORIENTED_EDGE ( 'NONE', *, *, #44896, .T. ) ;
#40072 = EDGE_LOOP ( 'NONE', ( #44735, #1116, #44117, #1525 ) ) ;
#40073 = CARTESIAN_POINT ( 'NONE',  ( 0.9542980589831819849, 0.02856680792132131746, 1.693175744540320604 ) ) ;
#40074 = ORIENTED_EDGE ( 'NONE', *, *, #14285, .T. ) ;
#40075 = ORIENTED_EDGE ( 'NONE', *, *, #22351, .F. ) ;
#40076 = CARTESIAN_POINT ( 'NONE',  ( -1.557927422371237158, 0.000000000000000000, 0.7824709080581183640 ) ) ;
#40077 = CARTESIAN_POINT ( 'NONE',  ( 0.000000000000000000, 3.346456692913386100, 0.000000000000000000 ) ) ;
#40078 = LINE ( 'NONE', #12201, #39278 ) ;
#40079 = EDGE_CURVE ( 'NONE', #31299, #48104, #26316, .T. ) ;
#40080 = ORIENTED_EDGE ( 'NONE', *, *, #35696, .F. ) ;
#40081 = ADVANCED_FACE ( 'NONE', ( #30951 ), #13868, .T. ) ;
#40082 = DIRECTION ( 'NONE',  ( 0.9005016466594217839, 0.000000000000000000, -0.4348526007323282871 ) ) ;
#40083 = DIRECTION ( 'NONE',  ( 1.734723475976806848E-16, -0.000000000000000000, 1.000000000000000000 ) ) ;
#40084 = CARTESIAN_POINT ( 'NONE',  ( 0.000000000000000000, 0.000000000000000000, 0.000000000000000000 ) ) ;
#40085 = VECTOR ( 'NONE', #13257, 39.37007874015748143 ) ;
#40086 = ORIENTED_EDGE ( 'NONE', *, *, #9406, .T. ) ;
#40087 = PLANE ( 'NONE',  #26555 ) ;
#40088 = LINE ( 'NONE', #48298, #47453 ) ;
#40089 = CIRCLE ( 'NONE', #6302, 1.850107469027523432 ) ;
#40090 = ORIENTED_EDGE ( 'NONE', *, *, #28302, .T. ) ;
#40091 = CONICAL_SURFACE ( 'NONE', #46651, 3.483074324928249421, 1.244861948955335196 ) ;
#40092 = EDGE_CURVE ( 'NONE', #48279, #46197, #35890, .T. ) ;
#40093 = CARTESIAN_POINT ( 'NONE',  ( 2.951990591674675368, 5.118110236220475784, -0.08331184815398323673 ) ) ;
#40094 = ORIENTED_EDGE ( 'NONE', *, *, #18103, .T. ) ;
#40095 = ORIENTED_EDGE ( 'NONE', *, *, #31170, .F. ) ;
#40096 = LINE ( 'NONE', #44211, #44391 ) ;
#40097 =( NAMED_UNIT ( * ) PLANE_ANGLE_UNIT ( ) SI_UNIT ( $, .RADIAN. ) );
#40098 = EDGE_CURVE ( 'NONE', #16054, #46917, #11328, .T. ) ;
#40099 = VECTOR ( 'NONE', #13546, 39.37007874015748143 ) ;
#40100 = LINE ( 'NONE', #47798, #37970 ) ;
#40101 = VECTOR ( 'NONE', #39578, 39.37007874015748143 ) ;
#40102 = FACE_OUTER_BOUND ( 'NONE', #44128, .T. ) ;
#40103 = CARTESIAN_POINT ( 'NONE',  ( 2.823445274216730638, 1.664781993127344872, 0.8656477926280681245 ) ) ;
#40104 = VERTEX_POINT ( 'NONE', #39454 ) ;
#40105 = EDGE_LOOP ( 'NONE', ( #17133, #20395, #26398, #38237 ) ) ;
#40106 = AXIS2_PLACEMENT_3D ( 'NONE', #31633, #38623, #19492 ) ;
#40107 = CARTESIAN_POINT ( 'NONE',  ( -1.536664496436148184E-16, 0.000000000000000000, -0.8267716535433052849 ) ) ;
#40108 = PRODUCT ( 'Rotor', 'Rotor', '', ( #40029 ) ) ;
#40109 = ORIENTED_EDGE ( 'NONE', *, *, #43479, .T. ) ;
#40110 = PLANE ( 'NONE',  #27728 ) ;
#40111 = CARTESIAN_POINT ( 'NONE',  ( -1.732283464566932052, 3.346456692913386100, -1.299212598425193210 ) ) ;
#40112 = B_SPLINE_CURVE_WITH_KNOTS ( 'NONE', 3,
 ( #108, #19472, #16640, #23864 ),
 .UNSPECIFIED., .F., .F.,
 ( 4, 4 ),
 ( 2.271941954864058199E-07, 0.002500388579452512972 ),
 .UNSPECIFIED. ) ;
#40113 = CARTESIAN_POINT ( 'NONE',  ( -1.536664496436148184E-16, 0.000000000000000000, -1.456692913385822630 ) ) ;
#40114 = PLANE ( 'NONE',  #21111 ) ;
#40115 = DIRECTION ( 'NONE',  ( 1.000000000000000000, -0.000000000000000000, 0.000000000000000000 ) ) ;
#40116 = ORIENTED_EDGE ( 'NONE', *, *, #8777, .T. ) ;
#40117 = DIRECTION ( 'NONE',  ( 0.000000000000000000, -1.000000000000000000, 0.000000000000000000 ) ) ;
#40118 = PLANE ( 'NONE',  #43824 ) ;
#40119 = ORIENTED_EDGE ( 'NONE', *, *, #7719, .T. ) ;
#40120 = CYLINDRICAL_SURFACE ( 'NONE', #6750, 2.164630168518208109 ) ;
#40121 = LINE ( 'NONE', #4752, #43453 ) ;
#40122 = CARTESIAN_POINT ( 'NONE',  ( -0.07591351300297337346, 3.267716535433071279, 2.633779063002570064E-17 ) ) ;
#40123 = ORIENTED_EDGE ( 'NONE', *, *, #30176, .T. ) ;
#40124 = VECTOR ( 'NONE', #28553, 39.37007874015748143 ) ;
#40125 = CARTESIAN_POINT ( 'NONE',  ( -1.735196932040237394, 1.680109596358665636, 1.320828101803479315 ) ) ;
#40126 = CARTESIAN_POINT ( 'NONE',  ( -0.5455278134075214336, 0.000000000000000000, -8.878505979408855953E-16 ) ) ;
#40127 = LINE ( 'NONE', #27984, #46471 ) ;
#40128 = ADVANCED_FACE ( 'NONE', ( #47669 ), #39969, .F. ) ;
#40129 = AXIS2_PLACEMENT_3D ( 'NONE', #2262, #21884, #6396 ) ;
#40130 = EDGE_CURVE ( 'NONE', #1426, #41559, #19565, .T. ) ;
#40131 = VECTOR ( 'NONE', #15340, 39.37007874015748143 ) ;
#40132 = ORIENTED_EDGE ( 'NONE', *, *, #12990, .F. ) ;
#40133 = FACE_BOUND ( 'NONE', #3950, .T. ) ;
#40134 = DIRECTION ( 'NONE',  ( -0.000000000000000000, 0.000000000000000000, 1.000000000000000000 ) ) ;
#40135 = ORIENTED_EDGE ( 'NONE', *, *, #12138, .F. ) ;
#40136 = EDGE_CURVE ( 'NONE', #25127, #23961, #9437, .T. ) ;
#40137 = CARTESIAN_POINT ( 'NONE',  ( -1.181102362204724310, 0.000000000000000000, -1.062992125984252079 ) ) ;
#40138 = EDGE_CURVE ( 'NONE', #12457, #35559, #35584, .T. ) ;
#40139 = LINE ( 'NONE', #20759, #17733 ) ;
#40140 = CARTESIAN_POINT ( 'NONE',  ( 0.7423782071083091516, 3.346456692913386100, 1.692913385826762873 ) ) ;
#40141 = CARTESIAN_POINT ( 'NONE',  ( -0.8919566823238733733, 0.004617306369309737146, 1.588833855319179200 ) ) ;
#40142 = CIRCLE ( 'NONE', #12905, 2.106299212598425008 ) ;
#40143 = EDGE_CURVE ( 'NONE', #35414, #13810, #24826, .T. ) ;
#40144 = B_SPLINE_CURVE_WITH_KNOTS ( 'NONE', 3,
 ( #30520, #37515, #2641, #14772 ),
 .UNSPECIFIED., .F., .F.,
 ( 4, 4 ),
 ( 0.0005826651466654904138, 0.003082939193993071859 ),
 .UNSPECIFIED. ) ;
#40145 = VECTOR ( 'NONE', #24396, 39.37007874015748143 ) ;
#40146 = VERTEX_POINT ( 'NONE', #40936 ) ;
#40147 = EDGE_LOOP ( 'NONE', ( #10306, #17568, #40182, #23289 ) ) ;
#40148 = CARTESIAN_POINT ( 'NONE',  ( -2.793030215715272213, 1.573188339825353665, 0.9592557174602283077 ) ) ;
#40149 = LINE ( 'NONE', #20252, #1534 ) ;
#40150 = ORIENTED_EDGE ( 'NONE', *, *, #45364, .F. ) ;
#40151 = CARTESIAN_POINT ( 'NONE',  ( 1.695772546416037363, 1.745688802946234297, -2.417756147381349141 ) ) ;
#40152 = CARTESIAN_POINT ( 'NONE',  ( 1.833433833923351353, 0.000000000000000000, 0.6299212598425164567 ) ) ;
#40153 = CARTESIAN_POINT ( 'NONE',  ( 1.973323729629757217, 0.000000000000000000, -0.7899196136953162695 ) ) ;
#40154 = CARTESIAN_POINT ( 'NONE',  ( 2.100403847690402337, 3.346456692913386100, -0.1574803149606304187 ) ) ;
#40155 = VERTEX_POINT ( 'NONE', #31714 ) ;
#40156 = ORIENTED_EDGE ( 'NONE', *, *, #28097, .F. ) ;
#40157 = ADVANCED_FACE ( 'NONE', ( #35333 ), #27823, .F. ) ;
#40158 = CARTESIAN_POINT ( 'NONE',  ( -0.5455278134075214336, 3.346456692913386100, -0.5118110236220467790 ) ) ;
#40159 = CARTESIAN_POINT ( 'NONE',  ( 0.000000000000000000, 0.5070346321433212289, -0.9794755770252108196 ) ) ;
#40160 = DIRECTION ( 'NONE',  ( 1.734723475976806848E-16, -0.000000000000000000, 1.000000000000000000 ) ) ;
#40161 = CARTESIAN_POINT ( 'NONE',  ( 0.1155636338427008941, -0.5222242541845523167, 0.000000000000000000 ) ) ;
#40162 = FACE_BOUND ( 'NONE', #43038, .T. ) ;
#40163 = ORIENTED_EDGE ( 'NONE', *, *, #3900, .F. ) ;
#40164 = EDGE_CURVE ( 'NONE', #40553, #31330, #21315, .T. ) ;
#40165 = CARTESIAN_POINT ( 'NONE',  ( 1.062992125984252079, 0.4235180831842795257, -6.146657985744593474E-17 ) ) ;
#40166 = VERTEX_POINT ( 'NONE', #12090 ) ;
#40167 = ORIENTED_EDGE ( 'NONE', *, *, #32645, .F. ) ;
#40168 = PLANE ( 'NONE',  #23381 ) ;
#40169 = AXIS2_PLACEMENT_3D ( 'NONE', #24112, #44236, #12756 ) ;
#40170 = ORIENTED_EDGE ( 'NONE', *, *, #17752, .T. ) ;
#40171 = ORIENTED_EDGE ( 'NONE', *, *, #6278, .F. ) ;
#40172 = CARTESIAN_POINT ( 'NONE',  ( 0.000000000000000000, 0.000000000000000000, 0.000000000000000000 ) ) ;
#40173 = ORIENTED_EDGE ( 'NONE', *, *, #25425, .F. ) ;
#40174 = VECTOR ( 'NONE', #2711, 39.37007874015748143 ) ;
#40175 = PLANE ( 'NONE',  #13063 ) ;
#40176 = EDGE_CURVE ( 'NONE', #36441, #45968, #8188, .T. ) ;
#40177 = LINE ( 'NONE', #43254, #27693 ) ;
#40178 = LINE ( 'NONE', #4803, #34168 ) ;
#40179 = LINE ( 'NONE', #20286, #40470 ) ;
#40180 = CARTESIAN_POINT ( 'NONE',  ( 0.000000000000000000, 3.267716535433071279, 0.000000000000000000 ) ) ;
#40181 = DIRECTION ( 'NONE',  ( -0.000000000000000000, 1.000000000000000000, -0.000000000000000000 ) ) ;
#40182 = ORIENTED_EDGE ( 'NONE', *, *, #11607, .F. ) ;
#40183 = CARTESIAN_POINT ( 'NONE',  ( 0.2727639067037604392, 3.267716535433071279, -4.731699523581607892E-17 ) ) ;
#40184 = VECTOR ( 'NONE', #27837, 39.37007874015748143 ) ;
#40185 = CYLINDRICAL_SURFACE ( 'NONE', #18607, 2.164630168518208109 ) ;
#40186 = CARTESIAN_POINT ( 'NONE',  ( 1.940243258758003853, 1.049866565067838264, 0.5786780620529168306 ) ) ;
#40187 = ORIENTED_EDGE ( 'NONE', *, *, #15654, .F. ) ;
#40188 = CARTESIAN_POINT ( 'NONE',  ( -0.9302092402134559679, 3.267716535433071279, 1.889763779527550147 ) ) ;
#40189 = B_SPLINE_CURVE_WITH_KNOTS ( 'NONE', 3,
 ( #18820, #6946, #30693, #7203 ),
 .UNSPECIFIED., .F., .F.,
 ( 4, 4 ),
 ( 0.1211775127643062860, 0.1625894504277921315 ),
 .UNSPECIFIED. ) ;
#40190 = CARTESIAN_POINT ( 'NONE',  ( 1.228430781948798955, 1.636319860738493892, -2.437439334865536544 ) ) ;
#40191 = EDGE_LOOP ( 'NONE', ( #5627, #31601, #5657, #20771 ) ) ;
#40192 = FACE_OUTER_BOUND ( 'NONE', #19288, .T. ) ;
#40193 = FACE_OUTER_BOUND ( 'NONE', #30431, .T. ) ;
#40194 = LINE ( 'NONE', #36578, #20214 ) ;
#40195 = EDGE_CURVE ( 'NONE', #9022, #32849, #43568, .T. ) ;
#40196 = ORIENTED_EDGE ( 'NONE', *, *, #20263, .F. ) ;
#40197 = DIRECTION ( 'NONE',  ( -0.000000000000000000, 1.000000000000000000, -0.000000000000000000 ) ) ;
#40198 = B_SPLINE_CURVE_WITH_KNOTS ( 'NONE', 3,
 ( #29878, #25747, #37637, #45594 ),
 .UNSPECIFIED., .F., .F.,
 ( 4, 4 ),
 ( 0.0003817749841608031802, 0.002881981116852952267 ),
 .UNSPECIFIED. ) ;
#40199 = ORIENTED_EDGE ( 'NONE', *, *, #11608, .T. ) ;
#40200 = FACE_BOUND ( 'NONE', #6594, .T. ) ;
#40201 = EDGE_CURVE ( 'NONE', #2075, #33385, #8219, .T. ) ;
#40202 = DIRECTION ( 'NONE',  ( -0.000000000000000000, 1.000000000000000000, -0.000000000000000000 ) ) ;
#40203 = CARTESIAN_POINT ( 'NONE',  ( -0.8244711865321519006, 0.01471425056033665718, -1.598608591632243892 ) ) ;
#40205 = EDGE_CURVE ( 'NONE', #45614, #39943, #23960, .T. ) ;
#40204 = CARTESIAN_POINT ( 'NONE',  ( 0.000000000000000000, 3.267716535433071279, -1.161035397307311917E-15 ) ) ;
#40206 = VECTOR ( 'NONE', #25105, 39.37007874015748143 ) ;
#40207 = EDGE_CURVE ( 'NONE', #12462, #35716, #467, .T. ) ;
#40208 = ORIENTED_EDGE ( 'NONE', *, *, #22092, .T. ) ;
#40209 = VERTEX_POINT ( 'NONE', #16221 ) ;
#40210 = LINE ( 'NONE', #31955, #48475 ) ;
#40211 = ORIENTED_EDGE ( 'NONE', *, *, #16987, .F. ) ;
#40212 = CARTESIAN_POINT ( 'NONE',  ( -0.6982598466389058345, 0.000000000000000000, 1.720449438420079691 ) ) ;
#40213 = EDGE_LOOP ( 'NONE', ( #26011, #36168, #10441, #39406 ) ) ;
#40214 = CARTESIAN_POINT ( 'NONE',  ( 1.015142113812069757, 3.267716535433071279, -3.521981712565033375E-16 ) ) ;
#40215 = EDGE_CURVE ( 'NONE', #31646, #31327, #32229, .T. ) ;
#40216 = ORIENTED_EDGE ( 'NONE', *, *, #29873, .F. ) ;
#40217 = DIRECTION ( 'NONE',  ( 0.000000000000000000, 0.000000000000000000, -1.000000000000000000 ) ) ;
#40218 = DIRECTION ( 'NONE',  ( -1.000000000000000000, 0.000000000000000000, 1.734723475976806848E-16 ) ) ;
#40219 = ORIENTED_EDGE ( 'NONE', *, *, #33464, .T. ) ;
#40220 = EDGE_CURVE ( 'NONE', #45649, #39707, #27825, .T. ) ;
#40221 = DIRECTION ( 'NONE',  ( -1.000000000000000000, 0.000000000000000000, 0.000000000000000000 ) ) ;
#40222 = ORIENTED_EDGE ( 'NONE', *, *, #12739, .T. ) ;
#40223 = VECTOR ( 'NONE', #9705, 39.37007874015748143 ) ;
#40224 = DIRECTION ( 'NONE',  ( 1.000000000000000000, -0.000000000000000000, 0.000000000000000000 ) ) ;
#40225 = EDGE_CURVE ( 'NONE', #9041, #22692, #33199, .T. ) ;
#40226 = ORIENTED_EDGE ( 'NONE', *, *, #14860, .T. ) ;
#40227 = VERTEX_POINT ( 'NONE', #3838 ) ;
#40228 = CARTESIAN_POINT ( 'NONE',  ( -0.5455278134075214336, 3.346456692913386100, -0.3149606299212593941 ) ) ;
#40229 = ORIENTED_EDGE ( 'NONE', *, *, #27388, .T. ) ;
#40230 = CARTESIAN_POINT ( 'NONE',  ( 2.875073879018141376, 1.764051760264652824, -0.6730428845924211201 ) ) ;
#40231 = EDGE_CURVE ( 'NONE', #28846, #43954, #26566, .T. ) ;
#40232 = ORIENTED_EDGE ( 'NONE', *, *, #30471, .T. ) ;
#40233 = CARTESIAN_POINT ( 'NONE',  ( -0.8067290215918264673, 1.574803149606302854, 2.009464521518170343 ) ) ;
#40234 = LINE ( 'NONE', #4862, #17618 ) ;
#40235 = AXIS2_PLACEMENT_3D ( 'NONE', #887, #48088, #37288 ) ;
#40236 = VECTOR ( 'NONE', #39995, 39.37007874015748143 ) ;
#40237 = CARTESIAN_POINT ( 'NONE',  ( -0.07591351300297277671, 3.267716535433071279, 1.102362204724404160 ) ) ;
#40238 = ORIENTED_EDGE ( 'NONE', *, *, #4967, .T. ) ;
#40239 = CARTESIAN_POINT ( 'NONE',  ( -1.478009596860490715, 1.585803725363800210, 1.616919955472289727 ) ) ;
#40240 = CARTESIAN_POINT ( 'NONE',  ( 1.952332965905436701, 0.01912591429768871476, 0.6860966224282102344 ) ) ;
#40241 = FACE_OUTER_BOUND ( 'NONE', #8304, .T. ) ;
#40242 = CARTESIAN_POINT ( 'NONE',  ( 0.5455278134075213226, 3.267716535433071279, -9.463399047163224412E-17 ) ) ;
#40243 = ADVANCED_FACE ( 'NONE', ( #38706 ), #18799, .T. ) ;
#40244 = AXIS2_PLACEMENT_3D ( 'NONE', #2819, #42058, #11321 ) ;
#40245 = PLANE ( 'NONE',  #44126 ) ;
#40246 = EDGE_CURVE ( 'NONE', #24535, #36108, #35336, .T. ) ;
#40247 = CARTESIAN_POINT ( 'NONE',  ( -1.166969139818016199, 0.000000000000000000, -0.9842519685039344823 ) ) ;
#40248 = VECTOR ( 'NONE', #40005, 39.37007874015748143 ) ;
#40249 = LINE ( 'NONE', #4875, #36706 ) ;
#40250 = ORIENTED_EDGE ( 'NONE', *, *, #48564, .T. ) ;
#40251 = CARTESIAN_POINT ( 'NONE',  ( -0.8942052331142552601, 0.000000000000000000, 1.889763779527550147 ) ) ;
#40252 = VECTOR ( 'NONE', #29687, 39.37007874015748143 ) ;
#40253 = ORIENTED_EDGE ( 'NONE', *, *, #28798, .T. ) ;
#40254 = CARTESIAN_POINT ( 'NONE',  ( 1.068402561569974818, 6.692913385826772199, -1.884154513482173776 ) ) ;
#40255 = VECTOR ( 'NONE', #50584, 39.37007874015748143 ) ;
#40256 = ORIENTED_EDGE ( 'NONE', *, *, #43992, .T. ) ;
#40257 = EDGE_CURVE ( 'NONE', #528, #9706, #3249, .T. ) ;
#40258 = CARTESIAN_POINT ( 'NONE',  ( 0.000000000000000000, 0.000000000000000000, 0.000000000000000000 ) ) ;
#40259 = CARTESIAN_POINT ( 'NONE',  ( 1.566178811999271892, 1.641618931010494498, -2.239385674323774555 ) ) ;
#40260 = DIRECTION ( 'NONE',  ( 0.000000000000000000, 0.000000000000000000, -1.000000000000000000 ) ) ;
#40261 = CARTESIAN_POINT ( 'NONE',  ( 2.889674983507178219, 1.448941827424379936, -0.6090712660037606030 ) ) ;
#40262 = ORIENTED_EDGE ( 'NONE', *, *, #17394, .F. ) ;
#40263 = EDGE_CURVE ( 'NONE', #38696, #8095, #7707, .T. ) ;
#40264 = DIRECTION ( 'NONE',  ( -0.000000000000000000, 1.000000000000000000, -0.000000000000000000 ) ) ;
#40265 = FACE_BOUND ( 'NONE', #20248, .T. ) ;
#40266 = VERTEX_POINT ( 'NONE', #34825 ) ;
#40267 = FACE_OUTER_BOUND ( 'NONE', #21454, .T. ) ;
#40268 = ORIENTED_EDGE ( 'NONE', *, *, #25184, .F. ) ;
#40269 = DIRECTION ( 'NONE',  ( -0.9909497617679331460, 0.000000000000000000, -0.1342332658176667026 ) ) ;
#40270 = DIRECTION ( 'NONE',  ( -0.000000000000000000, 1.000000000000000000, -0.000000000000000000 ) ) ;
#40271 = AXIS2_PLACEMENT_3D ( 'NONE', #32209, #27802, #43548 ) ;
#40272 = CARTESIAN_POINT ( 'NONE',  ( -2.150518151785907772, 1.673457466938482296, -0.2530435858860717313 ) ) ;
#40273 = ORIENTED_EDGE ( 'NONE', *, *, #49425, .T. ) ;
#40274 = ORIENTED_EDGE ( 'NONE', *, *, #33757, .T. ) ;
#40275 = DIRECTION ( 'NONE',  ( -1.000000000000000000, 0.000000000000000000, -0.000000000000000000 ) ) ;
#40276 = DIRECTION ( 'NONE',  ( 1.283101021437938170E-16, 1.000000000000000000, 1.154811821032258155E-17 ) ) ;
#40277 = DIRECTION ( 'NONE',  ( 3.197442310920450836E-14, 0.000000000000000000, 1.000000000000000000 ) ) ;
#40278 = VECTOR ( 'NONE', #35460, 39.37007874015748143 ) ;
#40279 = VECTOR ( 'NONE', #24403, 39.37007874015748143 ) ;
#40280 = CIRCLE ( 'NONE', #5676, 2.165354330708661568 ) ;
#40281 = CARTESIAN_POINT ( 'NONE',  ( -0.8182917201112814842, 0.000000000000000000, 1.417322834645662777 ) ) ;
#40282 = DIRECTION ( 'NONE',  ( 1.000000000000000000, 0.000000000000000000, 0.000000000000000000 ) ) ;
#40283 = EDGE_CURVE ( 'NONE', #38696, #28900, #22953, .T. ) ;
#40284 = EDGE_LOOP ( 'NONE', ( #25591, #47722, #50077, #32083 ) ) ;
#40285 = AXIS2_PLACEMENT_3D ( 'NONE', #23647, #42246, #11016 ) ;
#40286 = LINE ( 'NONE', #20131, #24943 ) ;
#40287 = VERTEX_POINT ( 'NONE', #4098 ) ;
#40288 = ORIENTED_EDGE ( 'NONE', *, *, #3987, .F. ) ;
#40289 = VECTOR ( 'NONE', #18476, 39.37007874015748143 ) ;
#40290 = EDGE_CURVE ( 'NONE', #24532, #11539, #49273, .T. ) ;
#40291 = VERTEX_POINT ( 'NONE', #208 ) ;
#40292 = CARTESIAN_POINT ( 'NONE',  ( -2.151809081513409438, 1.575012187087082127, 0.2418202932658340965 ) ) ;
#40293 = LINE ( 'NONE', #2072, #241 ) ;
#40294 = AXIS2_PLACEMENT_3D ( 'NONE', #42076, #3090, #37963 ) ;
#40295 = EDGE_CURVE ( 'NONE', #50819, #18042, #13016, .T. ) ;
#40296 = ADVANCED_FACE ( 'NONE', ( #31716 ), #15705, .F. ) ;
#40297 = CARTESIAN_POINT ( 'NONE',  ( -0.3486774197067339376, 0.000000000000000000, -1.574803149606293529 ) ) ;
#40298 = DIRECTION ( 'NONE',  ( -0.000000000000000000, -1.000000000000000000, -0.000000000000000000 ) ) ;
#40299 = ORIENTED_EDGE ( 'NONE', *, *, #50499, .F. ) ;
#40300 = VERTEX_POINT ( 'NONE', #46910 ) ;
#40301 = CARTESIAN_POINT ( 'NONE',  ( 2.099568260077707027, 5.905511811023623991, -0.5296909464895783737 ) ) ;
#40302 = DIRECTION ( 'NONE',  ( -3.469446951953613696E-16, 0.000000000000000000, -1.000000000000000000 ) ) ;
#40303 = PLANE ( 'NONE',  #38160 ) ;
#40304 = CARTESIAN_POINT ( 'NONE',  ( 1.091055626815043311, 0.000000000000000000, 1.377952755905504256 ) ) ;
#40305 = CARTESIAN_POINT ( 'NONE',  ( 1.015142113812069091, 3.346456692913386100, -1.614173228346451605 ) ) ;
#40306 = CARTESIAN_POINT ( 'NONE',  ( -0.5455278134075208785, 3.346456692913386100, 1.692913385826762873 ) ) ;
#40307 =( BOUNDED_CURVE ( )  B_SPLINE_CURVE ( 3, ( #28199, #16600, #32350, #48043 ),
 .UNSPECIFIED., .F., .F. ) 
 B_SPLINE_CURVE_WITH_KNOTS ( ( 4, 4 ),
 ( 5.042641131756091077, 5.093548817700087383 ),
 .UNSPECIFIED. ) 
 CURVE ( )  GEOMETRIC_REPRESENTATION_ITEM ( )  RATIONAL_B_SPLINE_CURVE ( ( 1.000000000000000000, 0.9997840456193998193, 0.9997840456193998193, 1.000000000000000000 ) ) 
 REPRESENTATION_ITEM ( '' )  );
#40308 = CONICAL_SURFACE ( 'NONE', #32054, 2.422428857167389982, 0.4363323129985800519 ) ;
#40309 = EDGE_CURVE ( 'NONE', #35147, #16704, #30954, .T. ) ;
#40310 = PLANE ( 'NONE',  #17660 ) ;
#40311 = LINE ( 'NONE', #6657, #29398 ) ;
#40312 = EDGE_LOOP ( 'NONE', ( #10288, #9024, #40741, #29671 ) ) ;
#40313 = CARTESIAN_POINT ( 'NONE',  ( -1.247273217833388514, 0.007942302252338809612, -1.260601835943744087 ) ) ;
#40314 = CARTESIAN_POINT ( 'NONE',  ( 0.2727639067037604392, 0.000000000000000000, -0.3543307086614173040 ) ) ;
#40315 = B_SPLINE_CURVE_WITH_KNOTS ( 'NONE', 3,
 ( #24039, #10271, #6406, #10777 ),
 .UNSPECIFIED., .F., .F.,
 ( 4, 4 ),
 ( 2.559138052676411348E-07, 0.01633353498065875237 ),
 .UNSPECIFIED. ) ;
#40316 = ORIENTED_EDGE ( 'NONE', *, *, #44150, .F. ) ;
#40318 = VERTEX_POINT ( 'NONE', #19821 ) ;
#40317 = EDGE_CURVE ( 'NONE', #15064, #40389, #42814, .T. ) ;
#40319 = VECTOR ( 'NONE', #18693, 39.37007874015748143 ) ;
#40321 = CARTESIAN_POINT ( 'NONE',  ( 1.928732080931637505, 3.346456692913386100, -0.9842519685039348154 ) ) ;
#40320 = AXIS2_PLACEMENT_3D ( 'NONE', #19292, #23943, #5021 ) ;
#40322 = PLANE ( 'NONE',  #14659 ) ;
#40323 = LINE ( 'NONE', #20681, #23032 ) ;
#40324 = VERTEX_POINT ( 'NONE', #3582 ) ;
#40325 = EDGE_CURVE ( 'NONE', #45901, #50834, #18828, .T. ) ;
#40326 = EDGE_CURVE ( 'NONE', #20192, #6756, #42569, .T. ) ;
#40327 = AXIS2_PLACEMENT_3D ( 'NONE', #35653, #46726, #27894 ) ;
#40328 = EDGE_LOOP ( 'NONE', ( #7140, #36397, #3053, #35675 ) ) ;
#40329 = CARTESIAN_POINT ( 'NONE',  ( -0.5455278134075214336, 0.000000000000000000, -0.9448818897637762948 ) ) ;
#40330 = ORIENTED_EDGE ( 'NONE', *, *, #45027, .F. ) ;
#40331 = AXIS2_PLACEMENT_3D ( 'NONE', #34912, #11419, #42892 ) ;
#40332 = CARTESIAN_POINT ( 'NONE',  ( 0.8668862056626265300, 0.04180443457634609727, -1.686684286392636789 ) ) ;
#40333 = ORIENTED_EDGE ( 'NONE', *, *, #5198, .F. ) ;
#40334 = DIRECTION ( 'NONE',  ( -0.000000000000000000, -1.000000000000000000, -0.000000000000000000 ) ) ;
#40335 = DIRECTION ( 'NONE',  ( -0.01601477604151182663, 0.9998717552508123996, -0.000000000000000000 ) ) ;
#40336 = CARTESIAN_POINT ( 'NONE',  ( -2.103998301714549157, 3.346456692913386100, -0.5118110236220464460 ) ) ;
#40337 = ORIENTED_EDGE ( 'NONE', *, *, #17507, .T. ) ;
#40338 = ORIENTED_EDGE ( 'NONE', *, *, #8332, .T. ) ;
#40339 = EDGE_LOOP ( 'NONE', ( #5354, #21840, #31751, #16189 ) ) ;
#40340 = CARTESIAN_POINT ( 'NONE',  ( -0.5455278134075214336, 0.000000000000000000, -1.574803149606293529 ) ) ;
#40341 = VERTEX_POINT ( 'NONE', #19315 ) ;
#40342 = ORIENTED_EDGE ( 'NONE', *, *, #7600, .F. ) ;
#40343 = CARTESIAN_POINT ( 'NONE',  ( -0.8004649005966125719, 0.000000000000000000, -1.548759025234861753 ) ) ;
#40344 = DIRECTION ( 'NONE',  ( 0.000000000000000000, -1.000000000000000000, 0.000000000000000000 ) ) ;
#40345 = DIRECTION ( 'NONE',  ( -0.000000000000000000, 1.000000000000000000, -0.000000000000000000 ) ) ;
#40346 = ORIENTED_EDGE ( 'NONE', *, *, #41814, .F. ) ;
#40347 = DIRECTION ( 'NONE',  ( -3.469446951953613696E-16, 0.000000000000000000, -1.000000000000000000 ) ) ;
#40348 = CARTESIAN_POINT ( 'NONE',  ( -1.091055626815042645, 3.346456692913386100, -0.8267716535433052849 ) ) ;
#40349 = DIRECTION ( 'NONE',  ( -0.000000000000000000, 1.000000000000000000, -0.000000000000000000 ) ) ;
#40350 = ORIENTED_EDGE ( 'NONE', *, *, #49477, .T. ) ;
#40351 = CARTESIAN_POINT ( 'NONE',  ( -0.3486774197067342151, 0.000000000000000000, -2.204724409448810540 ) ) ;
#40352 = DIRECTION ( 'NONE',  ( -3.469446951953613696E-16, 0.000000000000000000, -1.000000000000000000 ) ) ;
#40353 = DIRECTION ( 'NONE',  ( -1.000000000000000000, 0.000000000000000000, 1.734723475976806848E-16 ) ) ;
#40354 = ORIENTED_EDGE ( 'NONE', *, *, #16951, .F. ) ;
#40355 = VERTEX_POINT ( 'NONE', #3841 ) ;
#40356 = DIRECTION ( 'NONE',  ( 0.7818314824680221431, -7.240175090764046435E-17, 0.6234898018587431423 ) ) ;
#40357 = DIRECTION ( 'NONE',  ( 0.000000000000000000, 0.000000000000000000, 1.000000000000000000 ) ) ;
#40358 = VECTOR ( 'NONE', #48568, 39.37007874015748143 ) ;
#40359 = B_SPLINE_CURVE_WITH_KNOTS ( 'NONE', 3,
 ( #35042, #35295, #15667, #47117 ),
 .UNSPECIFIED., .F., .F.,
 ( 4, 4 ),
 ( 5.991603428212694306E-07, 0.0001408512246855418704 ),
 .UNSPECIFIED. ) ;
#40360 = DIRECTION ( 'NONE',  ( -3.986037398843765983E-20, -1.000000000000000000, -1.160734090543304660E-16 ) ) ;
#40361 = ADVANCED_FACE ( 'NONE', ( #15458 ), #31207, .F. ) ;
#40362 = ADVANCED_FACE ( 'NONE', ( #7962 ), #38458, .F. ) ;
#40363 = CARTESIAN_POINT ( 'NONE',  ( 2.867773316779195447, 5.905511811023623991, -0.7050287376751999124 ) ) ;
#40365 = VECTOR ( 'NONE', #37349, 39.37007874015748143 ) ;
#40364 = CARTESIAN_POINT ( 'NONE',  ( -0.2727639067037607723, 3.267716535433071279, -0.1574803149606301411 ) ) ;
#40366 = ORIENTED_EDGE ( 'NONE', *, *, #41023, .T. ) ;
#40368 = EDGE_CURVE ( 'NONE', #8660, #18633, #34579, .T. ) ;
#40367 = ORIENTED_EDGE ( 'NONE', *, *, #48372, .T. ) ;
#40369 = CARTESIAN_POINT ( 'NONE',  ( -1.556712866041157106, 5.905511811023623991, 2.509548638715848323 ) ) ;
#40370 = AXIS2_PLACEMENT_3D ( 'NONE', #10666, #38540, #50842 ) ;
#40371 = EDGE_LOOP ( 'NONE', ( #5599, #4976, #33546, #38242 ) ) ;
#40372 = PLANE ( 'NONE',  #34029 ) ;
#40373 = CARTESIAN_POINT ( 'NONE',  ( 1.028983995711348021, 0.000000000000000000, 1.754363299348386862 ) ) ;
#40374 = EDGE_CURVE ( 'NONE', #33705, #23434, #12599, .T. ) ;
#40375 = B_SPLINE_CURVE_WITH_KNOTS ( 'NONE', 3,
 ( #50035, #3094, #46180, #30968 ),
 .UNSPECIFIED., .F., .F.,
 ( 4, 4 ),
 ( 0.001414413680292015644, 0.004800578680812093990 ),
 .UNSPECIFIED. ) ;
#40376 = CARTESIAN_POINT ( 'NONE',  ( -0.8942052331142552601, 3.346456692913386100, 1.692913385826762873 ) ) ;
#40377 = CARTESIAN_POINT ( 'NONE',  ( 0.8182917201112819283, 3.346456692913386100, 0.4724409448818868706 ) ) ;
#40378 = CARTESIAN_POINT ( 'NONE',  ( -0.3486774197067334935, 3.346456692913386100, 0.7480314960629874665 ) ) ;
#40379 = ORIENTED_EDGE ( 'NONE', *, *, #17695, .F. ) ;
#40380 = PLANE ( 'NONE',  #35751 ) ;
#40381 = ADVANCED_FACE ( 'NONE', ( #20076 ), #8960, .T. ) ;
#40382 = DIRECTION ( 'NONE',  ( 0.000000000000000000, 0.000000000000000000, -1.000000000000000000 ) ) ;
#40383 = ORIENTED_EDGE ( 'NONE', *, *, #27177, .F. ) ;
#40384 = CARTESIAN_POINT ( 'NONE',  ( -0.5756566573089003658, 1.611847391933241669, 2.896516654582634853 ) ) ;
#40385 = EDGE_CURVE ( 'NONE', #25253, #8785, #39712, .T. ) ;
#40386 = CARTESIAN_POINT ( 'NONE',  ( -1.738921996492520661, 6.764728787913346618E-05, 0.1249482579781430736 ) ) ;
#40387 = LINE ( 'NONE', #20749, #17262 ) ;
#40388 = VECTOR ( 'NONE', #513, 39.37007874015748143 ) ;
#40389 = VERTEX_POINT ( 'NONE', #47671 ) ;
#40390 = DIRECTION ( 'NONE',  ( -3.469446951953613696E-16, 0.000000000000000000, -1.000000000000000000 ) ) ;
#40391 = DIRECTION ( 'NONE',  ( 1.734723475976806848E-16, 0.000000000000000000, 1.000000000000000000 ) ) ;
#40392 = ADVANCED_FACE ( 'NONE', ( #4599 ), #24481, .F. ) ;
#40393 = CARTESIAN_POINT ( 'NONE',  ( 0.000000000000000000, 3.267716535433071279, -1.771653543307081691 ) ) ;
#40394 = EDGE_CURVE ( 'NONE', #3256, #20489, #48184, .T. ) ;
#40395 = EDGE_LOOP ( 'NONE', ( #28201, #39059, #39155, #8468 ) ) ;
#40396 = CARTESIAN_POINT ( 'NONE',  ( -0.2727639067037602727, 0.000000000000000000, 0.9055118110236167750 ) ) ;
#40397 = DIRECTION ( 'NONE',  ( -0.000000000000000000, 1.000000000000000000, -0.000000000000000000 ) ) ;
#40398 = ORIENTED_EDGE ( 'NONE', *, *, #41409, .F. ) ;
#40399 = EDGE_CURVE ( 'NONE', #8450, #34440, #36972, .T. ) ;
#40400 = PLANE ( 'NONE',  #13853 ) ;
#40401 = VECTOR ( 'NONE', #22765, 39.37007874015748143 ) ;
#40402 = DIRECTION ( 'NONE',  ( 0.000000000000000000, 0.000000000000000000, -1.000000000000000000 ) ) ;
#40403 = FACE_OUTER_BOUND ( 'NONE', #24152, .T. ) ;
#40404 = CARTESIAN_POINT ( 'NONE',  ( 0.6418034415187964248, 0.01259213821865694249, 1.850136423892497994 ) ) ;
#40405 = ORIENTED_EDGE ( 'NONE', *, *, #15372, .F. ) ;
#40406 = ORIENTED_EDGE ( 'NONE', *, *, #35992, .F. ) ;
#40407 = CARTESIAN_POINT ( 'NONE',  ( 2.734482843737263025, 0.000000000000000000, -1.115254632218672937 ) ) ;
#40408 = DIRECTION ( 'NONE',  ( -0.000000000000000000, -1.000000000000000000, -0.000000000000000000 ) ) ;
#40409 = ORIENTED_EDGE ( 'NONE', *, *, #43364, .F. ) ;
#40410 = CARTESIAN_POINT ( 'NONE',  ( 1.565700802531847957, 1.740062672906616204, -2.238727750734997191 ) ) ;
#40411 = PLANE ( 'NONE',  #26846 ) ;
#40412 = VECTOR ( 'NONE', #21215, 39.37007874015748143 ) ;
#40413 = CARTESIAN_POINT ( 'NONE',  ( 0.9914495361338626633, 0.000000000000000000, 2.781765111341823360 ) ) ;
#40414 = CARTESIAN_POINT ( 'NONE',  ( 1.944213194762889119, 0.05905979794000976862, 0.2136995197171435157 ) ) ;
#40415 = ORIENTED_EDGE ( 'NONE', *, *, #11960, .F. ) ;
#40416 = ORIENTED_EDGE ( 'NONE', *, *, #43202, .T. ) ;
#40417 = CARTESIAN_POINT ( 'NONE',  ( -0.8942052331142547050, 3.346456692913386100, 1.574803149606291974 ) ) ;
#40418 = LINE ( 'NONE', #31639, #49665 ) ;
#40419 = CARTESIAN_POINT ( 'NONE',  ( 0.2727639067037604392, 0.000000000000000000, -1.299212598425193210 ) ) ;
#40420 = VERTEX_POINT ( 'NONE', #35841 ) ;
#40421 = DIRECTION ( 'NONE',  ( -1.267583980596137654E-16, 1.000000000000000000, -2.300325776299734791E-17 ) ) ;
#40422 = FACE_BOUND ( 'NONE', #37438, .T. ) ;
#40423 = ORIENTED_EDGE ( 'NONE', *, *, #40971, .F. ) ;
#40424 = DIRECTION ( 'NONE',  ( 0.000000000000000000, 1.000000000000000000, 0.000000000000000000 ) ) ;
#40425 = ORIENTED_EDGE ( 'NONE', *, *, #19206, .T. ) ;
#40426 = ORIENTED_EDGE ( 'NONE', *, *, #46266, .T. ) ;
#40427 = FACE_OUTER_BOUND ( 'NONE', #20908, .T. ) ;
#40428 = ORIENTED_EDGE ( 'NONE', *, *, #6024, .F. ) ;
#40429 = EDGE_LOOP ( 'NONE', ( #35576, #7551, #8228, #46478 ) ) ;
#40430 = LINE ( 'NONE', #407, #4677 ) ;
#40431 = ORIENTED_EDGE ( 'NONE', *, *, #44067, .T. ) ;
#40432 = EDGE_CURVE ( 'NONE', #5041, #6926, #24737, .T. ) ;
#40433 = EDGE_CURVE ( 'NONE', #65, #23861, #32492, .T. ) ;
#40434 = CARTESIAN_POINT ( 'NONE',  ( 1.636583440222563857, 0.000000000000000000, 0.6299212598425164567 ) ) ;
#40435 = LINE ( 'NONE', #928, #43345 ) ;
#40436 = EDGE_CURVE ( 'NONE', #22884, #30932, #21723, .T. ) ;
#40437 = FACE_OUTER_BOUND ( 'NONE', #22504, .T. ) ;
#40438 = VECTOR ( 'NONE', #22642, 39.37007874015748143 ) ;
#40439 = AXIS2_PLACEMENT_3D ( 'NONE', #11706, #8344, #24089 ) ;
#40440 = PLANE ( 'NONE',  #32214 ) ;
#40441 = CARTESIAN_POINT ( 'NONE',  ( 0.9836083787002616319, 5.905511811023623991, -1.929060376159698054 ) ) ;
#40442 = PLANE ( 'NONE',  #31967 ) ;
#40443 = EDGE_LOOP ( 'NONE', ( #36375, #5526, #6082, #42727, #7575 ) ) ;
#40444 = CARTESIAN_POINT ( 'NONE',  ( 0.4696143004045478797, 3.346456692913386100, 0.2755905511810994302 ) ) ;
#40445 = VECTOR ( 'NONE', #43352, 39.37007874015748143 ) ;
#40446 = CARTESIAN_POINT ( 'NONE',  ( -0.07591351300297277671, 3.267716535433071279, 1.732283464566921172 ) ) ;
#40447 = ORIENTED_EDGE ( 'NONE', *, *, #5742, .F. ) ;
#40448 = CARTESIAN_POINT ( 'NONE',  ( 1.560669927219590747, 3.346456692913386100, -0.4724409448818889246 ) ) ;
#40449 = EDGE_CURVE ( 'NONE', #2298, #28697, #21118, .T. ) ;
#40450 = DIRECTION ( 'NONE',  ( 0.000000000000000000, 0.000000000000000000, -1.000000000000000000 ) ) ;
#40451 = VERTEX_POINT ( 'NONE', #5107 ) ;
#40452 = DIRECTION ( 'NONE',  ( -0.000000000000000000, 0.000000000000000000, 1.000000000000000000 ) ) ;
#40453 = DIRECTION ( 'NONE',  ( 1.000000000000000000, 0.000000000000000000, -3.469446951953613696E-16 ) ) ;
#40454 = DIRECTION ( 'NONE',  ( 1.000000000000000000, 0.000000000000000000, 0.000000000000000000 ) ) ;
#40455 = EDGE_CURVE ( 'NONE', #38863, #32449, #28470, .T. ) ;
#40456 = EDGE_CURVE ( 'NONE', #25755, #26859, #48737, .T. ) ;
#40457 = VERTEX_POINT ( 'NONE', #470 ) ;
#40458 = CARTESIAN_POINT ( 'NONE',  ( -0.8182917201112814842, 0.000000000000000000, 0.4724409448818872592 ) ) ;
#40459 = ORIENTED_EDGE ( 'NONE', *, *, #35471, .T. ) ;
#40460 = FACE_BOUND ( 'NONE', #2002, .T. ) ;
#40461 = PLANE ( 'NONE',  #38302 ) ;
#40462 = DIRECTION ( 'NONE',  ( -0.5773502691896253980, 0.5773502691896246208, 0.5773502691896272854 ) ) ;
#40463 = LINE ( 'NONE', #21347, #14420 ) ;
#40464 = ORIENTED_EDGE ( 'NONE', *, *, #32360, .F. ) ;
#40465 = EDGE_LOOP ( 'NONE', ( #34083, #22937, #42924, #15944 ) ) ;
#40466 = CARTESIAN_POINT ( 'NONE',  ( -0.8182917201112819283, 3.346456692913386100, -1.614173228346451605 ) ) ;
#40467 = EDGE_LOOP ( 'NONE', ( #27171, #5337, #41297, #15434 ) ) ;
#40468 = CARTESIAN_POINT ( 'NONE',  ( -0.5455278134075208785, 3.267716535433071279, 1.377952755905504256 ) ) ;
#40469 = VERTEX_POINT ( 'NONE', #36615 ) ;
#40470 = VECTOR ( 'NONE', #8167, 39.37007874015748143 ) ;
#40471 = DIRECTION ( 'NONE',  ( -0.000000000000000000, 1.000000000000000000, -0.000000000000000000 ) ) ;
#40472 = VECTOR ( 'NONE', #13907, 39.37007874015748143 ) ;
#40473 = ORIENTED_EDGE ( 'NONE', *, *, #11799, .T. ) ;
#40474 = DIRECTION ( 'NONE',  ( 1.000000000000000000, 0.000000000000000000, 0.000000000000000000 ) ) ;
#40475 = DIRECTION ( 'NONE',  ( 0.9959742939952397345, 0.000000000000000000, -0.08963930890342654279 ) ) ;
#40476 = ORIENTED_EDGE ( 'NONE', *, *, #41594, .F. ) ;
#40477 = LINE ( 'NONE', #44330, #34790 ) ;
#40478 = EDGE_LOOP ( 'NONE', ( #3506, #8223, #39251, #19438 ) ) ;
#40479 = ORIENTED_EDGE ( 'NONE', *, *, #7554, .F. ) ;
#40480 = ORIENTED_EDGE ( 'NONE', *, *, #36928, .T. ) ;
#40481 = DIRECTION ( 'NONE',  ( -5.207613805427244364E-18, -1.000000000000000000, -1.159565308550900415E-16 ) ) ;
#40482 = EDGE_CURVE ( 'NONE', #29354, #47979, #31976, .T. ) ;
#40483 = ORIENTED_EDGE ( 'NONE', *, *, #10126, .F. ) ;
#40484 = CARTESIAN_POINT ( 'NONE',  ( 0.002207914879453961969, 6.692913385826772199, 0.04916304461325451958 ) ) ;
#40485 = ORIENTED_EDGE ( 'NONE', *, *, #1071, .T. ) ;
#40486 = DIRECTION ( 'NONE',  ( 0.000000000000000000, -1.000000000000000000, 0.000000000000000000 ) ) ;
#40487 = EDGE_CURVE ( 'NONE', #19354, #47308, #1236, .T. ) ;
#40488 = FACE_OUTER_BOUND ( 'NONE', #543, .T. ) ;
#40489 = EDGE_CURVE ( 'NONE', #43816, #26794, #44083, .T. ) ;
#40490 = DIRECTION ( 'NONE',  ( -1.000000000000000000, 0.000000000000000000, 0.000000000000000000 ) ) ;
#40491 = ORIENTED_EDGE ( 'NONE', *, *, #40394, .F. ) ;
#40492 = DIRECTION ( 'NONE',  ( 0.000000000000000000, 1.000000000000000000, 0.000000000000000000 ) ) ;
#40493 = LINE ( 'NONE', #17258, #44297 ) ;
#40494 = CARTESIAN_POINT ( 'NONE',  ( 2.481910067697468580, 1.652579973978634653, -0.5160015848849505149 ) ) ;
#40495 = DIRECTION ( 'NONE',  ( -0.000000000000000000, 1.000000000000000000, -0.000000000000000000 ) ) ;
#40496 = FACE_OUTER_BOUND ( 'NONE', #23052, .T. ) ;
#40497 = CARTESIAN_POINT ( 'NONE',  ( 0.4519983648154151656, 1.649524736702080441, 2.215103298928671638 ) ) ;
#40498 = AXIS2_PLACEMENT_3D ( 'NONE', #7975, #50523, #18596 ) ;
#40499 = AXIS2_PLACEMENT_3D ( 'NONE', #10501, #26244, #34509 ) ;
#40500 = CARTESIAN_POINT ( 'NONE',  ( 0.7423782071083087075, 0.000000000000000000, 0.6299212598425161236 ) ) ;
#40501 = ADVANCED_FACE ( 'NONE', ( #43572 ), #8222, .F. ) ;
#40502 = ORIENTED_EDGE ( 'NONE', *, *, #36203, .F. ) ;
#40503 = CARTESIAN_POINT ( 'NONE',  ( -0.7117868624172403180, 0.000000000000000000, -1.591464117667691580 ) ) ;
#40504 = CARTESIAN_POINT ( 'NONE',  ( -2.160407304981126764, 5.905511811023623991, -0.1462862061266901326 ) ) ;
#40505 = ORIENTED_EDGE ( 'NONE', *, *, #22691, .T. ) ;
#40506 = CARTESIAN_POINT ( 'NONE',  ( -0.8182917201112819283, 3.346456692913386100, -0.9842519685039342603 ) ) ;
#40507 = EDGE_CURVE ( 'NONE', #34452, #49288, #4859, .T. ) ;
#40508 = VECTOR ( 'NONE', #50067, 39.37007874015748143 ) ;
#40509 = ORIENTED_EDGE ( 'NONE', *, *, #43972, .F. ) ;
#40510 = LINE ( 'NONE', #17273, #5821 ) ;
#40511 = CARTESIAN_POINT ( 'NONE',  ( -1.693234526714950228, 0.000000000000000000, -0.4369479234249735167 ) ) ;
#40512 = VECTOR ( 'NONE', #11537, 39.37007874015748143 ) ;
#40513 = CARTESIAN_POINT ( 'NONE',  ( -1.979793062125317471, 1.589971192595758698, 2.191257344206539948 ) ) ;
#40514 = CARTESIAN_POINT ( 'NONE',  ( 1.091055626815042645, 3.267716535433071279, -1.892679809432644389E-16 ) ) ;
#40515 = CARTESIAN_POINT ( 'NONE',  ( 0.2156685157584260770, 1.510622172706404864, -2.945280361644574185 ) ) ;
#40516 = ORIENTED_EDGE ( 'NONE', *, *, #34288, .F. ) ;
#40517 = EDGE_CURVE ( 'NONE', #7509, #23296, #10584, .T. ) ;
#40518 = DIRECTION ( 'NONE',  ( 1.734723475976806848E-16, -0.000000000000000000, 1.000000000000000000 ) ) ;
#40519 = B_SPLINE_CURVE_WITH_KNOTS ( 'NONE', 3,
 ( #33494, #28571, #25219, #49181 ),
 .UNSPECIFIED., .F., .F.,
 ( 4, 4 ),
 ( 2.136451542541482466E-07, 0.002500479364714848496 ),
 .UNSPECIFIED. ) ;
#40520 = FACE_BOUND ( 'NONE', #31429, .T. ) ;
#40521 = ORIENTED_EDGE ( 'NONE', *, *, #19706, .T. ) ;
#40522 = CARTESIAN_POINT ( 'NONE',  ( -0.8241443283111672402, 1.596276574288824301, 2.055867440327626916 ) ) ;
#40523 = EDGE_CURVE ( 'NONE', #383, #31088, #42005, .T. ) ;
#40524 = ORIENTED_EDGE ( 'NONE', *, *, #29340, .T. ) ;
#40525 = DIRECTION ( 'NONE',  ( -0.000000000000000000, 1.000000000000000000, -0.000000000000000000 ) ) ;
#40526 = CARTESIAN_POINT ( 'NONE',  ( 0.000000000000000000, 3.346456692913386100, 0.000000000000000000 ) ) ;
#40527 = CARTESIAN_POINT ( 'NONE',  ( 0.1067246931122726866, 0.02962905676920215767, 0.000000000000000000 ) ) ;
#40528 = VERTEX_POINT ( 'NONE', #5873 ) ;
#40529 = VERTEX_POINT ( 'NONE', #41752 ) ;
#40530 = CARTESIAN_POINT ( 'NONE',  ( -2.996855935080999345, 5.118110236220475784, 0.1838511574193322229 ) ) ;
#40531 = CARTESIAN_POINT ( 'NONE',  ( 0.5455278134075211005, 0.000000000000000000, 0.4330708661417287386 ) ) ;
#40532 = FACE_BOUND ( 'NONE', #39379, .T. ) ;
#40533 = ORIENTED_EDGE ( 'NONE', *, *, #6457, .T. ) ;
#40534 = VECTOR ( 'NONE', #41266, 39.37007874015748143 ) ;
#40535 = AXIS2_PLACEMENT_3D ( 'NONE', #31386, #4268, #35767 ) ;
#40536 = CARTESIAN_POINT ( 'NONE',  ( -1.393175312147127531, 0.000000000000000000, 1.048074961516273218 ) ) ;
#40537 = DIRECTION ( 'NONE',  ( 0.6579387259397027066, -8.743779800425989470E-17, 0.7530714660036196273 ) ) ;
#40538 = ORIENTED_EDGE ( 'NONE', *, *, #30938, .F. ) ;
#40539 = CARTESIAN_POINT ( 'NONE',  ( 0.000000000000000000, 5.905511811023623991, 0.000000000000000000 ) ) ;
#40540 = VECTOR ( 'NONE', #45507, 39.37007874015748143 ) ;
#40541 = ORIENTED_EDGE ( 'NONE', *, *, #3933, .T. ) ;
#40542 = EDGE_LOOP ( 'NONE', ( #3847, #1097, #13211, #3452 ) ) ;
#40543 = VECTOR ( 'NONE', #2562, 39.37007874015748143 ) ;
#40544 = ORIENTED_EDGE ( 'NONE', *, *, #1171, .F. ) ;
#40545 = LINE ( 'NONE', #12925, #6167 ) ;
#40546 = EDGE_CURVE ( 'NONE', #32429, #47028, #49449, .T. ) ;
#40547 = VECTOR ( 'NONE', #27464, 39.37007874015748143 ) ;
#40548 = FACE_OUTER_BOUND ( 'NONE', #31355, .T. ) ;
#40549 = PLANE ( 'NONE',  #5303 ) ;
#40550 = EDGE_CURVE ( 'NONE', #42097, #17453, #21373, .T. ) ;
#40551 = CARTESIAN_POINT ( 'NONE',  ( 1.287906020515830585, 3.267716535433071279, 1.889763779527550369 ) ) ;
#40552 = ORIENTED_EDGE ( 'NONE', *, *, #35142, .T. ) ;
#40553 = VERTEX_POINT ( 'NONE', #45095 ) ;
#40554 = CARTESIAN_POINT ( 'NONE',  ( -0.04921259842519767197, 6.692913385826772199, -2.165433070866142007 ) ) ;
#40555 = FACE_OUTER_BOUND ( 'NONE', #35948, .T. ) ;
#40556 = CARTESIAN_POINT ( 'NONE',  ( -1.636583440222564301, 0.000000000000000000, -0.9448818897637762948 ) ) ;
#40557 = DIRECTION ( 'NONE',  ( 0.9195277725514489076, 0.000000000000000000, 0.3930250316539278810 ) ) ;
#40558 = FACE_OUTER_BOUND ( 'NONE', #43590, .T. ) ;
#40559 = DIRECTION ( 'NONE',  ( 1.000000000000000000, 0.000000000000000000, 0.000000000000000000 ) ) ;
#40560 = DIRECTION ( 'NONE',  ( -0.000000000000000000, 1.000000000000000000, -0.000000000000000000 ) ) ;
#40561 = ORIENTED_EDGE ( 'NONE', *, *, #42894, .F. ) ;
#40562 = LINE ( 'NONE', #5708, #35792 ) ;
#40563 = CARTESIAN_POINT ( 'NONE',  ( -1.712496953225537188, 3.346456692913386100, 0.1574803149606286423 ) ) ;
#40564 = VERTEX_POINT ( 'NONE', #49203 ) ;
#40565 = VECTOR ( 'NONE', #13770, 39.37007874015748143 ) ;
#40566 = ORIENTED_EDGE ( 'NONE', *, *, #9728, .F. ) ;
#40567 = DIRECTION ( 'NONE',  ( 0.000000000000000000, -1.000000000000000000, 0.000000000000000000 ) ) ;
#40568 = AXIS2_PLACEMENT_3D ( 'NONE', #23500, #31263, #2881 ) ;
#40569 = PLANE ( 'NONE',  #8047 ) ;
#40570 = EDGE_LOOP ( 'NONE', ( #4190, #39041, #25986, #4923 ) ) ;
#40571 = EDGE_CURVE ( 'NONE', #29332, #41869, #26256, .T. ) ;
#40572 = VECTOR ( 'NONE', #41541, 39.37007874015748143 ) ;
#40573 = ORIENTED_EDGE ( 'NONE', *, *, #17563, .T. ) ;
#40574 = FACE_OUTER_BOUND ( 'NONE', #44566, .T. ) ;
#40575 = AXIS2_PLACEMENT_3D ( 'NONE', #8916, #40424, #21050 ) ;
#40576 = ORIENTED_EDGE ( 'NONE', *, *, #22184, .T. ) ;
#40577 = ADVANCED_FACE ( 'NONE', ( #10005 ), #6645, .F. ) ;
#40578 = ORIENTED_EDGE ( 'NONE', *, *, #33087, .F. ) ;
#40579 = CIRCLE ( 'NONE', #20795, 2.246510896728926010 ) ;
#40580 = CARTESIAN_POINT ( 'NONE',  ( -0.8942052331142547050, 3.267716535433071279, 1.574803149606291974 ) ) ;
#40581 = DIRECTION ( 'NONE',  ( 1.734723475976806848E-16, -0.000000000000000000, 1.000000000000000000 ) ) ;
#40582 = ADVANCED_FACE ( 'NONE', ( #21880 ), #29627, .F. ) ;
#40583 = EDGE_CURVE ( 'NONE', #6769, #21621, #40198, .T. ) ;
#40584 = ORIENTED_EDGE ( 'NONE', *, *, #34666, .T. ) ;
#40585 = ORIENTED_EDGE ( 'NONE', *, *, #43348, .F. ) ;
#40586 = ORIENTED_EDGE ( 'NONE', *, *, #11731, .F. ) ;
#40587 = CYLINDRICAL_SURFACE ( 'NONE', #6557, 2.165354330708661568 ) ;
#40588 = ORIENTED_EDGE ( 'NONE', *, *, #32000, .T. ) ;
#40589 = ORIENTED_EDGE ( 'NONE', *, *, #4043, .T. ) ;
#40590 = EDGE_CURVE ( 'NONE', #24946, #10781, #37383, .T. ) ;
#40591 = CARTESIAN_POINT ( 'NONE',  ( 0.8182917201112817063, 3.346456692913386100, -2.047244094488181343 ) ) ;
#40592 = DIRECTION ( 'NONE',  ( 0.000000000000000000, 1.000000000000000000, 0.000000000000000000 ) ) ;
#40593 = DIRECTION ( 'NONE',  ( 0.000000000000000000, -1.000000000000000000, 0.000000000000000000 ) ) ;
#40594 = EDGE_CURVE ( 'NONE', #37232, #15892, #44843, .T. ) ;
#40595 = ORIENTED_EDGE ( 'NONE', *, *, #16404, .F. ) ;
#40596 = CARTESIAN_POINT ( 'NONE',  ( 0.7423782071083087075, 3.267716535433071279, 0.3149606299212576177 ) ) ;
#40597 = LINE ( 'NONE', #21231, #22544 ) ;
#40598 = LINE ( 'NONE', #44458, #49220 ) ;
#40599 = ORIENTED_EDGE ( 'NONE', *, *, #18621, .F. ) ;
#40600 = CARTESIAN_POINT ( 'NONE',  ( -2.659122809025360024, 1.575291203863115275, 0.4098647105644042110 ) ) ;
#40601 = LINE ( 'NONE', #20199, #31852 ) ;
#40602 = DIRECTION ( 'NONE',  ( 0.000000000000000000, 0.000000000000000000, -1.000000000000000000 ) ) ;
#40603 = ORIENTED_EDGE ( 'NONE', *, *, #50003, .F. ) ;
#40604 = ORIENTED_EDGE ( 'NONE', *, *, #18621, .T. ) ;
#40605 = CARTESIAN_POINT ( 'NONE',  ( 0.5286458662987449930, 5.905511811023623991, 2.100489422084715674 ) ) ;
#40606 =( CONVERSION_BASED_UNIT ( 'INCH', #24088 ) LENGTH_UNIT ( ) NAMED_UNIT ( #36715 ) );
#40607 = EDGE_CURVE ( 'NONE', #7571, #43175, #22390, .T. ) ;
#40609 = VECTOR ( 'NONE', #36927, 39.37007874015748143 ) ;
#40608 = DIRECTION ( 'NONE',  ( -3.986037398843765983E-20, -1.000000000000000000, -1.160734090543304660E-16 ) ) ;
#40610 = DIRECTION ( 'NONE',  ( 0.5773502691896245098, 0.5773502691896259531, -0.5773502691896270633 ) ) ;
#40611 = EDGE_CURVE ( 'NONE', #35864, #43265, #22137, .T. ) ;
#40612 = LINE ( 'NONE', #17120, #40358 ) ;
#40613 = ORIENTED_EDGE ( 'NONE', *, *, #48650, .F. ) ;
#40614 = VERTEX_POINT ( 'NONE', #21622 ) ;
#40615 = VECTOR ( 'NONE', #33756, 39.37007874015748854 ) ;
#40616 = EDGE_CURVE ( 'NONE', #40227, #5560, #18517, .T. ) ;
#40617 = LINE ( 'NONE', #17123, #50564 ) ;
#40618 = AXIS2_PLACEMENT_3D ( 'NONE', #41873, #9619, #6512 ) ;
#40619 = VERTEX_POINT ( 'NONE', #33255 ) ;
#40620 = DIRECTION ( 'NONE',  ( -0.000000000000000000, 1.000000000000000000, 0.000000000000000000 ) ) ;
#40621 = LINE ( 'NONE', #1371, #44864 ) ;
#40622 = CONICAL_SURFACE ( 'NONE', #14224, 2.246510896728926010, 0.01601546068027819014 ) ;
#40623 = DIRECTION ( 'NONE',  ( -1.000000000000000000, 0.000000000000000000, 0.000000000000000000 ) ) ;
#40624 = DIRECTION ( 'NONE',  ( 0.000000000000000000, 0.000000000000000000, -1.000000000000000000 ) ) ;
#40625 = CARTESIAN_POINT ( 'NONE',  ( -0.5455278134075214336, 3.267716535433071279, -0.9448818897637762948 ) ) ;
#40626 = VERTEX_POINT ( 'NONE', #9497 ) ;
#40627 = CARTESIAN_POINT ( 'NONE',  ( -0.07591351300297327631, 3.267716535433071279, 2.633779063002566366E-17 ) ) ;
#40628 = DIRECTION ( 'NONE',  ( -1.000000000000000000, -0.000000000000000000, -0.000000000000000000 ) ) ;
#40629 = VERTEX_POINT ( 'NONE', #48940 ) ;
#40630 = CARTESIAN_POINT ( 'NONE',  ( 1.287906020515830585, 0.000000000000000000, 1.889763779527550369 ) ) ;
#40631 = CARTESIAN_POINT ( 'NONE',  ( 2.457479397754350536, 1.750633465154818991, -0.6113818280758235302 ) ) ;
#40632 = CARTESIAN_POINT ( 'NONE',  ( 0.1968503937007873017, 3.346456692913386100, -1.574803149606293529 ) ) ;
#40633 = ORIENTED_EDGE ( 'NONE', *, *, #3625, .F. ) ;
#40634 = EDGE_CURVE ( 'NONE', #27835, #37100, #2517, .T. ) ;
#40635 = CARTESIAN_POINT ( 'NONE',  ( -0.2878729405423523513, 0.5249316475426858419, 1.861923633677847079 ) ) ;
#40636 = LINE ( 'NONE', #5010, #34975 ) ;
#40637 = ORIENTED_EDGE ( 'NONE', *, *, #39902, .T. ) ;
#40638 = CARTESIAN_POINT ( 'NONE',  ( 1.930898218216747120, 1.205361022782829114E-17, -0.8788249315385436855 ) ) ;
#40639 = CARTESIAN_POINT ( 'NONE',  ( 0.2156685157584260770, 1.624173731825095723, -2.945280361644574185 ) ) ;
#40640 = VERTEX_POINT ( 'NONE', #13626 ) ;
#40641 = DIRECTION ( 'NONE',  ( 0.000000000000000000, -1.000000000000000000, 0.000000000000000000 ) ) ;
#40642 = LINE ( 'NONE', #5783, #17762 ) ;
#40643 = DIRECTION ( 'NONE',  ( -1.000000000000000000, 0.000000000000000000, -0.000000000000000000 ) ) ;
#40644 = DIRECTION ( 'NONE',  ( 1.687538997430237941E-14, 0.000000000000000000, 1.000000000000000000 ) ) ;
#40645 = ADVANCED_FACE ( 'NONE', ( #17749 ), #25491, .T. ) ;
#40646 = EDGE_CURVE ( 'NONE', #32098, #3695, #40999, .T. ) ;
#40647 = EDGE_CURVE ( 'NONE', #27463, #21275, #7400, .T. ) ;
#40648 = LINE ( 'NONE', #5273, #36230 ) ;
#40649 = CIRCLE ( 'NONE', #18384, 2.106299212598425008 ) ;
#40650 = ORIENTED_EDGE ( 'NONE', *, *, #37887, .F. ) ;
#40651 = ORIENTED_EDGE ( 'NONE', *, *, #9306, .T. ) ;
#40652 = DIRECTION ( 'NONE',  ( 1.000000000000000000, 0.000000000000000000, -3.469446951953613696E-16 ) ) ;
#40653 = DIRECTION ( 'NONE',  ( -0.000000000000000000, 1.000000000000000000, -0.000000000000000000 ) ) ;
#40654 = ORIENTED_EDGE ( 'NONE', *, *, #36178, .T. ) ;
#40655 = CARTESIAN_POINT ( 'NONE',  ( 1.636583440222563635, 0.000000000000000000, -0.9448818897637765168 ) ) ;
#40656 = LINE ( 'NONE', #20256, #44169 ) ;
#40657 = CARTESIAN_POINT ( 'NONE',  ( -1.195183497228115035E-16, 0.000000000000000000, -0.6299212598425177889 ) ) ;
#40658 = VECTOR ( 'NONE', #36164, 39.37007874015748143 ) ;
#40659 = DIRECTION ( 'NONE',  ( 0.000000000000000000, 1.000000000000000000, 0.000000000000000000 ) ) ;
#40660 = VECTOR ( 'NONE', #49278, 39.37007874015748143 ) ;
#40661 = ORIENTED_EDGE ( 'NONE', *, *, #41419, .F. ) ;
#40662 = ORIENTED_EDGE ( 'NONE', *, *, #19246, .F. ) ;
#40663 = DIRECTION ( 'NONE',  ( -3.469446951953613696E-16, 0.000000000000000000, -1.000000000000000000 ) ) ;
#40664 = CARTESIAN_POINT ( 'NONE',  ( 0.000000000000000000, 3.267716535433071279, 1.732283464566921172 ) ) ;
#40665 = CARTESIAN_POINT ( 'NONE',  ( 1.363819533518803695, 3.346456692913386100, 1.732283464566921172 ) ) ;
#40666 = VERTEX_POINT ( 'NONE', #39400 ) ;
#40667 = DIRECTION ( 'NONE',  ( 1.734723475976806848E-16, 0.000000000000000000, 1.000000000000000000 ) ) ;
#40668 = FACE_BOUND ( 'NONE', #18822, .T. ) ;
#40669 = VECTOR ( 'NONE', #36054, 39.37007874015748143 ) ;
#40670 = ORIENTED_EDGE ( 'NONE', *, *, #31937, .T. ) ;
#40671 = DIRECTION ( 'NONE',  ( 0.000000000000000000, 0.000000000000000000, 1.000000000000000000 ) ) ;
#40672 = ORIENTED_EDGE ( 'NONE', *, *, #8178, .F. ) ;
#40673 = VERTEX_POINT ( 'NONE', #30897 ) ;
#40674 = ADVANCED_FACE ( 'NONE', ( #38889 ), #27001, .F. ) ;
#40675 = DIRECTION ( 'NONE',  ( -1.000000000000000000, 0.000000000000000000, 1.734723475976806848E-16 ) ) ;
#40676 = ADVANCED_FACE ( 'NONE', ( #7900 ), #50203, .F. ) ;
#40677 = EDGE_LOOP ( 'NONE', ( #24923, #4591, #38707, #5588, #29116, #29153, #31490, #48897, #45680, #39579, #12379 ) ) ;
#40678 = DIRECTION ( 'NONE',  ( -0.000000000000000000, 1.000000000000000000, -0.000000000000000000 ) ) ;
#40679 = EDGE_CURVE ( 'NONE', #26214, #39217, #3021, .T. ) ;
#40680 = VERTEX_POINT ( 'NONE', #27509 ) ;
#40681 = EDGE_CURVE ( 'NONE', #13726, #21920, #50448, .T. ) ;
#40682 = DIRECTION ( 'NONE',  ( -1.000000000000000000, 0.000000000000000000, 0.000000000000000000 ) ) ;
#40683 = DIRECTION ( 'NONE',  ( -0.000000000000000000, -1.000000000000000000, -0.000000000000000000 ) ) ;
#40684 = CARTESIAN_POINT ( 'NONE',  ( 1.287906020515829919, 3.346456692913386100, -1.889763779527552368 ) ) ;
#40685 = CARTESIAN_POINT ( 'NONE',  ( -0.8182917201112819283, 0.000000000000000000, -0.3543307086614175816 ) ) ;
#40686 = B_SPLINE_CURVE_WITH_KNOTS ( 'NONE', 3,
 ( #8622, #361, #24372, #876 ),
 .UNSPECIFIED., .F., .F.,
 ( 4, 4 ),
 ( 2.075011172033926488E-07, 0.002500489681420431202 ),
 .UNSPECIFIED. ) ;
#40687 = CONICAL_SURFACE ( 'NONE', #18422, 2.165354330708661568, 0.2617993877991570129 ) ;
#40688 = PLANE ( 'NONE',  #20365 ) ;
#40689 = CARTESIAN_POINT ( 'NONE',  ( -4.268512490100411402E-16, 3.346456692913386100, -2.401574803149598480 ) ) ;
#40690 = ORIENTED_EDGE ( 'NONE', *, *, #20163, .F. ) ;
#40691 = DIRECTION ( 'NONE',  ( -3.469446951953613696E-16, 0.000000000000000000, -1.000000000000000000 ) ) ;
#40692 = VECTOR ( 'NONE', #29002, 39.37007874015748143 ) ;
#40693 = DIRECTION ( 'NONE',  ( -0.000000000000000000, 1.000000000000000000, -0.000000000000000000 ) ) ;
#40694 = VECTOR ( 'NONE', #26640, 39.37007874015748143 ) ;
#40695 = ORIENTED_EDGE ( 'NONE', *, *, #12907, .F. ) ;
#40696 = CARTESIAN_POINT ( 'NONE',  ( 2.298708793198899869, 5.118110236220475784, 1.181102362204724754 ) ) ;
#40697 = LINE ( 'NONE', #685, #36854 ) ;
#40698 = ORIENTED_EDGE ( 'NONE', *, *, #19749, .F. ) ;
#40699 = DIRECTION ( 'NONE',  ( 1.000000000000000000, 0.000000000000000000, -3.469446951953613696E-16 ) ) ;
#40700 = CARTESIAN_POINT ( 'NONE',  ( 1.834499544866850851, 1.737284818394516206, 1.400019292979238772 ) ) ;
#40701 = CARTESIAN_POINT ( 'NONE',  ( 2.112725606141798718, 1.676124320423267866, -0.9565416868427374375 ) ) ;
#40702 = VECTOR ( 'NONE', #25379, 39.37007874015748143 ) ;
#40703 = VERTEX_POINT ( 'NONE', #38391 ) ;
#40704 = DIRECTION ( 'NONE',  ( 1.000000000000000000, 0.000000000000000000, -3.469446951953613696E-16 ) ) ;
#40705 = B_SPLINE_CURVE_WITH_KNOTS ( 'NONE', 3,
 ( #20460, #40600, #20198, #8335 ),
 .UNSPECIFIED., .F., .F.,
 ( 4, 4 ),
 ( 6.908975551891818311E-06, 0.02000310376711551125 ),
 .UNSPECIFIED. ) ;
#40706 = ORIENTED_EDGE ( 'NONE', *, *, #5150, .T. ) ;
#40707 = FACE_BOUND ( 'NONE', #22680, .T. ) ;
#40708 = DIRECTION ( 'NONE',  ( 1.000000000000000000, 0.000000000000000000, 0.000000000000000000 ) ) ;
#40709 = DIRECTION ( 'NONE',  ( -0.000000000000000000, 1.000000000000000000, -0.000000000000000000 ) ) ;
#40710 = DIRECTION ( 'NONE',  ( 1.734723475976806848E-16, -0.000000000000000000, 1.000000000000000000 ) ) ;
#40711 = EDGE_CURVE ( 'NONE', #38291, #18200, #38645, .T. ) ;
#40712 = EDGE_LOOP ( 'NONE', ( #34835, #19, #13873 ) ) ;
#40713 = ORIENTED_EDGE ( 'NONE', *, *, #32437, .T. ) ;
#40714 = EDGE_CURVE ( 'NONE', #30930, #14507, #46354, .T. ) ;
#40715 = CARTESIAN_POINT ( 'NONE',  ( -1.091055626815042201, 0.000000000000000000, 0.3149606299212580063 ) ) ;
#40716 = EDGE_LOOP ( 'NONE', ( #5688, #29548, #46159, #27296 ) ) ;
#40717 = DIRECTION ( 'NONE',  ( -0.07365742419378766559, 0.000000000000000000, 0.9972836025229415702 ) ) ;
#40718 = ORIENTED_EDGE ( 'NONE', *, *, #38839, .T. ) ;
#40719 = EDGE_CURVE ( 'NONE', #50260, #35018, #14642, .T. ) ;
#40720 = CARTESIAN_POINT ( 'NONE',  ( -0.5455278134075214336, 0.000000000000000000, 2.204724409448808764 ) ) ;
#40721 = B_SPLINE_CURVE_WITH_KNOTS ( 'NONE', 3,
 ( #40638, #5777, #1393, #25146 ),
 .UNSPECIFIED., .F., .F.,
 ( 4, 4 ),
 ( 6.537091799742329783E-07, 0.004672429636363999335 ),
 .UNSPECIFIED. ) ;
#40722 = ORIENTED_EDGE ( 'NONE', *, *, #8781, .T. ) ;
#40723 = DIRECTION ( 'NONE',  ( -0.000000000000000000, 1.000000000000000000, -0.000000000000000000 ) ) ;
#40724 = CIRCLE ( 'NONE', #1129, 1.743387098533651480 ) ;
#40725 = LINE ( 'NONE', #20845, #47042 ) ;
#40726 = ORIENTED_EDGE ( 'NONE', *, *, #12221, .T. ) ;
#40727 = DIRECTION ( 'NONE',  ( -1.000000000000000000, 0.000000000000000000, 0.000000000000000000 ) ) ;
#40728 = VECTOR ( 'NONE', #39680, 39.37007874015748143 ) ;
#40729 = ORIENTED_EDGE ( 'NONE', *, *, #34640, .F. ) ;
#40730 = ORIENTED_EDGE ( 'NONE', *, *, #9303, .T. ) ;
#40731 = VECTOR ( 'NONE', #21777, 39.37007874015748143 ) ;
#40732 = VECTOR ( 'NONE', #40560, 39.37007874015748143 ) ;
#40733 = EDGE_CURVE ( 'NONE', #17198, #9822, #38277, .T. ) ;
#40734 = B_SPLINE_CURVE_WITH_KNOTS ( 'NONE', 3,
 ( #35493, #7614, #635, #35743 ),
 .UNSPECIFIED., .F., .F.,
 ( 4, 4 ),
 ( 0.01074804989555521069, 0.03073582135077717464 ),
 .UNSPECIFIED. ) ;
#40735 = ORIENTED_EDGE ( 'NONE', *, *, #22380, .F. ) ;
#40736 = ORIENTED_EDGE ( 'NONE', *, *, #22330, .T. ) ;
#40737 = LINE ( 'NONE', #41748, #48300 ) ;
#40738 = DIRECTION ( 'NONE',  ( 1.000000000000000000, 0.000000000000000000, 0.000000000000000000 ) ) ;
#40739 = AXIS2_PLACEMENT_3D ( 'NONE', #1576, #21455, #37209 ) ;
#40740 = ADVANCED_FACE ( 'NONE', ( #15143 ), #31400, .F. ) ;
#40741 = ORIENTED_EDGE ( 'NONE', *, *, #36343, .F. ) ;
#40742 = CARTESIAN_POINT ( 'NONE',  ( 1.091055626815042645, 3.346456692913386100, -0.1968503937007883287 ) ) ;
#40743 = ORIENTED_EDGE ( 'NONE', *, *, #36117, .F. ) ;
#40744 = DIRECTION ( 'NONE',  ( -0.000000000000000000, 1.000000000000000000, -0.000000000000000000 ) ) ;
#40745 = CARTESIAN_POINT ( 'NONE',  ( 1.909347346926324684, 3.267716535433071279, -0.1574803149606304187 ) ) ;
#40746 = ORIENTED_EDGE ( 'NONE', *, *, #29827, .F. ) ;
#40747 = CARTESIAN_POINT ( 'NONE',  ( 1.700185224778670401, 1.636708331897141377, -1.557456981387029149 ) ) ;
#40748 = PLANE ( 'NONE',  #37845 ) ;
#40749 = ORIENTED_EDGE ( 'NONE', *, *, #43139, .T. ) ;
#40750 = FACE_OUTER_BOUND ( 'NONE', #15766, .T. ) ;
#40751 = FACE_OUTER_BOUND ( 'NONE', #18191, .T. ) ;
#40752 = CARTESIAN_POINT ( 'NONE',  ( 1.726519710923990480, 1.205361022782829114E-17, -1.198633063221572481 ) ) ;
#40753 = DIRECTION ( 'NONE',  ( -0.000000000000000000, 1.000000000000000000, -0.000000000000000000 ) ) ;
#40754 = DIRECTION ( 'NONE',  ( 1.734723475976806848E-16, 0.000000000000000000, 1.000000000000000000 ) ) ;
#40755 = ORIENTED_EDGE ( 'NONE', *, *, #37095, .T. ) ;
#40756 = DIRECTION ( 'NONE',  ( 1.000000000000000000, 0.000000000000000000, 0.000000000000000000 ) ) ;
#40757 = DIRECTION ( 'NONE',  ( 1.734723475976806848E-16, -0.000000000000000000, 1.000000000000000000 ) ) ;
#40758 =( GEOMETRIC_REPRESENTATION_CONTEXT ( 3 ) GLOBAL_UNCERTAINTY_ASSIGNED_CONTEXT ( ( #5051 ) ) GLOBAL_UNIT_ASSIGNED_CONTEXT ( ( #13245, #44966, #29493 ) ) REPRESENTATION_CONTEXT ( 'NONE', 'WORKASPACE' ) );
#40759 = ORIENTED_EDGE ( 'NONE', *, *, #32936, .T. ) ;
#40760 = CARTESIAN_POINT ( 'NONE',  ( 0.8182917201112824834, 0.000000000000000000, 1.732283464566921172 ) ) ;
#40761 = VECTOR ( 'NONE', #25051, 39.37007874015748143 ) ;
#40762 = VECTOR ( 'NONE', #24864, 39.37007874015748143 ) ;
#40763 = ORIENTED_EDGE ( 'NONE', *, *, #29604, .T. ) ;
#40764 = CARTESIAN_POINT ( 'NONE',  ( 1.634516194504713527, 0.03557717711494950280, -1.137902073757964816 ) ) ;
#40765 = AXIS2_PLACEMENT_3D ( 'NONE', #8753, #24509, #40260 ) ;
#40767 = CIRCLE ( 'NONE', #47307, 0.3740157480314961203 ) ;
#40766 = DIRECTION ( 'NONE',  ( -0.000000000000000000, -1.000000000000000000, -0.000000000000000000 ) ) ;
#40768 = LINE ( 'NONE', #13148, #33647 ) ;
#40769 = DIRECTION ( 'NONE',  ( -1.000000000000000000, 0.000000000000000000, -0.000000000000000000 ) ) ;
#40770 = CARTESIAN_POINT ( 'NONE',  ( -2.151809081513409438, 1.575012187087082127, 0.2418202932658340965 ) ) ;
#40771 = ORIENTED_EDGE ( 'NONE', *, *, #10533, .F. ) ;
#40772 = CARTESIAN_POINT ( 'NONE',  ( -1.052882153134559129, 1.702845081222334578, 2.758709064543730438 ) ) ;
#40773 = EDGE_CURVE ( 'NONE', #35361, #11368, #50698, .T. ) ;
#40774 = AXIS2_PLACEMENT_3D ( 'NONE', #30857, #45366, #10028 ) ;
#40775 = CARTESIAN_POINT ( 'NONE',  ( 0.4696143004045484903, 0.000000000000000000, 1.102362204724404160 ) ) ;
#40776 = EDGE_CURVE ( 'NONE', #50201, #43816, #44397, .T. ) ;
#40777 = ORIENTED_EDGE ( 'NONE', *, *, #30938, .T. ) ;
#40778 = CARTESIAN_POINT ( 'NONE',  ( 1.368795924897367566, 1.049866565067838486, 1.491914849661855502 ) ) ;
#40779 = VERTEX_POINT ( 'NONE', #7647 ) ;
#40780 = EDGE_CURVE ( 'NONE', #20664, #1280, #6265, .T. ) ;
#40781 = CARTESIAN_POINT ( 'NONE',  ( 1.090138530625468283, -2.244369135793855756E-16, 1.920534397867776910 ) ) ;
#40782 = CARTESIAN_POINT ( 'NONE',  ( 2.793030215715258446, 1.762782749918499814, 0.9592557174602684977 ) ) ;
#40783 = LINE ( 'NONE', #5405, #13375 ) ;
#40784 = DIRECTION ( 'NONE',  ( -0.01601477604151182663, 0.9998717552508123996, -0.000000000000000000 ) ) ;
#40785 = ORIENTED_EDGE ( 'NONE', *, *, #28356, .F. ) ;
#40786 = ORIENTED_EDGE ( 'NONE', *, *, #23616, .F. ) ;
#40787 = PLANE ( 'NONE',  #6226 ) ;
#40788 = PLANE ( 'NONE',  #11671 ) ;
#40789 = FACE_BOUND ( 'NONE', #4211, .T. ) ;
#40790 = LINE ( 'NONE', #21173, #33655 ) ;
#40791 = EDGE_CURVE ( 'NONE', #6075, #46791, #14893, .T. ) ;
#40792 = CARTESIAN_POINT ( 'NONE',  ( -2.576863348864732117, 1.568913320674888201, 1.442554885838411849 ) ) ;
#40793 = EDGE_LOOP ( 'NONE', ( #11912, #50039, #8709, #4715 ) ) ;
#40794 = CARTESIAN_POINT ( 'NONE',  ( 0.002207914879453961969, 6.692913385826772199, 0.04916304461325451958 ) ) ;
#40795 = APPLICATION_CONTEXT ( 'automotive_design' ) ;
#40796 = VECTOR ( 'NONE', #43701, 39.37007874015748143 ) ;
#40797 = DIRECTION ( 'NONE',  ( -0.7071067811865481278, 0.7071067811865469066, -1.221861889385012670E-15 ) ) ;
#40798 = ADVANCED_FACE ( 'NONE', ( #30640 ), #49955, .F. ) ;
#40799 = ORIENTED_EDGE ( 'NONE', *, *, #16649, .F. ) ;
#40800 = AXIS2_PLACEMENT_3D ( 'NONE', #20671, #40042, #36432 ) ;
#40801 = ORIENTED_EDGE ( 'NONE', *, *, #430, .T. ) ;
#40802 = CIRCLE ( 'NONE', #18542, 2.443628662382284489 ) ;
#40803 = ORIENTED_EDGE ( 'NONE', *, *, #1568, .F. ) ;
#40804 = DIRECTION ( 'NONE',  ( -3.469446951953613696E-16, 0.000000000000000000, -1.000000000000000000 ) ) ;
#40805 = CARTESIAN_POINT ( 'NONE',  ( 0.3664524127070866721, -0.6299212598425202314, 0.07483588040983164824 ) ) ;
#40806 = PLANE ( 'NONE',  #48925 ) ;
#40807 = DIRECTION ( 'NONE',  ( -0.000000000000000000, 1.000000000000000000, -0.000000000000000000 ) ) ;
#40808 = EDGE_LOOP ( 'NONE', ( #35151, #30820, #498, #31548 ) ) ;
#40809 = ORIENTED_EDGE ( 'NONE', *, *, #39829, .F. ) ;
#40810 = VECTOR ( 'NONE', #4917, 39.37007874015748143 ) ;
#40811 = LINE ( 'NONE', #13441, #30737 ) ;
#40812 = DIRECTION ( 'NONE',  ( 0.2225209339563184452, 0.000000000000000000, -0.9749279121818227312 ) ) ;
#40813 = CARTESIAN_POINT ( 'NONE',  ( 0.000000000000000000, 3.267716535433071279, -1.771653543307081025 ) ) ;
#40814 = EDGE_CURVE ( 'NONE', #25289, #1960, #35025, .T. ) ;
#40815 = LINE ( 'NONE', #1050, #12792 ) ;
#40816 = DIRECTION ( 'NONE',  ( 1.000000000000000000, 0.000000000000000000, -3.469446951953613696E-16 ) ) ;
#40817 = DIRECTION ( 'NONE',  ( -1.000000000000000000, -0.000000000000000000, -0.000000000000000000 ) ) ;
#40818 = LINE ( 'NONE', #24553, #33339 ) ;
#40819 = VERTEX_POINT ( 'NONE', #23385 ) ;
#40820 = CARTESIAN_POINT ( 'NONE',  ( -1.166969139818015977, 3.346456692913386100, -1.823990790610291013 ) ) ;
#40821 = LINE ( 'NONE', #29191, #42551 ) ;
#40822 = EDGE_LOOP ( 'NONE', ( #233, #29606, #5228, #39254 ) ) ;
#40823 = ORIENTED_EDGE ( 'NONE', *, *, #13214, .T. ) ;
#40824 = CARTESIAN_POINT ( 'NONE',  ( 1.363819533518803251, 3.346456692913386100, -0.7874015748031473194 ) ) ;
#40825 = FACE_OUTER_BOUND ( 'NONE', #45698, .T. ) ;
#40826 = ORIENTED_EDGE ( 'NONE', *, *, #7528, .F. ) ;
#40827 = AXIS2_PLACEMENT_3D ( 'NONE', #23517, #35154, #27382 ) ;
#40828 = AXIS2_PLACEMENT_3D ( 'NONE', #19612, #20645, #24525 ) ;
#40829 = ORIENTED_EDGE ( 'NONE', *, *, #3465, .T. ) ;
#40830 = CIRCLE ( 'NONE', #16097, 1.850107469027523432 ) ;
#40831 = DIRECTION ( 'NONE',  ( -3.469446951953613696E-16, 0.000000000000000000, -1.000000000000000000 ) ) ;
#40832 = VECTOR ( 'NONE', #50359, 39.37007874015748143 ) ;
#40833 = VERTEX_POINT ( 'NONE', #12807 ) ;
#40834 = ADVANCED_FACE ( 'NONE', ( #28537 ), #24421, .F. ) ;
#40835 = CARTESIAN_POINT ( 'NONE',  ( -1.985260859929298016, 3.346456692913386100, -0.7037298423582233342 ) ) ;
#40836 = LINE ( 'NONE', #44441, #46157 ) ;
#40837 = ADVANCED_FACE ( 'NONE', ( #16160 ), #47617, .F. ) ;
#40838 = ADVANCED_FACE ( 'NONE', ( #12293 ), #40175, .T. ) ;
#40839 = EDGE_LOOP ( 'NONE', ( #28687, #34761, #43449, #32693 ) ) ;
#40840 = ORIENTED_EDGE ( 'NONE', *, *, #33150, .F. ) ;
#40841 = EDGE_LOOP ( 'NONE', ( #26460, #33016, #24326, #38790 ) ) ;
#40842 = VECTOR ( 'NONE', #49611, 39.37007874015748143 ) ;
#40843 = LINE ( 'NONE', #24328, #10640 ) ;
#40844 = EDGE_LOOP ( 'NONE', ( #12537, #19170, #16327, #31638 ) ) ;
#40845 = ORIENTED_EDGE ( 'NONE', *, *, #46976, .F. ) ;
#40846 = LINE ( 'NONE', #5473, #9175 ) ;
#40847 = CARTESIAN_POINT ( 'NONE',  ( 1.833433833923351353, 3.267716535433071279, -0.1968503937007886062 ) ) ;
#40848 = DIRECTION ( 'NONE',  ( -0.000000000000000000, -1.000000000000000000, -0.000000000000000000 ) ) ;
#40849 = VERTEX_POINT ( 'NONE', #27770 ) ;
#40850 = DIRECTION ( 'NONE',  ( 0.5877852522924684742, -9.392878985996986848E-17, 0.8090169943749506709 ) ) ;
#40851 = EDGE_CURVE ( 'NONE', #31303, #3180, #24930, .T. ) ;
#40852 = LINE ( 'NONE', #25605, #43123 ) ;
#40853 = LINE ( 'NONE', #17608, #2276 ) ;
#40854 = ORIENTED_EDGE ( 'NONE', *, *, #46193, .F. ) ;
#40855 = B_SPLINE_CURVE_WITH_KNOTS ( 'NONE', 3,
 ( #47987, #16797, #24796, #21182 ),
 .UNSPECIFIED., .F., .F.,
 ( 4, 4 ),
 ( 0.002222465192948955282, 0.004722220330562246909 ),
 .UNSPECIFIED. ) ;
#40856 = CARTESIAN_POINT ( 'NONE',  ( 0.1968503937007873017, 0.000000000000000000, -1.574803149606293529 ) ) ;
#40857 = CARTESIAN_POINT ( 'NONE',  ( 1.882988517681382756, 6.692913385826772199, 1.069164917025817951 ) ) ;
#40858 = DIRECTION ( 'NONE',  ( -3.986037398843765983E-20, -1.000000000000000000, -1.160734090543304660E-16 ) ) ;
#40859 = ORIENTED_EDGE ( 'NONE', *, *, #9243, .T. ) ;
#40860 = ORIENTED_EDGE ( 'NONE', *, *, #5183, .T. ) ;
#40861 = LINE ( 'NONE', #36739, #49444 ) ;
#40862 = ADVANCED_FACE ( 'NONE', ( #44533 ), #8420, .F. ) ;
#40863 = FACE_OUTER_BOUND ( 'NONE', #29775, .T. ) ;
#40864 = CARTESIAN_POINT ( 'NONE',  ( -0.2727639067037608278, 0.000000000000000000, -1.929133858267710000 ) ) ;
#40865 = VERTEX_POINT ( 'NONE', #44025 ) ;
#40866 = EDGE_LOOP ( 'NONE', ( #41589, #29949, #16829, #13952 ) ) ;
#40867 = VECTOR ( 'NONE', #8428, 39.37007874015748854 ) ;
#40868 = AXIS2_PLACEMENT_3D ( 'NONE', #30097, #11235, #26966 ) ;
#40869 = DIRECTION ( 'NONE',  ( -0.000000000000000000, 1.000000000000000000, -0.000000000000000000 ) ) ;
#40870 = ORIENTED_EDGE ( 'NONE', *, *, #32585, .T. ) ;
#40871 = LINE ( 'NONE', #41130, #47159 ) ;
#40872 = ADVANCED_FACE ( 'NONE', ( #4545 ), #927, .T. ) ;
#40873 = LINE ( 'NONE', #37772, #352 ) ;
#40874 = AXIS2_PLACEMENT_3D ( 'NONE', #21466, #20690, #17343 ) ;
#40875 = VECTOR ( 'NONE', #7075, 39.37007874015748143 ) ;
#40876 = FACE_OUTER_BOUND ( 'NONE', #3060, .T. ) ;
#40877 = CARTESIAN_POINT ( 'NONE',  ( 0.1968503937007869686, 0.000000000000000000, -2.401574803149598480 ) ) ;
#40878 = LINE ( 'NONE', #25888, #669 ) ;
#40879 = VECTOR ( 'NONE', #12700, 39.37007874015748143 ) ;
#40880 = ORIENTED_EDGE ( 'NONE', *, *, #46443, .T. ) ;
#40881 = CARTESIAN_POINT ( 'NONE',  ( 1.091055626815042423, 0.000000000000000000, -1.889763779527552368 ) ) ;
#40882 = EDGE_CURVE ( 'NONE', #13286, #36052, #20281, .T. ) ;
#40883 = CARTESIAN_POINT ( 'NONE',  ( 2.378961647330872342, 3.230577599468342775, 0.6299212598425161236 ) ) ;
#40884 = EDGE_CURVE ( 'NONE', #25226, #28296, #36045, .T. ) ;
#40885 = ORIENTED_EDGE ( 'NONE', *, *, #31338, .T. ) ;
#40886 = FACE_OUTER_BOUND ( 'NONE', #31053, .T. ) ;
#40887 = CARTESIAN_POINT ( 'NONE',  ( -0.07591351300297284610, 3.346456692913386100, 1.850393700787392293 ) ) ;
#40888 = CARTESIAN_POINT ( 'NONE',  ( 0.002207914879453961969, 6.692913385826772199, 0.04916304461325451958 ) ) ;
#40889 = VERTEX_POINT ( 'NONE', #670 ) ;
#40890 = DIRECTION ( 'NONE',  ( 5.782411586589357392E-17, 0.000000000000000000, 1.000000000000000000 ) ) ;
#40891 = DIRECTION ( 'NONE',  ( 1.000000000000000000, 0.000000000000000000, -3.469446951953613696E-16 ) ) ;
#40892 = EDGE_LOOP ( 'NONE', ( #34306, #24366, #47330, #33604 ) ) ;
#40893 = DIRECTION ( 'NONE',  ( 1.000000000000000000, -0.000000000000000000, 0.000000000000000000 ) ) ;
#40894 = DIRECTION ( 'NONE',  ( -0.000000000000000000, 1.000000000000000000, -0.000000000000000000 ) ) ;
#40895 = ORIENTED_EDGE ( 'NONE', *, *, #8261, .T. ) ;
#40896 = DIRECTION ( 'NONE',  ( -0.01601477604151182663, 0.9998717552508123996, -0.000000000000000000 ) ) ;
#40897 = EDGE_CURVE ( 'NONE', #24770, #42837, #13067, .T. ) ;
#40898 = CARTESIAN_POINT ( 'NONE',  ( 1.091055626815042423, 0.000000000000000000, -1.259842519685035134 ) ) ;
#40899 = DIRECTION ( 'NONE',  ( 1.000000000000000000, 0.000000000000000000, 0.000000000000000000 ) ) ;
#40900 = DIRECTION ( 'NONE',  ( 0.7071067811865463515, 0.000000000000000000, -0.7071067811865487940 ) ) ;
#40901 = AXIS2_PLACEMENT_3D ( 'NONE', #41637, #25887, #24874 ) ;
#40902 = EDGE_CURVE ( 'NONE', #8821, #28712, #32178, .T. ) ;
#40903 = EDGE_CURVE ( 'NONE', #6366, #8029, #12540, .T. ) ;
#40904 = LINE ( 'NONE', #21531, #27957 ) ;
#40905 = ORIENTED_EDGE ( 'NONE', *, *, #12095, .T. ) ;
#40906 = ORIENTED_EDGE ( 'NONE', *, *, #1683, .T. ) ;
#40907 = CARTESIAN_POINT ( 'NONE',  ( -2.182111253630085290, 3.346456692913386100, 0.4330708661417290162 ) ) ;
#40908 = VECTOR ( 'NONE', #2089, 39.37007874015748143 ) ;
#40909 = EDGE_CURVE ( 'NONE', #20873, #5560, #1318, .T. ) ;
#40910 = CARTESIAN_POINT ( 'NONE',  ( 2.106197740627112402, 3.267716535433071279, -0.5026832550384014997 ) ) ;
#40911 = CIRCLE ( 'NONE', #21116, 1.850107469027523432 ) ;
#40912 = ORIENTED_EDGE ( 'NONE', *, *, #44147, .T. ) ;
#40913 = DIRECTION ( 'NONE',  ( -0.9998717552508121775, -0.01601477604151182663, 0.000000000000000000 ) ) ;
#40914 = CARTESIAN_POINT ( 'NONE',  ( -1.805735793713946435, 1.049866565877818347, 0.9158222790674427349 ) ) ;
#40915 = CARTESIAN_POINT ( 'NONE',  ( -1.363819533518803029, 0.000000000000000000, 0.1574803149606287811 ) ) ;
#40916 = VECTOR ( 'NONE', #28115, 39.37007874015748143 ) ;
#40917 = DIRECTION ( 'NONE',  ( -0.000000000000000000, 1.000000000000000000, -0.000000000000000000 ) ) ;
#40918 = ORIENTED_EDGE ( 'NONE', *, *, #17207, .T. ) ;
#40919 = ORIENTED_EDGE ( 'NONE', *, *, #17418, .T. ) ;
#40920 = FACE_OUTER_BOUND ( 'NONE', #35635, .T. ) ;
#40921 = FACE_OUTER_BOUND ( 'NONE', #23191, .T. ) ;
#40922 = VECTOR ( 'NONE', #9525, 39.37007874015748143 ) ;
#40923 = CARTESIAN_POINT ( 'NONE',  ( -1.091055626815042201, 0.000000000000000000, 0.4330708661417290162 ) ) ;
#40924 = ORIENTED_EDGE ( 'NONE', *, *, #30811, .T. ) ;
#40925 = CARTESIAN_POINT ( 'NONE',  ( 1.833433833923351353, 3.346456692913386100, -0.9448818897637765168 ) ) ;
#40927 = AXIS2_PLACEMENT_3D ( 'NONE', #22616, #22116, #17731 ) ;
#40926 = FACE_BOUND ( 'NONE', #14653, .T. ) ;
#40928 = EDGE_LOOP ( 'NONE', ( #29058, #41939, #29871, #296 ) ) ;
#40929 = CARTESIAN_POINT ( 'NONE',  ( -1.636583440222563635, 0.000000000000000000, 0.1181102362204704270 ) ) ;
#40930 = ORIENTED_EDGE ( 'NONE', *, *, #11157, .F. ) ;
#40931 = EDGE_LOOP ( 'NONE', ( #36650, #29378, #16259, #36391 ) ) ;
#40932 = CARTESIAN_POINT ( 'NONE',  ( -0.08518262569720812249, 0.000000000000000000, 0.003633560317753287746 ) ) ;
#40934 = ORIENTED_EDGE ( 'NONE', *, *, #15135, .T. ) ;
#40933 = EDGE_CURVE ( 'NONE', #46112, #22897, #8672, .T. ) ;
#40935 = DIRECTION ( 'NONE',  ( 0.000000000000000000, 1.000000000000000000, 0.000000000000000000 ) ) ;
#40936 = CARTESIAN_POINT ( 'NONE',  ( -2.734482843737247038, 1.676638068352269029, -1.115254632218712016 ) ) ;
#40937 = ORIENTED_EDGE ( 'NONE', *, *, #22982, .F. ) ;
#40938 = CARTESIAN_POINT ( 'NONE',  ( -1.439733046521776361, 3.267716535433071279, 4.995077429881866871E-16 ) ) ;
#40939 = LINE ( 'NONE', #41699, #38480 ) ;
#40940 = ADVANCED_FACE ( 'NONE', ( #24680 ), #31655, .F. ) ;
#40941 = LINE ( 'NONE', #21063, #47262 ) ;
#40942 = EDGE_CURVE ( 'NONE', #49645, #29198, #8163, .T. ) ;
#40943 = EDGE_CURVE ( 'NONE', #19430, #16862, #16139, .T. ) ;
#40944 = VECTOR ( 'NONE', #49660, 39.37007874015748143 ) ;
#40945 = CARTESIAN_POINT ( 'NONE',  ( -2.182111253630085734, 3.267716535433070391, -1.099868863272876141 ) ) ;
#40946 = CARTESIAN_POINT ( 'NONE',  ( 1.636583440222563635, 3.346456692913386100, -1.417869535855832419 ) ) ;
#40947 = DIRECTION ( 'NONE',  ( -0.9959742939952397345, 1.288287287306305530E-16, 0.08963930890342654279 ) ) ;
#40948 = VECTOR ( 'NONE', #2759, 39.37007874015748143 ) ;
#40949 = EDGE_LOOP ( 'NONE', ( #43535, #50987, #35345, #7945 ) ) ;
#40950 = LINE ( 'NONE', #41707, #48871 ) ;
#40951 = VECTOR ( 'NONE', #38835, 39.37007874015748143 ) ;
#40952 = VECTOR ( 'NONE', #48609, 39.37007874015748143 ) ;
#40953 = DIRECTION ( 'NONE',  ( 1.734723475976806848E-16, -0.000000000000000000, 1.000000000000000000 ) ) ;
#40954 = VERTEX_POINT ( 'NONE', #23905 ) ;
#40955 = CARTESIAN_POINT ( 'NONE',  ( 0.4696143004045484903, 3.346456692913386100, 2.362204724409437961 ) ) ;
#40956 = CARTESIAN_POINT ( 'NONE',  ( -0.5455278134075208785, 0.000000000000000000, 1.377952755905504256 ) ) ;
#40957 = ORIENTED_EDGE ( 'NONE', *, *, #18510, .T. ) ;
#40958 = CARTESIAN_POINT ( 'NONE',  ( 1.363819533518803251, 3.346456692913386100, 1.102362204724403938 ) ) ;
#40959 = CIRCLE ( 'NONE', #30223, 1.850107469027523432 ) ;
#40960 = ADVANCED_FACE ( 'NONE', ( #33201 ), #38523, .F. ) ;
#40961 = CARTESIAN_POINT ( 'NONE',  ( -0.6094175224461334528, 1.205361022782829114E-17, 1.763844451117148271 ) ) ;
#40962 = DIRECTION ( 'NONE',  ( -1.000000000000000000, 0.000000000000000000, 0.000000000000000000 ) ) ;
#40963 = MANIFOLD_SOLID_BREP ( 'Cut-Extrude1', #1508 ) ;
#40964 = VECTOR ( 'NONE', #31569, 39.37007874015748143 ) ;
#40965 = B_SPLINE_CURVE_WITH_KNOTS ( 'NONE', 3,
 ( #14971, #27083, #14719, #7474 ),
 .UNSPECIFIED., .F., .F.,
 ( 4, 4 ),
 ( 0.02651100088651920511, 0.02872006419308328895 ),
 .UNSPECIFIED. ) ;
#40966 = ORIENTED_EDGE ( 'NONE', *, *, #34634, .T. ) ;
#40967 = LINE ( 'NONE', #9720, #15036 ) ;
#40968 = VERTEX_POINT ( 'NONE', #26384 ) ;
#40969 = FACE_BOUND ( 'NONE', #20159, .T. ) ;
#40970 = LINE ( 'NONE', #48911, #13569 ) ;
#40971 = EDGE_CURVE ( 'NONE', #35836, #31431, #39464, .T. ) ;
#40972 = LINE ( 'NONE', #2491, #30922 ) ;
#40973 = LINE ( 'NONE', #12574, #36683 ) ;
#40974 = EDGE_CURVE ( 'NONE', #31767, #20580, #14771, .T. ) ;
#40975 = EDGE_CURVE ( 'NONE', #1319, #5048, #30767, .T. ) ;
#40976 = ORIENTED_EDGE ( 'NONE', *, *, #21271, .T. ) ;
#40977 = ORIENTED_EDGE ( 'NONE', *, *, #33502, .T. ) ;
#40978 = EDGE_CURVE ( 'NONE', #13286, #31414, #25435, .T. ) ;
#40979 = DIRECTION ( 'NONE',  ( -1.000000000000000000, 0.000000000000000000, -0.000000000000000000 ) ) ;
#40980 = EDGE_CURVE ( 'NONE', #50863, #17115, #18386, .T. ) ;
#40981 = EDGE_LOOP ( 'NONE', ( #43753, #30364, #14165, #37116 ) ) ;
#40982 = LINE ( 'NONE', #48413, #19449 ) ;
#40983 = EDGE_LOOP ( 'NONE', ( #23463, #17949 ) ) ;
#40984 = PLANE ( 'NONE',  #36348 ) ;
#40985 = VERTEX_POINT ( 'NONE', #30519 ) ;
#40986 = DIRECTION ( 'NONE',  ( 0.000000000000000000, -1.000000000000000000, 0.000000000000000000 ) ) ;
#40987 = CIRCLE ( 'NONE', #12962, 1.743387098533651480 ) ;
#40988 = CARTESIAN_POINT ( 'NONE',  ( -0.6380732109764247761, 1.697682040615038801, -2.127022210610377773 ) ) ;
#40989 = AXIS2_PLACEMENT_3D ( 'NONE', #45351, #33014, #25497 ) ;
#40990 = ORIENTED_EDGE ( 'NONE', *, *, #20694, .F. ) ;
#40991 = CARTESIAN_POINT ( 'NONE',  ( -0.8182917201112814842, 0.000000000000000000, 0.2755905511810998187 ) ) ;
#40992 = ORIENTED_EDGE ( 'NONE', *, *, #15762, .T. ) ;
#40993 = VERTEX_POINT ( 'NONE', #46232 ) ;
#40994 = VECTOR ( 'NONE', #36166, 39.37007874015748143 ) ;
#40995 = ORIENTED_EDGE ( 'NONE', *, *, #7887, .F. ) ;
#40996 = VERTEX_POINT ( 'NONE', #46480 ) ;
#40997 = LINE ( 'NONE', #13367, #18682 ) ;
#40998 = EDGE_LOOP ( 'NONE', ( #24267, #14057, #36637, #774 ) ) ;
#40999 = LINE ( 'NONE', #5622, #18835 ) ;
#41000 = VERTEX_POINT ( 'NONE', #38022 ) ;
#41001 = CARTESIAN_POINT ( 'NONE',  ( -2.325625524897931840, 1.576417212481815211, 0.7038963509006195274 ) ) ;
#41002 = B_SPLINE_CURVE_WITH_KNOTS ( 'NONE', 3,
 ( #6754, #50556, #29990, #7508 ),
 .UNSPECIFIED., .F., .F.,
 ( 4, 4 ),
 ( 2.655964760909496045E-07, 0.002500437657294805275 ),
 .UNSPECIFIED. ) ;
#41003 = ADVANCED_FACE ( 'NONE', ( #10889 ), #34147, .F. ) ;
#41004 = DIRECTION ( 'NONE',  ( 5.175581015019631661E-17, -0.9063077870366510469, 0.4226182617406972208 ) ) ;
#41005 = EDGE_LOOP ( 'NONE', ( #25934, #24224, #14051, #38567 ) ) ;
#41006 = EDGE_CURVE ( 'NONE', #14697, #28392, #5305, .T. ) ;
#41007 = CARTESIAN_POINT ( 'NONE',  ( 0.1067246931122726866, 0.02962905676920215767, 0.000000000000000000 ) ) ;
#41008 = DIRECTION ( 'NONE',  ( 1.000000000000000000, 0.000000000000000000, 0.000000000000000000 ) ) ;
#41009 = ORIENTED_EDGE ( 'NONE', *, *, #11327, .F. ) ;
#41010 = CARTESIAN_POINT ( 'NONE',  ( 1.129748414438405124, 1.627571742414081202, 1.986830176535870907 ) ) ;
#41011 = CARTESIAN_POINT ( 'NONE',  ( 1.556712866041120247, 1.480457248723645591, 2.509548638715870084 ) ) ;
#41012 = CARTESIAN_POINT ( 'NONE',  ( 1.746845460392688620, 0.000000000000000000, -1.172799208037324847 ) ) ;
#41013 = LINE ( 'NONE', #5379, #23196 ) ;
#41014 = FACE_OUTER_BOUND ( 'NONE', #39488, .T. ) ;
#41015 = ORIENTED_EDGE ( 'NONE', *, *, #18777, .F. ) ;
#41016 = CARTESIAN_POINT ( 'NONE',  ( 0.1067246931122726866, 0.02962905676920215767, 0.000000000000000000 ) ) ;
#41017 = AXIS2_PLACEMENT_3D ( 'NONE', #21909, #37150, #41025 ) ;
#41018 = AXIS2_PLACEMENT_3D ( 'NONE', #7239, #22977, #10347 ) ;
#41019 = CARTESIAN_POINT ( 'NONE',  ( -1.014069264286641792, 0.4724409448818898127, -1.014069264286642458 ) ) ;
#41020 = EDGE_LOOP ( 'NONE', ( #24487, #17012, #34994, #34689 ) ) ;
#41021 = VECTOR ( 'NONE', #33468, 39.37007874015748143 ) ;
#41022 = CARTESIAN_POINT ( 'NONE',  ( 1.636583440222563635, 3.346456692913386100, -1.325930245594399537 ) ) ;
#41023 = EDGE_CURVE ( 'NONE', #2513, #5755, #34646, .T. ) ;
#41024 = ORIENTED_EDGE ( 'NONE', *, *, #40136, .F. ) ;
#41025 = DIRECTION ( 'NONE',  ( -1.000000000000000000, 0.000000000000000000, -0.000000000000000000 ) ) ;
#41026 = PLANE ( 'NONE',  #35782 ) ;
#41027 = CARTESIAN_POINT ( 'NONE',  ( -0.6690177265809421625, 0.000000000000000000, 1.735666008086750089 ) ) ;
#41028 = EDGE_CURVE ( 'NONE', #1621, #20851, #37636, .T. ) ;
#41029 = DIRECTION ( 'NONE',  ( -0.000000000000000000, 1.000000000000000000, -0.000000000000000000 ) ) ;
#41030 = CARTESIAN_POINT ( 'NONE',  ( 2.106197740627111514, 0.000000000000000000, -0.7874015748031473194 ) ) ;
#41031 = ORIENTED_EDGE ( 'NONE', *, *, #9642, .T. ) ;
#41032 = EDGE_CURVE ( 'NONE', #36221, #29961, #36812, .T. ) ;
#41033 = CARTESIAN_POINT ( 'NONE',  ( 0.000000000000000000, 3.267716535433071279, -1.614173228346451605 ) ) ;
#41034 = FACE_BOUND ( 'NONE', #36252, .T. ) ;
#41035 = ADVANCED_FACE ( 'NONE', ( #39265 ), #8283, .T. ) ;
#41036 = VERTEX_POINT ( 'NONE', #11900 ) ;
#41037 = CARTESIAN_POINT ( 'NONE',  ( 0.8182917201112819283, 0.000000000000000000, -1.102362204724405714 ) ) ;
#41038 = VECTOR ( 'NONE', #28804, 39.37007874015748143 ) ;
#41039 = B_SPLINE_CURVE_WITH_KNOTS ( 'NONE', 3,
 ( #6213, #26081, #13446, #6469 ),
 .UNSPECIFIED., .F., .F.,
 ( 4, 4 ),
 ( 0.002601184284654935782, 0.004660285992363409451 ),
 .UNSPECIFIED. ) ;
#41040 = VERTEX_POINT ( 'NONE', #7522 ) ;
#41041 = CARTESIAN_POINT ( 'NONE',  ( -1.363819533518803473, 0.000000000000000000, -0.7874015748031470974 ) ) ;
#41042 = FACE_OUTER_BOUND ( 'NONE', #45098, .T. ) ;
#41043 = DIRECTION ( 'NONE',  ( 0.000000000000000000, 0.000000000000000000, -1.000000000000000000 ) ) ;
#41044 = MANIFOLD_SOLID_BREP ( 'CirPattern1', #19652 ) ;
#41045 = DIRECTION ( 'NONE',  ( -0.9998717552508121775, -0.01601477604151182663, 0.000000000000000000 ) ) ;
#41046 = VERTEX_POINT ( 'NONE', #19634 ) ;
#41047 = EDGE_LOOP ( 'NONE', ( #41747, #7796, #36058, #32884 ) ) ;
#41048 = DIRECTION ( 'NONE',  ( 1.142080616180678453E-16, -1.000000000000000000, 2.072570748943325363E-17 ) ) ;
#41049 = CARTESIAN_POINT ( 'NONE',  ( 2.298708793198899425, 2.755905511811027164, 1.181102362204724088 ) ) ;
#41050 = FACE_BOUND ( 'NONE', #21392, .T. ) ;
#41051 = ORIENTED_EDGE ( 'NONE', *, *, #1211, .T. ) ;
#41052 = CARTESIAN_POINT ( 'NONE',  ( 1.636583440222563857, 3.267716535433071279, 0.6299212598425164567 ) ) ;
#41053 = DIRECTION ( 'NONE',  ( 1.000000000000000000, -0.000000000000000000, 0.000000000000000000 ) ) ;
#41054 = AXIS2_PLACEMENT_3D ( 'NONE', #46818, #11492, #50921 ) ;
#41055 = VECTOR ( 'NONE', #2857, 39.37007874015748143 ) ;
#41056 = VERTEX_POINT ( 'NONE', #8026 ) ;
#41057 = ORIENTED_EDGE ( 'NONE', *, *, #47094, .T. ) ;
#41058 = DIRECTION ( 'NONE',  ( 1.000000000000000000, 0.000000000000000000, -3.469446951953613696E-16 ) ) ;
#41059 = CARTESIAN_POINT ( 'NONE',  ( -1.057143431661237143, 3.346456692913386100, -1.889763779527552146 ) ) ;
#41060 = VERTEX_POINT ( 'NONE', #31277 ) ;
#41061 = ORIENTED_EDGE ( 'NONE', *, *, #27757, .F. ) ;
#41062 = VECTOR ( 'NONE', #23185, 39.37007874015748143 ) ;
#41063 = ORIENTED_EDGE ( 'NONE', *, *, #26497, .F. ) ;
#41064 = CARTESIAN_POINT ( 'NONE',  ( -2.101347671104863313, 1.674245022174266406, -0.5300970854448181502 ) ) ;
#41065 = CARTESIAN_POINT ( 'NONE',  ( 1.015142113812069313, 3.346456692913386100, 1.102362204724403938 ) ) ;
#41066 = CARTESIAN_POINT ( 'NONE',  ( 0.000000000000000000, 3.267716535433071279, 0.000000000000000000 ) ) ;
#41067 = CARTESIAN_POINT ( 'NONE',  ( 1.287906020515830141, 3.346456692913386100, 0.9448818897637746295 ) ) ;
#41068 = CIRCLE ( 'NONE', #47613, 2.164630168518208109 ) ;
#41069 = ORIENTED_EDGE ( 'NONE', *, *, #20762, .T. ) ;
#41070 = ORIENTED_EDGE ( 'NONE', *, *, #29987, .F. ) ;
#41071 = ADVANCED_FACE ( 'NONE', ( #4157 ), #39778, .F. ) ;
#41072 = CARTESIAN_POINT ( 'NONE',  ( 0.5756566573088583993, 5.905511811023623991, 2.896516654582643291 ) ) ;
#41073 = LENGTH_MEASURE_WITH_UNIT ( LENGTH_MEASURE( 0.02539999999999999897 ), #48508 );
#41074 = EDGE_CURVE ( 'NONE', #26643, #17294, #17969, .T. ) ;
#41075 = CARTESIAN_POINT ( 'NONE',  ( -0.5455278134075208785, 3.346456692913386100, 1.259842519685033357 ) ) ;
#41076 = CARTESIAN_POINT ( 'NONE',  ( -0.3486774197067340486, 0.000000000000000000, -1.771653543307081025 ) ) ;
#41077 = EDGE_CURVE ( 'NONE', #49909, #36932, #34894, .T. ) ;
#41078 = DIRECTION ( 'NONE',  ( 0.000000000000000000, 0.000000000000000000, 1.000000000000000000 ) ) ;
#41079 = CARTESIAN_POINT ( 'NONE',  ( 0.3595914698493179462, 0.000000000000000000, 1.705899337635486290 ) ) ;
#41080 = CARTESIAN_POINT ( 'NONE',  ( 1.636583440222563635, 3.346456692913386100, -0.9448818897637765168 ) ) ;
#41081 = VERTEX_POINT ( 'NONE', #15768 ) ;
#41082 = CARTESIAN_POINT ( 'NONE',  ( -1.091055626815042645, 0.000000000000000000, -1.771653543307081025 ) ) ;
#41083 = DIRECTION ( 'NONE',  ( 0.000000000000000000, 1.160734090543304660E-16, -1.000000000000000000 ) ) ;
#41084 = VERTEX_POINT ( 'NONE', #31019 ) ;
#41085 = ORIENTED_EDGE ( 'NONE', *, *, #10074, .T. ) ;
#41086 = DIRECTION ( 'NONE',  ( 1.000000000000000000, 0.000000000000000000, 0.000000000000000000 ) ) ;
#41087 = DIRECTION ( 'NONE',  ( -1.000000000000000000, 0.000000000000000000, 1.734723475976806848E-16 ) ) ;
#41088 = EDGE_CURVE ( 'NONE', #21474, #28376, #50576, .T. ) ;
#41089 = VECTOR ( 'NONE', #10293, 39.37007874015748143 ) ;
#41090 = VERTEX_POINT ( 'NONE', #31787 ) ;
#41091 = EDGE_CURVE ( 'NONE', #48217, #4317, #23775, .T. ) ;
#41092 = ORIENTED_EDGE ( 'NONE', *, *, #548, .F. ) ;
#41093 = CARTESIAN_POINT ( 'NONE',  ( 1.733526556417521958, 0.000000000000000000, 0.1851600754179809072 ) ) ;
#41094 = VECTOR ( 'NONE', #37828, 39.37007874015748143 ) ;
#41095 = VERTEX_POINT ( 'NONE', #15271 ) ;
#41096 = VECTOR ( 'NONE', #22039, 39.37007874015748143 ) ;
#41097 = DIRECTION ( 'NONE',  ( -1.000000000000000000, 0.000000000000000000, 1.734723475976806848E-16 ) ) ;
#41098 = DIRECTION ( 'NONE',  ( -1.000000000000000000, 0.000000000000000000, 0.000000000000000000 ) ) ;
#41099 = VECTOR ( 'NONE', #12863, 39.37007874015748143 ) ;
#41100 = ORIENTED_EDGE ( 'NONE', *, *, #27297, .F. ) ;
#41101 = ORIENTED_EDGE ( 'NONE', *, *, #28978, .F. ) ;
#41102 = EDGE_LOOP ( 'NONE', ( #15725, #12443, #23273, #20638 ) ) ;
#41103 = CARTESIAN_POINT ( 'NONE',  ( -1.909347346926324906, 3.346456692913386100, 1.220472440944875059 ) ) ;
#41104 = ORIENTED_EDGE ( 'NONE', *, *, #3043, .T. ) ;
#41105 = ORIENTED_EDGE ( 'NONE', *, *, #38739, .F. ) ;
#41106 = CARTESIAN_POINT ( 'NONE',  ( -2.456251886791057437, 1.676905504490172838, -1.103371865719809275 ) ) ;
#41107 = PLANE ( 'NONE',  #507 ) ;
#41108 = DIRECTION ( 'NONE',  ( 1.000000000000000000, 0.000000000000000000, 0.000000000000000000 ) ) ;
#41109 = VECTOR ( 'NONE', #29900, 39.37007874015748143 ) ;
#41110 = ADVANCED_FACE ( 'NONE', ( #31527 ), #12157, .F. ) ;
#41111 = ORIENTED_EDGE ( 'NONE', *, *, #16649, .T. ) ;
#41112 = CARTESIAN_POINT ( 'NONE',  ( 0.7423782071083085965, 3.346456692913386100, -1.456692913385822630 ) ) ;
#41113 = CARTESIAN_POINT ( 'NONE',  ( -0.9302092402134520821, 3.267716535433071279, -1.889763779527552146 ) ) ;
#41114 = CARTESIAN_POINT ( 'NONE',  ( 3.937007874015748143, 2.913385826771657250, -1.023622047244094224 ) ) ;
#41115 = VERTEX_POINT ( 'NONE', #47484 ) ;
#41116 = DIRECTION ( 'NONE',  ( 0.000000000000000000, -1.000000000000000000, 0.000000000000000000 ) ) ;
#41117 = DIRECTION ( 'NONE',  ( 0.9998717552508121775, 0.01601477604151182663, 0.000000000000000000 ) ) ;
#41118 = FACE_OUTER_BOUND ( 'NONE', #4761, .T. ) ;
#41119 = ORIENTED_EDGE ( 'NONE', *, *, #49416, .T. ) ;
#41120 = EDGE_LOOP ( 'NONE', ( #7968, #40755, #34586, #30757 ) ) ;
#41121 = CARTESIAN_POINT ( 'NONE',  ( -0.2727639067037608278, 0.000000000000000000, -0.9842519685039344823 ) ) ;
#41122 = VECTOR ( 'NONE', #22365, 39.37007874015748143 ) ;
#41123 = DIRECTION ( 'NONE',  ( 1.000000000000000000, -0.000000000000000000, 0.000000000000000000 ) ) ;
#41124 = DIRECTION ( 'NONE',  ( 1.000000000000000000, 0.000000000000000000, 0.000000000000000000 ) ) ;
#41125 = VERTEX_POINT ( 'NONE', #5435 ) ;
#41126 = ORIENTED_EDGE ( 'NONE', *, *, #8999, .F. ) ;
#41127 = EDGE_CURVE ( 'NONE', #9666, #36309, #29178, .T. ) ;
#41128 = PLANE ( 'NONE',  #3638 ) ;
#41129 = EDGE_LOOP ( 'NONE', ( #33893, #7963, #40771, #21947 ) ) ;
#41130 = CARTESIAN_POINT ( 'NONE',  ( 0.000000000000000000, 3.267716535433071279, 1.062992125984246083 ) ) ;
#41131 = LINE ( 'NONE', #21249, #30884 ) ;
#41132 = ADVANCED_FACE ( 'NONE', ( #24544 ), #20411, .F. ) ;
#41133 = AXIS2_PLACEMENT_3D ( 'NONE', #29223, #25352, #5734 ) ;
#41134 = VECTOR ( 'NONE', #41534, 39.37007874015748143 ) ;
#41135 = EDGE_CURVE ( 'NONE', #32722, #50026, #36945, .T. ) ;
#41136 = ADVANCED_FACE ( 'NONE', ( #36426 ), #20666, .F. ) ;
#41137 = VECTOR ( 'NONE', #16804, 39.37007874015748143 ) ;
#41139 = B_SPLINE_CURVE_WITH_KNOTS ( 'NONE', 3,
 ( #2159, #29008, #48845, #25394 ),
 .UNSPECIFIED., .F., .F.,
 ( 4, 4 ),
 ( 0.1211775127643062860, 0.1625894504277921315 ),
 .UNSPECIFIED. ) ;
#41138 = CARTESIAN_POINT ( 'NONE',  ( 0.2727639067037610499, 0.000000000000000000, 2.362204724409437961 ) ) ;
#41140 = DIRECTION ( 'NONE',  ( 1.000000000000000000, 0.000000000000000000, 0.000000000000000000 ) ) ;
#41141 = CARTESIAN_POINT ( 'NONE',  ( 0.000000000000000000, 3.346456692913386100, 0.000000000000000000 ) ) ;
#41142 = ORIENTED_EDGE ( 'NONE', *, *, #9538, .F. ) ;
#41143 = CARTESIAN_POINT ( 'NONE',  ( 1.329442508636073939, 1.634319695305515463, 2.129162132572615551 ) ) ;
#41144 = DIRECTION ( 'NONE',  ( -1.000000000000000000, -0.000000000000000000, -0.000000000000000000 ) ) ;
#41145 = VECTOR ( 'NONE', #47054, 39.37007874015748143 ) ;
#41146 = CARTESIAN_POINT ( 'NONE',  ( 0.2483449720853004861, 1.723125804968587360, -2.942339427345150860 ) ) ;
#41147 = VERTEX_POINT ( 'NONE', #47993 ) ;
#41148 = LINE ( 'NONE', #2152, #3428 ) ;
#41149 = PLANE ( 'NONE',  #13779 ) ;
#41150 = EDGE_CURVE ( 'NONE', #39017, #27844, #4925, .T. ) ;
#41151 = LINE ( 'NONE', #9386, #44437 ) ;
#41152 = ORIENTED_EDGE ( 'NONE', *, *, #12396, .T. ) ;
#41153 = DIRECTION ( 'NONE',  ( 7.237058681235334921E-17, -1.000000000000000000, -9.074984547606431700E-17 ) ) ;
#41154 = CARTESIAN_POINT ( 'NONE',  ( 1.363819533518803251, 3.267716535433071279, -0.03937007874015908959 ) ) ;
#41155 = ADVANCED_FACE ( 'NONE', ( #44659 ), #28148, .F. ) ;
#41156 = ORIENTED_EDGE ( 'NONE', *, *, #24195, .T. ) ;
#41157 = CARTESIAN_POINT ( 'NONE',  ( -2.154836593528564492, 1.574965465101147766, -0.2160053639259867930 ) ) ;
#41158 = CARTESIAN_POINT ( 'NONE',  ( -0.1450362469327511061, 1.574803149606302854, -2.160491579385214411 ) ) ;
#41159 = ORIENTED_EDGE ( 'NONE', *, *, #30525, .T. ) ;
#41160 = DIRECTION ( 'NONE',  ( -1.000000000000000000, 0.000000000000000000, 0.000000000000000000 ) ) ;
#41161 = CARTESIAN_POINT ( 'NONE',  ( -1.891495399494460106, 1.644797792086550858, 1.073742665334450175 ) ) ;
#41162 = LINE ( 'NONE', #21791, #8221 ) ;
#41163 = CARTESIAN_POINT ( 'NONE',  ( -2.047355983664255863, 1.576684601009278319, 0.7169714724935087879 ) ) ;
#41164 = AXIS2_PLACEMENT_3D ( 'NONE', #22049, #37807, #21798 ) ;
#41165 = ADVANCED_FACE ( 'NONE', ( #32827 ), #8797, .F. ) ;
#41166 = DIRECTION ( 'NONE',  ( -0.9362348706397368714, -1.160734090543304413E-16, -0.3513748240813434620 ) ) ;
#41167 = ORIENTED_EDGE ( 'NONE', *, *, #2840, .T. ) ;
#41168 = ORIENTED_EDGE ( 'NONE', *, *, #42297, .F. ) ;
#41169 = DIRECTION ( 'NONE',  ( -0.9998717552508122886, -0.01601477604151181275, 0.000000000000000000 ) ) ;
#41170 = CARTESIAN_POINT ( 'NONE',  ( -1.723188456408593527, 6.692913385826772199, 1.311251662046200472 ) ) ;
#41171 = EDGE_LOOP ( 'NONE', ( #20254, #24855, #17484, #43829 ) ) ;
#41172 = DIRECTION ( 'NONE',  ( -3.469446951953613696E-16, 0.000000000000000000, -1.000000000000000000 ) ) ;
#41173 = LINE ( 'NONE', #5794, #35972 ) ;
#41174 = CARTESIAN_POINT ( 'NONE',  ( 1.015142113812069091, 3.346456692913386100, -1.912654141836395816 ) ) ;
#41175 = EDGE_CURVE ( 'NONE', #36717, #31407, #12936, .T. ) ;
#41176 = VECTOR ( 'NONE', #36741, 39.37007874015748143 ) ;
#41177 = ORIENTED_EDGE ( 'NONE', *, *, #11699, .F. ) ;
#41178 = ORIENTED_EDGE ( 'NONE', *, *, #2973, .F. ) ;
#41179 = LINE ( 'NONE', #17929, #4863 ) ;
#41180 = CARTESIAN_POINT ( 'NONE',  ( 0.5455278134075212115, 0.000000000000000000, 0.6299212598425161236 ) ) ;
#41181 = CARTESIAN_POINT ( 'NONE',  ( -2.449433152083427601, 3.244423651327855485, 0.1574803149606286423 ) ) ;
#41182 = ORIENTED_EDGE ( 'NONE', *, *, #18329, .T. ) ;
#41183 = VECTOR ( 'NONE', #23606, 39.37007874015748143 ) ;
#41184 = FACE_BOUND ( 'NONE', #35359, .T. ) ;
#41185 = ORIENTED_EDGE ( 'NONE', *, *, #50211, .T. ) ;
#41186 = EDGE_CURVE ( 'NONE', #22883, #20959, #44411, .T. ) ;
#41187 = DIRECTION ( 'NONE',  ( 0.000000000000000000, -1.000000000000000000, 0.000000000000000000 ) ) ;
#41188 = ORIENTED_EDGE ( 'NONE', *, *, #46447, .T. ) ;
#41189 = ORIENTED_EDGE ( 'NONE', *, *, #45839, .F. ) ;
#41190 = VECTOR ( 'NONE', #45250, 39.37007874015748143 ) ;
#41191 = FACE_OUTER_BOUND ( 'NONE', #43884, .T. ) ;
#41192 = CARTESIAN_POINT ( 'NONE',  ( 1.478089240774732582, 0.05159396975604255142, 1.241682111880268558 ) ) ;
#41193 = EDGE_CURVE ( 'NONE', #31407, #44897, #21445, .T. ) ;
#41194 = ORIENTED_EDGE ( 'NONE', *, *, #32737, .F. ) ;
#41195 = DIRECTION ( 'NONE',  ( 1.734723475976806848E-16, 0.000000000000000000, 1.000000000000000000 ) ) ;
#41196 = CARTESIAN_POINT ( 'NONE',  ( 0.000000000000000000, 3.267716535433071279, 1.732283464566921172 ) ) ;
#41197 = ORIENTED_EDGE ( 'NONE', *, *, #2616, .F. ) ;
#41198 = CARTESIAN_POINT ( 'NONE',  ( 0.000000000000000000, 3.267716535433071279, 2.007874015748021268 ) ) ;
#41199 = CARTESIAN_POINT ( 'NONE',  ( 1.083598637574782142, 1.637691314537677023, 2.747180975113346246 ) ) ;
#41200 = DIRECTION ( 'NONE',  ( 1.000000000000000000, 0.000000000000000000, -3.469446951953613696E-16 ) ) ;
#41201 = ADVANCED_FACE ( 'NONE', ( #40555 ), #21191, .F. ) ;
#41202 = CARTESIAN_POINT ( 'NONE',  ( -2.182111253630085734, 3.254137321050718956, -1.113937159217551764 ) ) ;
#41203 = EDGE_CURVE ( 'NONE', #23878, #10495, #29605, .T. ) ;
#41204 = FACE_OUTER_BOUND ( 'NONE', #50266, .T. ) ;
#41205 = CARTESIAN_POINT ( 'NONE',  ( -1.636583440222563635, 3.346456692913386100, 0.4330708661417290162 ) ) ;
#41206 = ORIENTED_EDGE ( 'NONE', *, *, #8003, .T. ) ;
#41207 = DIRECTION ( 'NONE',  ( 0.000000000000000000, -1.000000000000000000, -0.000000000000000000 ) ) ;
#41208 = CARTESIAN_POINT ( 'NONE',  ( 0.000000000000000000, 3.267716535433071279, 0.1181102362204701633 ) ) ;
#41209 = VECTOR ( 'NONE', #18326, 39.37007874015748143 ) ;
#41210 = ORIENTED_EDGE ( 'NONE', *, *, #34551, .F. ) ;
#41211 = PLANE ( 'NONE',  #24021 ) ;
#41212 = CARTESIAN_POINT ( 'NONE',  ( -1.166969139818015977, 3.267716535433071279, -0.7874015748031470974 ) ) ;
#41213 = EDGE_LOOP ( 'NONE', ( #23053, #46435, #39279, #28428 ) ) ;
#41214 = DIRECTION ( 'NONE',  ( 0.000000000000000000, 1.160734090543304660E-16, -1.000000000000000000 ) ) ;
#41215 = DIRECTION ( 'NONE',  ( -1.000000000000000000, -0.000000000000000000, -0.000000000000000000 ) ) ;
#41216 = CARTESIAN_POINT ( 'NONE',  ( 1.930898218216747120, 1.205361022782829114E-17, -0.8788249315385436855 ) ) ;
#41217 = MANIFOLD_SOLID_BREP ( 'Shell1', #33708 ) ;
#41218 = VERTEX_POINT ( 'NONE', #46174 ) ;
#41219 = LINE ( 'NONE', #33983, #25495 ) ;
#41220 = CIRCLE ( 'NONE', #3278, 2.066929133858268042 ) ;
#41221 = VERTEX_POINT ( 'NONE', #49521 ) ;
#41222 = FACE_BOUND ( 'NONE', #20455, .T. ) ;
#41223 = DIRECTION ( 'NONE',  ( -3.469446951953613696E-16, 0.000000000000000000, -1.000000000000000000 ) ) ;
#41224 = LINE ( 'NONE', #5335, #29253 ) ;
#41225 = FACE_OUTER_BOUND ( 'NONE', #40822, .T. ) ;
#41226 = EDGE_CURVE ( 'NONE', #40680, #33135, #33077, .T. ) ;
#41227 = ORIENTED_EDGE ( 'NONE', *, *, #27872, .T. ) ;
#41228 = VERTEX_POINT ( 'NONE', #30204 ) ;
#41229 = LINE ( 'NONE', #13098, #26301 ) ;
#41230 = ORIENTED_EDGE ( 'NONE', *, *, #9889, .F. ) ;
#41231 = CARTESIAN_POINT ( 'NONE',  ( -0.6214413264104945434, 0.000000000000000000, -0.4724409448818886470 ) ) ;
#41232 = ORIENTED_EDGE ( 'NONE', *, *, #40246, .F. ) ;
#41233 = EDGE_CURVE ( 'NONE', #22611, #1994, #21698, .T. ) ;
#41234 = DIRECTION ( 'NONE',  ( -0.000000000000000000, -1.000000000000000000, -0.000000000000000000 ) ) ;
#41235 = EDGE_CURVE ( 'NONE', #38291, #23969, #37716, .T. ) ;
#41236 = VECTOR ( 'NONE', #29030, 39.37007874015748143 ) ;
#41237 = ORIENTED_EDGE ( 'NONE', *, *, #10527, .F. ) ;
#41238 = LINE ( 'NONE', #21360, #28213 ) ;
#41239 = EDGE_CURVE ( 'NONE', #41221, #39889, #10081, .T. ) ;
#41240 = DIRECTION ( 'NONE',  ( 1.734723475976806848E-16, -0.000000000000000000, 1.000000000000000000 ) ) ;
#41241 = EDGE_LOOP ( 'NONE', ( #25042, #18108, #32289, #22557 ) ) ;
#41242 = EDGE_CURVE ( 'NONE', #46048, #19150, #10833, .T. ) ;
#41243 = CARTESIAN_POINT ( 'NONE',  ( 1.636583440222563635, 0.000000000000000000, -0.9448818897637765168 ) ) ;
#41244 = ORIENTED_EDGE ( 'NONE', *, *, #40714, .T. ) ;
#41245 = ORIENTED_EDGE ( 'NONE', *, *, #26732, .T. ) ;
#41246 = VECTOR ( 'NONE', #10829, 39.37007874015748143 ) ;
#41247 = CIRCLE ( 'NONE', #23909, 2.165354330708661568 ) ;
#41248 = VERTEX_POINT ( 'NONE', #30464 ) ;
#41249 = ORIENTED_EDGE ( 'NONE', *, *, #7903, .F. ) ;
#41250 = DIRECTION ( 'NONE',  ( -0.9998717552508122886, -0.01601477604151185785, 0.000000000000000000 ) ) ;
#41251 = ORIENTED_EDGE ( 'NONE', *, *, #12189, .F. ) ;
#41252 = VECTOR ( 'NONE', #41098, 39.37007874015748143 ) ;
#41253 = DIRECTION ( 'NONE',  ( 1.734723475976806848E-16, -0.000000000000000000, 1.000000000000000000 ) ) ;
#41254 = DIRECTION ( 'NONE',  ( -3.469446951953613696E-16, 0.000000000000000000, -1.000000000000000000 ) ) ;
#41255 = EDGE_CURVE ( 'NONE', #17122, #43876, #17332, .T. ) ;
#41256 = CARTESIAN_POINT ( 'NONE',  ( 0.2727639067037604392, 3.346456692913386100, 0.2755905511810994302 ) ) ;
#41257 = EDGE_CURVE ( 'NONE', #32688, #29455, #26575, .T. ) ;
#41258 = ORIENTED_EDGE ( 'NONE', *, *, #48108, .F. ) ;
#41259 = CARTESIAN_POINT ( 'NONE',  ( -0.8182917201112814842, 0.000000000000000000, 1.220472440944875281 ) ) ;
#41260 = LINE ( 'NONE', #49710, #11430 ) ;
#41261 = EDGE_CURVE ( 'NONE', #34367, #41791, #50029, .T. ) ;
#41262 = ORIENTED_EDGE ( 'NONE', *, *, #8495, .T. ) ;
#41263 = CARTESIAN_POINT ( 'NONE',  ( 0.5455278134075208785, 3.346456692913386100, -1.574803149606293529 ) ) ;
#41264 = DIRECTION ( 'NONE',  ( -0.000000000000000000, -1.000000000000000000, -0.000000000000000000 ) ) ;
#41265 = CARTESIAN_POINT ( 'NONE',  ( 1.662320194739496770, 5.905511811023623991, -1.388601395075552247 ) ) ;
#41266 = DIRECTION ( 'NONE',  ( -9.701723960855857903E-17, 1.000000000000000000, 8.476140964546263859E-17 ) ) ;
#41267 = CARTESIAN_POINT ( 'NONE',  ( 1.979793062125284608, 1.651646828087945051, 2.191257344206569257 ) ) ;
#41268 = DIRECTION ( 'NONE',  ( -3.469446951953613696E-16, 0.000000000000000000, -1.000000000000000000 ) ) ;
#41269 = EDGE_LOOP ( 'NONE', ( #25418, #25870, #26313, #3382 ) ) ;
#41270 = DIRECTION ( 'NONE',  ( -2.582876339026340310E-17, -1.000000000000000000, 1.131632063491650798E-16 ) ) ;
#41271 = CARTESIAN_POINT ( 'NONE',  ( -0.3937007874015747699, 0.000000000000000000, -1.220472440944881942 ) ) ;
#41272 = EDGE_LOOP ( 'NONE', ( #13464, #26139, #42879, #15245 ) ) ;
#41273 = CARTESIAN_POINT ( 'NONE',  ( 0.000000000000000000, 3.267716535433071279, -0.8267716535433052849 ) ) ;
#41274 = ORIENTED_EDGE ( 'NONE', *, *, #452, .F. ) ;
#41275 = CARTESIAN_POINT ( 'NONE',  ( 1.680518189209764479, 0.01778946649618510026, -1.168267724599023838 ) ) ;
#41276 = CARTESIAN_POINT ( 'NONE',  ( -2.889674983507169337, 1.674218314264582785, -0.6090712660038034576 ) ) ;
#41277 = VECTOR ( 'NONE', #16555, 39.37007874015748143 ) ;
#41278 = DIRECTION ( 'NONE',  ( -0.000000000000000000, 1.000000000000000000, -0.000000000000000000 ) ) ;
#41279 = VECTOR ( 'NONE', #20310, 39.37007874015748143 ) ;
#41280 = DIRECTION ( 'NONE',  ( 1.000000000000000000, 0.000000000000000000, -3.469446951953613696E-16 ) ) ;
#41281 = PLANE ( 'NONE',  #31026 ) ;
#41282 = ORIENTED_EDGE ( 'NONE', *, *, #16179, .F. ) ;
#41283 = DIRECTION ( 'NONE',  ( -3.469446951953613696E-16, 0.000000000000000000, -1.000000000000000000 ) ) ;
#41284 = ORIENTED_EDGE ( 'NONE', *, *, #11452, .T. ) ;
#41285 = CARTESIAN_POINT ( 'NONE',  ( -1.891607981616729495, 1.579179190298960256, 1.073803248357834139 ) ) ;
#41286 = ORIENTED_EDGE ( 'NONE', *, *, #13187, .T. ) ;
#41287 = CARTESIAN_POINT ( 'NONE',  ( -1.166969139818015977, 3.267716535433071279, 2.047244094488179567 ) ) ;
#41288 = VECTOR ( 'NONE', #42796, 39.37007874015748143 ) ;
#41289 = PLANE ( 'NONE',  #11215 ) ;
#41290 = VERTEX_POINT ( 'NONE', #21958 ) ;
#41291 = DIRECTION ( 'NONE',  ( 0.6910626489868684219, 0.000000000000000000, -0.7227948638273878901 ) ) ;
#41292 = ADVANCED_FACE ( 'NONE', ( #17823 ), #29952, .F. ) ;
#41293 = LINE ( 'NONE', #31444, #45480 ) ;
#41294 = EDGE_CURVE ( 'NONE', #10030, #16727, #18839, .T. ) ;
#41295 = EDGE_CURVE ( 'NONE', #39335, #40266, #38468, .T. ) ;
#41296 = LINE ( 'NONE', #132, #4114 ) ;
#41297 = ORIENTED_EDGE ( 'NONE', *, *, #17357, .F. ) ;
#41298 = VERTEX_POINT ( 'NONE', #22213 ) ;
#41299 = DIRECTION ( 'NONE',  ( 1.000000000000000000, 0.000000000000000000, 0.000000000000000000 ) ) ;
#41300 = FACE_BOUND ( 'NONE', #5274, .T. ) ;
#41301 = ORIENTED_EDGE ( 'NONE', *, *, #11585, .T. ) ;
#41302 = DIRECTION ( 'NONE',  ( -1.000000000000000000, 0.000000000000000000, 0.000000000000000000 ) ) ;
#41303 = CARTESIAN_POINT ( 'NONE',  ( 0.5455278134075208785, 3.267716535433071279, -1.771653543307081025 ) ) ;
#41304 = ORIENTED_EDGE ( 'NONE', *, *, #45612, .T. ) ;
#41305 = ORIENTED_EDGE ( 'NONE', *, *, #18587, .F. ) ;
#41306 = CARTESIAN_POINT ( 'NONE',  ( -1.232620761116186126, 1.574803149606302854, -1.780282403660753410 ) ) ;
#41307 = DIRECTION ( 'NONE',  ( -3.469446951953613696E-16, 0.000000000000000000, -1.000000000000000000 ) ) ;
#41308 = ORIENTED_EDGE ( 'NONE', *, *, #44323, .F. ) ;
#41309 = EDGE_LOOP ( 'NONE', ( #15490, #4387, #45687, #42607 ) ) ;
#41310 = EDGE_CURVE ( 'NONE', #643, #33237, #15450, .T. ) ;
#41311 = ORIENTED_EDGE ( 'NONE', *, *, #41091, .T. ) ;
#41312 = CARTESIAN_POINT ( 'NONE',  ( 0.8182917201112817063, 3.267716535433071279, -2.244094488188969283 ) ) ;
#41313 = AXIS2_PLACEMENT_3D ( 'NONE', #1755, #22151, #17511 ) ;
#41314 = CARTESIAN_POINT ( 'NONE',  ( 1.909347346926324684, 0.000000000000000000, 0.7874015748031456541 ) ) ;
#41315 = EDGE_CURVE ( 'NONE', #1290, #34165, #33590, .T. ) ;
#41316 = VECTOR ( 'NONE', #21362, 39.37007874015748143 ) ;
#41317 = CARTESIAN_POINT ( 'NONE',  ( -0.9836083787002332102, 1.574803149606302854, -1.929060376159713375 ) ) ;
#41318 = CARTESIAN_POINT ( 'NONE',  ( 0.000000000000000000, 3.267716535433071279, 0.000000000000000000 ) ) ;
#41319 = ADVANCED_FACE ( 'NONE', ( #34589 ), #2837, .F. ) ;
#41320 = ORIENTED_EDGE ( 'NONE', *, *, #33572, .T. ) ;
#41321 = EDGE_LOOP ( 'NONE', ( #38638, #8380, #49442, #47157 ) ) ;
#41322 = LINE ( 'NONE', #37456, #36495 ) ;
#41323 = DIRECTION ( 'NONE',  ( -3.469446951953613696E-16, 0.000000000000000000, -1.000000000000000000 ) ) ;
#41324 = EDGE_CURVE ( 'NONE', #40996, #16084, #49277, .T. ) ;
#41325 = DIRECTION ( 'NONE',  ( 1.000000000000000000, -0.000000000000000000, 0.000000000000000000 ) ) ;
#41326 = VECTOR ( 'NONE', #42487, 39.37007874015748143 ) ;
#41327 = DIRECTION ( 'NONE',  ( 1.734723475976806848E-16, -0.000000000000000000, 1.000000000000000000 ) ) ;
#41328 = PLANE ( 'NONE',  #5046 ) ;
#41329 = VECTOR ( 'NONE', #24439, 39.37007874015748143 ) ;
#41330 = DIRECTION ( 'NONE',  ( -0.000000000000000000, 0.000000000000000000, 1.000000000000000000 ) ) ;
#41331 = DIRECTION ( 'NONE',  ( -1.729310098865080642E-17, 1.000000000000000000, 1.276627980444840260E-16 ) ) ;
#41332 = EDGE_LOOP ( 'NONE', ( #1013, #28275, #36161, #1456 ) ) ;
#41333 = CARTESIAN_POINT ( 'NONE',  ( 1.548545842648739956, 1.732704746525083772, 1.697655184951773810 ) ) ;
#41334 = DIRECTION ( 'NONE',  ( -0.000000000000000000, 1.000000000000000000, -0.000000000000000000 ) ) ;
#41335 = ORIENTED_EDGE ( 'NONE', *, *, #14796, .T. ) ;
#41336 = EDGE_LOOP ( 'NONE', ( #8081, #23713, #37559, #12483 ) ) ;
#41337 = DIRECTION ( 'NONE',  ( -1.000000000000000000, 0.000000000000000000, 1.734723475976806848E-16 ) ) ;
#41338 = ORIENTED_EDGE ( 'NONE', *, *, #46744, .T. ) ;
#41339 = EDGE_LOOP ( 'NONE', ( #48389, #7145, #22628, #4570 ) ) ;
#41340 = CARTESIAN_POINT ( 'NONE',  ( -0.04921259842519689481, 0.000000000000000000, 1.742692369722729895 ) ) ;
#41341 = ORIENTED_EDGE ( 'NONE', *, *, #47657, .T. ) ;
#41342 = VECTOR ( 'NONE', #20025, 39.37007874015748143 ) ;
#41343 = DIRECTION ( 'NONE',  ( -0.000000000000000000, -1.000000000000000000, -0.000000000000000000 ) ) ;
#41344 = CARTESIAN_POINT ( 'NONE',  ( -2.106299212598425008, 3.346456692913386100, -6.146657985744592735E-16 ) ) ;
#41345 = ORIENTED_EDGE ( 'NONE', *, *, #13281, .F. ) ;
#41346 = ADVANCED_FACE ( 'NONE', ( #14713 ), #14460, .F. ) ;
#41347 = ORIENTED_EDGE ( 'NONE', *, *, #50333, .T. ) ;
#41348 = VECTOR ( 'NONE', #24901, 39.37007874015748143 ) ;
#41349 = CARTESIAN_POINT ( 'NONE',  ( 2.378961647330872786, 0.000000000000000000, 0.6299212598425161236 ) ) ;
#41350 = EDGE_CURVE ( 'NONE', #46637, #45913, #14965, .T. ) ;
#41351 = ORIENTED_EDGE ( 'NONE', *, *, #6030, .T. ) ;
#41352 = VERTEX_POINT ( 'NONE', #7224 ) ;
#41353 = LINE ( 'NONE', #14232, #1757 ) ;
#41354 = CARTESIAN_POINT ( 'NONE',  ( 1.900276455977023549, 1.738338356005314722, -1.313328886422038710 ) ) ;
#41355 = AXIS2_PLACEMENT_3D ( 'NONE', #20259, #40659, #387 ) ;
#41356 = CARTESIAN_POINT ( 'NONE',  ( 2.164658444855302122, 5.905511811023623991, -0.04795272066889885720 ) ) ;
#41357 = EDGE_CURVE ( 'NONE', #45206, #14060, #22963, .T. ) ;
#41358 = AXIS2_PLACEMENT_3D ( 'NONE', #40630, #9384, #37021 ) ;
#41359 = ORIENTED_EDGE ( 'NONE', *, *, #5253, .F. ) ;
#41360 = CARTESIAN_POINT ( 'NONE',  ( 1.232995795418176943, 5.905511811023623991, 1.780798594093568221 ) ) ;
#41361 = PLANE ( 'NONE',  #48000 ) ;
#41362 = DIRECTION ( 'NONE',  ( -3.469446951953613696E-16, 0.000000000000000000, -1.000000000000000000 ) ) ;
#41363 = EDGE_LOOP ( 'NONE', ( #41948, #10912, #13916, #20919 ) ) ;
#41364 = CARTESIAN_POINT ( 'NONE',  ( -2.307846990702095535, 5.118110236220475784, -0.8016101313716829102 ) ) ;
#41365 = FACE_OUTER_BOUND ( 'NONE', #25623, .T. ) ;
#41366 = LINE ( 'NONE', #17871, #24136 ) ;
#41367 = ORIENTED_EDGE ( 'NONE', *, *, #47753, .F. ) ;
#41368 = EDGE_LOOP ( 'NONE', ( #6179, #6913, #6592, #41063 ) ) ;
#41369 = LENGTH_MEASURE_WITH_UNIT ( LENGTH_MEASURE( 0.02539999999999999897 ), #26126 );
#41370 = CARTESIAN_POINT ( 'NONE',  ( 0.1968503937007877735, 0.000000000000000000, 1.377952755905504256 ) ) ;
#41371 = EDGE_CURVE ( 'NONE', #27812, #45405, #15212, .T. ) ;
#41372 = LINE ( 'NONE', #21241, #27774 ) ;
#41373 = CARTESIAN_POINT ( 'NONE',  ( -1.181102362204724310, 0.000000000000000000, -1.181102362204724754 ) ) ;
#41374 = ORIENTED_EDGE ( 'NONE', *, *, #32399, .F. ) ;
#41375 = ORIENTED_EDGE ( 'NONE', *, *, #26098, .T. ) ;
#41376 = EDGE_CURVE ( 'NONE', #9179, #28139, #47427, .T. ) ;
#41377 = CARTESIAN_POINT ( 'NONE',  ( -0.4424051356154121706, 0.01394701979125833637, -1.788003152444398225 ) ) ;
#41378 = ORIENTED_EDGE ( 'NONE', *, *, #24290, .T. ) ;
#41379 = CARTESIAN_POINT ( 'NONE',  ( 0.000000000000000000, 0.000000000000000000, -0.8858267716535433989 ) ) ;
#41380 = CARTESIAN_POINT ( 'NONE',  ( 2.099568260077707027, 2.755905511811027164, -0.5296909464895783737 ) ) ;
#41381 = VECTOR ( 'NONE', #49845, 39.37007874015748143 ) ;
#41382 = VECTOR ( 'NONE', #15511, 39.37007874015748143 ) ;
#41383 = CARTESIAN_POINT ( 'NONE',  ( 2.326943258702977246, 1.646747008850265370, -0.05524094006260020506 ) ) ;
#41384 = FACE_OUTER_BOUND ( 'NONE', #2362, .T. ) ;
#41386 = LINE ( 'NONE', #6011, #1518 ) ;
#41385 = CIRCLE ( 'NONE', #43863, 2.165354330708661568 ) ;
#41387 = ORIENTED_EDGE ( 'NONE', *, *, #41995, .F. ) ;
#41388 = DIRECTION ( 'NONE',  ( 1.000000000000000000, 0.000000000000000000, 0.000000000000000000 ) ) ;
#41389 = DIRECTION ( 'NONE',  ( 1.000000000000000000, 0.000000000000000000, 0.000000000000000000 ) ) ;
#41390 = VECTOR ( 'NONE', #49440, 39.37007874015748143 ) ;
#41391 = DIRECTION ( 'NONE',  ( 3.986037398843765983E-20, 1.000000000000000000, 1.160734090543304660E-16 ) ) ;
#41392 = ORIENTED_EDGE ( 'NONE', *, *, #13556, .T. ) ;
#41393 = VECTOR ( 'NONE', #50980, 39.37007874015748143 ) ;
#41394 = CARTESIAN_POINT ( 'NONE',  ( -1.613340714851948965, 1.583636149837539975, -1.474425128113891814 ) ) ;
#41395 = CARTESIAN_POINT ( 'NONE',  ( 1.461363083917469163, 6.692913385826772199, 1.597866488315585087 ) ) ;
#41396 = CARTESIAN_POINT ( 'NONE',  ( 0.000000000000000000, 1.595182601976580683, 0.000000000000000000 ) ) ;
#41397 = ORIENTED_EDGE ( 'NONE', *, *, #10841, .F. ) ;
#41398 = DIRECTION ( 'NONE',  ( 0.000000000000000000, 1.000000000000000000, 0.000000000000000000 ) ) ;
#41399 = CARTESIAN_POINT ( 'NONE',  ( 0.000000000000000000, 3.267716535433071279, 0.9448818897637749625 ) ) ;
#41400 = VERTEX_POINT ( 'NONE', #46672 ) ;
#41401 = DIRECTION ( 'NONE',  ( -0.000000000000000000, 1.000000000000000000, -0.000000000000000000 ) ) ;
#41402 = CARTESIAN_POINT ( 'NONE',  ( 2.867773316779195447, 1.205361022782829114E-17, -0.7050287376752006896 ) ) ;
#41403 = EDGE_LOOP ( 'NONE', ( #36582, #26108, #24181, #43126 ) ) ;
#41404 = DIRECTION ( 'NONE',  ( -0.9362348706397417564, 0.000000000000000000, 0.3513748240813304724 ) ) ;
#41405 = PLANE ( 'NONE',  #47348 ) ;
#41406 = DIRECTION ( 'NONE',  ( 1.000000000000000000, -0.000000000000000000, 0.000000000000000000 ) ) ;
#41407 = CARTESIAN_POINT ( 'NONE',  ( -1.171161938979115025, 1.656335251912683271, 1.864245081490210731 ) ) ;
#41408 = CARTESIAN_POINT ( 'NONE',  ( 0.2727639067037605503, 3.267716535433071279, -4.731699523581609741E-17 ) ) ;
#41409 = EDGE_CURVE ( 'NONE', #38085, #10739, #15715, .T. ) ;
#41410 = VERTEX_POINT ( 'NONE', #26825 ) ;
#41411 = ORIENTED_EDGE ( 'NONE', *, *, #51038, .T. ) ;
#41412 = CARTESIAN_POINT ( 'NONE',  ( -1.408960544533061299, 0.005352583808700523381, 1.060663264281380025 ) ) ;
#41413 = LINE ( 'NONE', #897, #19685 ) ;
#41414 = ADVANCED_FACE ( 'NONE', ( #35093 ), #50519, .F. ) ;
#41415 = VERTEX_POINT ( 'NONE', #4357 ) ;
#41416 = LINE ( 'NONE', #6042, #1996 ) ;
#41417 = CARTESIAN_POINT ( 'NONE',  ( -1.636583440222563635, 3.346456692913386100, 1.062992125984246083 ) ) ;
#41418 = CARTESIAN_POINT ( 'NONE',  ( 2.277873973731426194, 1.656288013650806912, 1.879489153247668076 ) ) ;
#41419 = EDGE_CURVE ( 'NONE', #22594, #15665, #6505, .T. ) ;
#41420 = ORIENTED_EDGE ( 'NONE', *, *, #11110, .F. ) ;
#41421 = AXIS2_PLACEMENT_3D ( 'NONE', #6698, #26809, #46161 ) ;
#41422 = ORIENTED_EDGE ( 'NONE', *, *, #41542, .F. ) ;
#41423 = DIRECTION ( 'NONE',  ( -0.9909497617679352555, 0.000000000000000000, 0.1342332658176522697 ) ) ;
#41424 = LINE ( 'NONE', #41180, #4373 ) ;
#41425 = DIRECTION ( 'NONE',  ( -0.000000000000000000, 1.000000000000000000, -0.000000000000000000 ) ) ;
#41426 = ADVANCED_FACE ( 'NONE', ( #15967 ), #23205, .T. ) ;
#41427 = ORIENTED_EDGE ( 'NONE', *, *, #18708, .T. ) ;
#41428 = CARTESIAN_POINT ( 'NONE',  ( -1.909347346926324462, 3.267716535433071279, 3.312189666507127188E-16 ) ) ;
#41429 = CARTESIAN_POINT ( 'NONE',  ( -1.025452293874513199, 0.4479795140330847802, -1.038530695135447157 ) ) ;
#41430 = ORIENTED_EDGE ( 'NONE', *, *, #35573, .F. ) ;
#41431 = DIRECTION ( 'NONE',  ( 0.000000000000000000, -1.000000000000000000, 0.000000000000000000 ) ) ;
#41432 = EDGE_LOOP ( 'NONE', ( #49798, #5912, #13939, #5279 ) ) ;
#41433 = VECTOR ( 'NONE', #26745, 39.37007874015748143 ) ;
#41434 = ORIENTED_EDGE ( 'NONE', *, *, #13263, .F. ) ;
#41435 = DIRECTION ( 'NONE',  ( 0.000000000000000000, 0.000000000000000000, -1.000000000000000000 ) ) ;
#41436 = PLANE ( 'NONE',  #15978 ) ;
#41437 = VECTOR ( 'NONE', #48652, 39.37007874015748143 ) ;
#41438 = EDGE_CURVE ( 'NONE', #42820, #36594, #6808, .T. ) ;
#41439 = ORIENTED_EDGE ( 'NONE', *, *, #11541, .F. ) ;
#41440 = DIRECTION ( 'NONE',  ( 0.000000000000000000, 0.000000000000000000, 1.000000000000000000 ) ) ;
#41441 = PLANE ( 'NONE',  #1581 ) ;
#41442 = ORIENTED_EDGE ( 'NONE', *, *, #4473, .F. ) ;
#41443 = EDGE_CURVE ( 'NONE', #4205, #8227, #42822, .T. ) ;
#41444 = DIRECTION ( 'NONE',  ( 1.000000000000000000, 0.000000000000000000, 0.000000000000000000 ) ) ;
#41445 = FACE_OUTER_BOUND ( 'NONE', #28659, .T. ) ;
#41446 = ADVANCED_FACE ( 'NONE', ( #39211 ), #20084, .F. ) ;
#41447 = DIRECTION ( 'NONE',  ( -3.469446951953613696E-16, 0.000000000000000000, -1.000000000000000000 ) ) ;
#41448 = DIRECTION ( 'NONE',  ( -0.000000000000000000, 0.000000000000000000, 1.000000000000000000 ) ) ;
#41449 = DIRECTION ( 'NONE',  ( -0.4626380123495250074, 0.000000000000000000, 0.8865472742777346093 ) ) ;
#41450 = EDGE_LOOP ( 'NONE', ( #27340, #50759, #17830, #27015 ) ) ;
#41451 = DIRECTION ( 'NONE',  ( 0.000000000000000000, 0.000000000000000000, -1.000000000000000000 ) ) ;
#41452 = B_SPLINE_CURVE_WITH_KNOTS ( 'NONE', 3,
 ( #1633, #44986, #41143, #33653 ),
 .UNSPECIFIED., .F., .F.,
 ( 4, 4 ),
 ( 2.330467837939416791E-07, 0.01688764880552376044 ),
 .UNSPECIFIED. ) ;
#41453 = EDGE_CURVE ( 'NONE', #31299, #27036, #11589, .T. ) ;
#41454 = DIRECTION ( 'NONE',  ( -1.000000000000000000, -0.000000000000000000, -0.000000000000000000 ) ) ;
#41455 = ORIENTED_EDGE ( 'NONE', *, *, #1693, .T. ) ;
#41456 = VECTOR ( 'NONE', #31971, 39.37007874015748143 ) ;
#41457 = DIRECTION ( 'NONE',  ( -3.469446951953613696E-16, 0.000000000000000000, -1.000000000000000000 ) ) ;
#41458 = CARTESIAN_POINT ( 'NONE',  ( -1.909347346926324462, 3.346456692913386100, 1.102362204724404160 ) ) ;
#41459 = ORIENTED_EDGE ( 'NONE', *, *, #5112, .T. ) ;
#41460 = LINE ( 'NONE', #18219, #37841 ) ;
#41461 = DIRECTION ( 'NONE',  ( -0.000000000000000000, 1.000000000000000000, -0.000000000000000000 ) ) ;
#41462 = LINE ( 'NONE', #36835, #36745 ) ;
#41463 = VECTOR ( 'NONE', #9164, 39.37007874015748143 ) ;
#41464 = ORIENTED_EDGE ( 'NONE', *, *, #12782, .T. ) ;
#41465 = AXIS2_PLACEMENT_3D ( 'NONE', #29742, #21489, #13999 ) ;
#41466 = LINE ( 'NONE', #10225, #40365 ) ;
#41467 = VERTEX_POINT ( 'NONE', #43067 ) ;
#41468 = FACE_BOUND ( 'NONE', #18031, .T. ) ;
#41469 = FACE_OUTER_BOUND ( 'NONE', #1734, .T. ) ;
#41470 = VECTOR ( 'NONE', #29951, 39.37007874015748143 ) ;
#41471 = FACE_OUTER_BOUND ( 'NONE', #1647, .T. ) ;
#41472 = CARTESIAN_POINT ( 'NONE',  ( 0.6584127755596609344, 0.000000000000000000, 1.614277297217986851 ) ) ;
#41473 = ORIENTED_EDGE ( 'NONE', *, *, #7848, .F. ) ;
#41474 = ORIENTED_EDGE ( 'NONE', *, *, #22635, .T. ) ;
#41475 = CARTESIAN_POINT ( 'NONE',  ( -1.195183497228115035E-16, 3.346456692913386100, -1.259842519685035134 ) ) ;
#41476 = EDGE_LOOP ( 'NONE', ( #10023, #52, #27547, #6725 ) ) ;
#41477 = CARTESIAN_POINT ( 'NONE',  ( -2.919165122154194769, 1.575328909575085090, 0.4450898352768660748 ) ) ;
#41478 = ORIENTED_EDGE ( 'NONE', *, *, #27587, .F. ) ;
#41479 = EDGE_CURVE ( 'NONE', #472, #187, #3850, .T. ) ;
#41480 = CARTESIAN_POINT ( 'NONE',  ( 0.2727639067037604947, 0.000000000000000000, 0.4724409448818868706 ) ) ;
#41481 = EDGE_CURVE ( 'NONE', #16704, #9041, #35348, .T. ) ;
#41482 = EDGE_LOOP ( 'NONE', ( #490, #2975, #49886, #35516 ) ) ;
#41483 = CARTESIAN_POINT ( 'NONE',  ( -2.932638728931780125, 1.673548413681422042, 0.3475908556737793420 ) ) ;
#41484 = EDGE_CURVE ( 'NONE', #43099, #14557, #31470, .T. ) ;
#41485 = LINE ( 'NONE', #42492, #19866 ) ;
#41486 = ORIENTED_EDGE ( 'NONE', *, *, #17507, .F. ) ;
#41487 = CARTESIAN_POINT ( 'NONE',  ( -1.172858943013144861, -2.300834904144050480E-16, 1.867085387823100628 ) ) ;
#41488 = ORIENTED_EDGE ( 'NONE', *, *, #13972, .T. ) ;
#41489 = ORIENTED_EDGE ( 'NONE', *, *, #30790, .F. ) ;
#41490 = ORIENTED_EDGE ( 'NONE', *, *, #9534, .F. ) ;
#41491 = ORIENTED_EDGE ( 'NONE', *, *, #19946, .T. ) ;
#41492 = CARTESIAN_POINT ( 'NONE',  ( -0.2492758785930729581, 1.703909341437327862, -2.220674960591680680 ) ) ;
#41493 = AXIS2_PLACEMENT_3D ( 'NONE', #5735, #25353, #25104 ) ;
#41494 = VERTEX_POINT ( 'NONE', #43327 ) ;
#41495 = CIRCLE ( 'NONE', #3569, 2.164630168518208109 ) ;
#41496 = CARTESIAN_POINT ( 'NONE',  ( -1.166969139818016865, 3.267716535433071279, 4.048737525165548620E-16 ) ) ;
#41497 = CARTESIAN_POINT ( 'NONE',  ( 1.306035350298335729, 1.696012099853481336, -1.881328916909827065 ) ) ;
#41498 = AXIS2_PLACEMENT_3D ( 'NONE', #42870, #30761, #18887 ) ;
#41499 = VECTOR ( 'NONE', #2080, 39.37007874015748143 ) ;
#41500 = EDGE_CURVE ( 'NONE', #18533, #35538, #7971, .T. ) ;
#41501 = CARTESIAN_POINT ( 'NONE',  ( 0.1968503937007873017, 3.267716535433071279, -0.6299212598425177889 ) ) ;
#41502 = ORIENTED_EDGE ( 'NONE', *, *, #30868, .F. ) ;
#41503 = PLANE ( 'NONE',  #40129 ) ;
#41504 = CARTESIAN_POINT ( 'NONE',  ( 0.7423782071083087075, 3.346456692913386100, 0.9448818897637746295 ) ) ;
#41505 = AXIS2_PLACEMENT_3D ( 'NONE', #26892, #2905, #18907 ) ;
#41506 = ORIENTED_EDGE ( 'NONE', *, *, #32040, .T. ) ;
#41507 = CARTESIAN_POINT ( 'NONE',  ( 0.8182917201112817063, 3.267716535433071279, -1.732283464566923614 ) ) ;
#41508 = CARTESIAN_POINT ( 'NONE',  ( -1.712496953225537633, 0.000000000000000000, -0.7874015748031470974 ) ) ;
#41509 = CARTESIAN_POINT ( 'NONE',  ( 2.742591780645512234, 1.758546389883244965, -0.07390773670709777088 ) ) ;
#41510 = EDGE_CURVE ( 'NONE', #40324, #8605, #24490, .T. ) ;
#41511 = CARTESIAN_POINT ( 'NONE',  ( 1.833433833923351353, 3.346456692913386100, -0.3149606299212596716 ) ) ;
#41512 = LINE ( 'NONE', #6404, #30110 ) ;
#41513 = FACE_OUTER_BOUND ( 'NONE', #41855, .T. ) ;
#41514 = VERTEX_POINT ( 'NONE', #20866 ) ;
#41515 = CARTESIAN_POINT ( 'NONE',  ( -0.5455278134075208785, 0.000000000000000000, 0.7480314960629874665 ) ) ;
#41516 = EDGE_CURVE ( 'NONE', #38951, #39747, #29582, .T. ) ;
#41517 = CARTESIAN_POINT ( 'NONE',  ( 0.000000000000000000, 3.267716535433071279, 0.000000000000000000 ) ) ;
#41518 = ORIENTED_EDGE ( 'NONE', *, *, #20324, .F. ) ;
#41519 = LINE ( 'NONE', #15102, #43215 ) ;
#41520 = EDGE_CURVE ( 'NONE', #50367, #39693, #25251, .T. ) ;
#41521 = VERTEX_POINT ( 'NONE', #24995 ) ;
#41522 = CARTESIAN_POINT ( 'NONE',  ( 1.560669927219590525, 3.267716535433071279, -0.6692913385826764205 ) ) ;
#41523 = EDGE_CURVE ( 'NONE', #19504, #22619, #4611, .T. ) ;
#41524 = DIRECTION ( 'NONE',  ( 1.734723475976806848E-16, -0.000000000000000000, 1.000000000000000000 ) ) ;
#41525 = CARTESIAN_POINT ( 'NONE',  ( -1.712496953225537633, 3.267716535433071279, 1.226315847645293999 ) ) ;
#41526 = CARTESIAN_POINT ( 'NONE',  ( -2.165460538733998241, 1.205361022782829114E-17, 0.04798874274652762534 ) ) ;
#41527 = DIRECTION ( 'NONE',  ( -3.469446951953613696E-16, 0.000000000000000000, -1.000000000000000000 ) ) ;
#41528 = EDGE_LOOP ( 'NONE', ( #38842, #18558, #45073, #45937 ) ) ;
#41529 = LINE ( 'NONE', #10289, #6742 ) ;
#41530 = ORIENTED_EDGE ( 'NONE', *, *, #34662, .T. ) ;
#41531 = ORIENTED_EDGE ( 'NONE', *, *, #47984, .F. ) ;
#41532 = DIRECTION ( 'NONE',  ( -3.469446951953613696E-16, 0.000000000000000000, -1.000000000000000000 ) ) ;
#41533 = ORIENTED_EDGE ( 'NONE', *, *, #9125, .T. ) ;
#41534 = DIRECTION ( 'NONE',  ( -0.000000000000000000, 1.000000000000000000, -0.000000000000000000 ) ) ;
#41535 = DIRECTION ( 'NONE',  ( 1.000000000000000000, 0.000000000000000000, 0.000000000000000000 ) ) ;
#41536 = VERTEX_POINT ( 'NONE', #36879 ) ;
#41537 = AXIS2_PLACEMENT_3D ( 'NONE', #43999, #47842, #899 ) ;
#41538 = EDGE_CURVE ( 'NONE', #16952, #23409, #24744, .T. ) ;
#41539 = CONICAL_SURFACE ( 'NONE', #13496, 3.483074324928249421, 1.244861948955335196 ) ;
#41540 = CARTESIAN_POINT ( 'NONE',  ( -0.2834077913992259501, 2.755905511811024056, -0.2440651625074179987 ) ) ;
#41541 = DIRECTION ( 'NONE',  ( 0.000000000000000000, -1.000000000000000000, 0.000000000000000000 ) ) ;
#41542 = EDGE_CURVE ( 'NONE', #28842, #49676, #32501, .T. ) ;
#41543 = EDGE_CURVE ( 'NONE', #48519, #48829, #40493, .T. ) ;
#41544 = CARTESIAN_POINT ( 'NONE',  ( -1.909347346926324906, 3.267716535433071279, -0.6692913385826758654 ) ) ;
#41545 = EDGE_CURVE ( 'NONE', #38459, #42332, #32764, .T. ) ;
#41546 = ORIENTED_EDGE ( 'NONE', *, *, #35228, .T. ) ;
#41547 = ORIENTED_EDGE ( 'NONE', *, *, #43186, .F. ) ;
#41548 = PLANE ( 'NONE',  #38087 ) ;
#41549 = FACE_BOUND ( 'NONE', #44056, .T. ) ;
#41550 = EDGE_LOOP ( 'NONE', ( #24094, #42476, #26499, #18003 ) ) ;
#41551 = DIRECTION ( 'NONE',  ( 0.7818314824680221431, 0.000000000000000000, 0.6234898018587431423 ) ) ;
#41552 = CARTESIAN_POINT ( 'NONE',  ( 0.000000000000000000, 3.267716535433071279, -1.259842519685035800 ) ) ;
#41553 = EDGE_LOOP ( 'NONE', ( #30995, #50255 ) ) ;
#41554 = ORIENTED_EDGE ( 'NONE', *, *, #34505, .F. ) ;
#41555 = CARTESIAN_POINT ( 'NONE',  ( -0.5373920265435009336, 0.5242596937404421231, -2.132180421997459607 ) ) ;
#41556 = DIRECTION ( 'NONE',  ( 1.000000000000000000, 0.000000000000000000, 0.000000000000000000 ) ) ;
#41557 = VERTEX_POINT ( 'NONE', #8485 ) ;
#41558 = EDGE_LOOP ( 'NONE', ( #24732, #28494, #6085, #21427, #18977, #32060, #37908, #36983, #10746, #41345, #6951, #16594, #7480 ) ) ;
#41559 = VERTEX_POINT ( 'NONE', #48694 ) ;
#41560 = CARTESIAN_POINT ( 'NONE',  ( -1.439733046521776139, 3.267716535433071279, 4.995077429881866871E-16 ) ) ;
#41561 = CARTESIAN_POINT ( 'NONE',  ( -2.721590468760166193, 1.571075366034202947, -1.145417842932506147 ) ) ;
#41562 = CARTESIAN_POINT ( 'NONE',  ( 1.560669927219590747, 0.000000000000000000, 1.417322834645662777 ) ) ;
#41563 = EDGE_CURVE ( 'NONE', #20029, #33804, #16031, .T. ) ;
#41564 = DIRECTION ( 'NONE',  ( -0.9998717552508121775, -0.01601477604151182663, 0.000000000000000000 ) ) ;
#41565 = ORIENTED_EDGE ( 'NONE', *, *, #38901, .T. ) ;
#41566 = ORIENTED_EDGE ( 'NONE', *, *, #39082, .F. ) ;
#41567 = VECTOR ( 'NONE', #20539, 39.37007874015748143 ) ;
#41568 = CARTESIAN_POINT ( 'NONE',  ( 1.287906020515830141, 0.000000000000000000, -0.6299212598425181220 ) ) ;
#41569 = CARTESIAN_POINT ( 'NONE',  ( -0.3382312733057311060, 1.205361022782829114E-17, -2.139420919314970693 ) ) ;
#41570 = AXIS2_PLACEMENT_3D ( 'NONE', #31273, #27375, #35904 ) ;
#41571 = CARTESIAN_POINT ( 'NONE',  ( -0.8942052331142552601, 0.000000000000000000, -0.8267716535433052849 ) ) ;
#41572 = AXIS2_PLACEMENT_3D ( 'NONE', #24192, #24956, #5078 ) ;
#41573 = DIRECTION ( 'NONE',  ( 0.000000000000000000, 0.000000000000000000, -1.000000000000000000 ) ) ;
#41574 = EDGE_CURVE ( 'NONE', #23260, #33703, #36349, .T. ) ;
#41575 = AXIS2_PLACEMENT_3D ( 'NONE', #13524, #40891, #29526 ) ;
#41576 = CARTESIAN_POINT ( 'NONE',  ( -0.5440951526915226433, 1.699187271209207983, -2.156468654116168171 ) ) ;
#41577 = VECTOR ( 'NONE', #8549, 39.37007874015748143 ) ;
#41578 = ADVANCED_FACE ( 'NONE', ( #20612 ), #40748, .F. ) ;
#41579 = DIRECTION ( 'NONE',  ( 0.000000000000000000, -1.000000000000000000, 0.000000000000000000 ) ) ;
#41580 = EDGE_CURVE ( 'NONE', #33697, #37057, #45548, .T. ) ;
#41581 = LINE ( 'NONE', #18338, #26713 ) ;
#41582 = VECTOR ( 'NONE', #27468, 39.37007874015748143 ) ;
#41583 = ORIENTED_EDGE ( 'NONE', *, *, #27388, .F. ) ;
#41584 = DIRECTION ( 'NONE',  ( -0.000000000000000000, 1.000000000000000000, -0.000000000000000000 ) ) ;
#41585 = FACE_OUTER_BOUND ( 'NONE', #8260, .T. ) ;
#41586 = ORIENTED_EDGE ( 'NONE', *, *, #2888, .F. ) ;
#41587 = EDGE_LOOP ( 'NONE', ( #49356, #39051, #17081, #10389 ) ) ;
#41588 = CARTESIAN_POINT ( 'NONE',  ( 1.574803149606299080, 1.172985819482486924, -4.133858267716535195 ) ) ;
#41589 = ORIENTED_EDGE ( 'NONE', *, *, #45563, .T. ) ;
#41590 = EDGE_CURVE ( 'NONE', #2069, #12621, #9503, .T. ) ;
#41591 = B_SPLINE_CURVE_WITH_KNOTS ( 'NONE', 3,
 ( #9121, #1376, #14016, #48577 ),
 .UNSPECIFIED., .F., .F.,
 ( 4, 4 ),
 ( 0.1211775127643062860, 0.1625894504277921315 ),
 .UNSPECIFIED. ) ;
#41592 = ORIENTED_EDGE ( 'NONE', *, *, #32460, .T. ) ;
#41593 = CARTESIAN_POINT ( 'NONE',  ( 2.106197740627112402, 3.346456692913386100, -0.02067487291359444701 ) ) ;
#41594 = EDGE_CURVE ( 'NONE', #20385, #47699, #36110, .T. ) ;
#41595 = ORIENTED_EDGE ( 'NONE', *, *, #40978, .F. ) ;
#41596 = CARTESIAN_POINT ( 'NONE',  ( 0.000000000000000000, 2.344748451760389596, 0.000000000000000000 ) ) ;
#41597 = DIRECTION ( 'NONE',  ( -0.000000000000000000, 1.000000000000000000, -0.000000000000000000 ) ) ;
#41598 = EDGE_CURVE ( 'NONE', #32620, #7484, #47937, .T. ) ;
#41599 = EDGE_LOOP ( 'NONE', ( #50858, #26847, #7050, #7734 ) ) ;
#41600 = ORIENTED_EDGE ( 'NONE', *, *, #7765, .T. ) ;
#41601 = B_SPLINE_CURVE_WITH_KNOTS ( 'NONE', 3,
 ( #7997, #35628, #30742, #39498 ),
 .UNSPECIFIED., .F., .F.,
 ( 4, 4 ),
 ( 0.04362072447804023201, 0.06160699411348036225 ),
 .UNSPECIFIED. ) ;
#41602 = PLANE ( 'NONE',  #46926 ) ;
#41603 = AXIS2_PLACEMENT_3D ( 'NONE', #50398, #50644, #15342 ) ;
#41605 = VERTEX_POINT ( 'NONE', #12356 ) ;
#41604 = ADVANCED_FACE ( 'NONE', ( #4868 ), #31989, .T. ) ;
#41606 = ORIENTED_EDGE ( 'NONE', *, *, #43979, .T. ) ;
#41607 = DIRECTION ( 'NONE',  ( 0.000000000000000000, 1.000000000000000000, 0.000000000000000000 ) ) ;
#41608 = CARTESIAN_POINT ( 'NONE',  ( -2.258024766633058622, 3.267716535433071279, -0.3543307086614173040 ) ) ;
#41609 = PLANE ( 'NONE',  #30264 ) ;
#41610 = AXIS2_PLACEMENT_3D ( 'NONE', #22168, #13397, #33798 ) ;
#41611 = VECTOR ( 'NONE', #49722, 39.37007874015748143 ) ;
#41612 = B_SPLINE_CURVE_WITH_KNOTS ( 'NONE', 3,
 ( #6954, #23444, #42816, #11832 ),
 .UNSPECIFIED., .F., .F.,
 ( 4, 4 ),
 ( 2.766355543619157244E-07, 0.002500607986718841793 ),
 .UNSPECIFIED. ) ;
#41613 = VERTEX_POINT ( 'NONE', #28089 ) ;
#41614 = DIRECTION ( 'NONE',  ( 1.000000000000000000, 0.000000000000000000, -3.469446951953613696E-16 ) ) ;
#41615 = DIRECTION ( 'NONE',  ( 0.000000000000000000, -1.000000000000000000, 0.000000000000000000 ) ) ;
#41616 = DIRECTION ( 'NONE',  ( 0.000000000000000000, -1.000000000000000000, -0.000000000000000000 ) ) ;
#41617 = VERTEX_POINT ( 'NONE', #43834 ) ;
#41618 = CARTESIAN_POINT ( 'NONE',  ( 0.1968503937007878291, 3.346456692913386100, 2.097080421798980687 ) ) ;
#41619 = CARTESIAN_POINT ( 'NONE',  ( 2.106197740627111514, 3.346456692913386100, -0.9842519685039348154 ) ) ;
#41620 = VECTOR ( 'NONE', #23013, 39.37007874015748143 ) ;
#41621 = DIRECTION ( 'NONE',  ( -3.469446951953613696E-16, 0.000000000000000000, -1.000000000000000000 ) ) ;
#41622 = ORIENTED_EDGE ( 'NONE', *, *, #41294, .F. ) ;
#41623 = ORIENTED_EDGE ( 'NONE', *, *, #13449, .T. ) ;
#41624 = SHAPE_REPRESENTATION_RELATIONSHIP ( 'NONE' , 'NONE' ,  #34429, #31011 ) ;
#41625 = CARTESIAN_POINT ( 'NONE',  ( 0.3546377434558362074, 1.615156926475952881, 2.229828021450985798 ) ) ;
#41626 = CARTESIAN_POINT ( 'NONE',  ( 2.043634885149959501, 1.574803149606302854, 0.7157624142946232837 ) ) ;
#41627 = CARTESIAN_POINT ( 'NONE',  ( 0.7516222819726512405, 1.687132160473688636, 2.142747677857361310 ) ) ;
#41628 = ORIENTED_EDGE ( 'NONE', *, *, #19843, .F. ) ;
#41629 = ORIENTED_EDGE ( 'NONE', *, *, #47296, .T. ) ;
#41630 = LINE ( 'NONE', #18137, #47303 ) ;
#41631 = ORIENTED_EDGE ( 'NONE', *, *, #28592, .T. ) ;
#41632 = DIRECTION ( 'NONE',  ( -3.469446951953613696E-16, 0.000000000000000000, -1.000000000000000000 ) ) ;
#41633 = DIRECTION ( 'NONE',  ( 1.734723475976806848E-16, -0.000000000000000000, 1.000000000000000000 ) ) ;
#41634 = EDGE_CURVE ( 'NONE', #15854, #17057, #41260, .T. ) ;
#41635 = DIRECTION ( 'NONE',  ( 1.000000000000000000, 0.000000000000000000, 0.000000000000000000 ) ) ;
#41636 = EDGE_CURVE ( 'NONE', #10110, #40291, #14390, .T. ) ;
#41637 = CARTESIAN_POINT ( 'NONE',  ( 0.2727639067037602172, 0.000000000000000000, -2.047244094488182231 ) ) ;
#41638 = DIRECTION ( 'NONE',  ( -0.000000000000000000, 1.000000000000000000, -0.000000000000000000 ) ) ;
#41639 = ORIENTED_EDGE ( 'NONE', *, *, #45617, .F. ) ;
#41640 = AXIS2_PLACEMENT_3D ( 'NONE', #9058, #1570, #13956 ) ;
#41641 = EDGE_CURVE ( 'NONE', #24717, #45399, #21885, .T. ) ;
#41642 = CARTESIAN_POINT ( 'NONE',  ( -1.439733046521776583, 3.346456692913386100, -0.6299212598425177889 ) ) ;
#41643 = DIRECTION ( 'NONE',  ( 1.734723475976806848E-16, 0.000000000000000000, 1.000000000000000000 ) ) ;
#41644 = VECTOR ( 'NONE', #39985, 39.37007874015748143 ) ;
#41645 = LINE ( 'NONE', #26149, #42186 ) ;
#41646 = CIRCLE ( 'NONE', #7001, 2.246510896728926010 ) ;
#41647 = ORIENTED_EDGE ( 'NONE', *, *, #34571, .F. ) ;
#41648 = LINE ( 'NONE', #3412, #13356 ) ;
#41649 = DIRECTION ( 'NONE',  ( -1.288287287306305283E-16, 1.000000000000000000, 0.000000000000000000 ) ) ;
#41650 = DIRECTION ( 'NONE',  ( 0.000000000000000000, 0.000000000000000000, 1.000000000000000000 ) ) ;
#41651 = ORIENTED_EDGE ( 'NONE', *, *, #29575, .T. ) ;
#41652 = CARTESIAN_POINT ( 'NONE',  ( -0.8182917201112819283, 3.267716535433071279, -0.6692913385826760875 ) ) ;
#41653 = VECTOR ( 'NONE', #14614, 39.37007874015748143 ) ;
#41654 = ORIENTED_EDGE ( 'NONE', *, *, #45617, .T. ) ;
#41655 = PLANE ( 'NONE',  #5717 ) ;
#41656 = LINE ( 'NONE', #29266, #9292 ) ;
#41658 = ORIENTED_EDGE ( 'NONE', *, *, #28715, .F. ) ;
#41657 = ADVANCED_FACE ( 'NONE', ( #6649 ), #26508, .T. ) ;
#41659 = DIRECTION ( 'NONE',  ( -3.469446951953613696E-16, 0.000000000000000000, -1.000000000000000000 ) ) ;
#41660 = CARTESIAN_POINT ( 'NONE',  ( 1.560669927219590303, 0.000000000000000000, -1.732283464566923170 ) ) ;
#41661 = ADVANCED_FACE ( 'NONE', ( #29377 ), #1445, .F. ) ;
#41662 = CARTESIAN_POINT ( 'NONE',  ( 0.000000000000000000, 2.755905511811024056, 0.000000000000000000 ) ) ;
#41663 = PLANE ( 'NONE',  #39172 ) ;
#41664 = ORIENTED_EDGE ( 'NONE', *, *, #23854, .T. ) ;
#41665 = ORIENTED_EDGE ( 'NONE', *, *, #43252, .T. ) ;
#41666 = CARTESIAN_POINT ( 'NONE',  ( -1.091055626815042645, 3.346456692913386100, -1.574803149606293529 ) ) ;
#41667 = DIRECTION ( 'NONE',  ( -0.5407162030609373726, -0.6444004775717706579, 0.5407162030609373726 ) ) ;
#41668 = EDGE_CURVE ( 'NONE', #37443, #17837, #37391, .T. ) ;
#41669 = ORIENTED_EDGE ( 'NONE', *, *, #1883, .F. ) ;
#41670 = DIRECTION ( 'NONE',  ( 1.000000000000000000, 0.000000000000000000, 0.000000000000000000 ) ) ;
#41671 = LINE ( 'NONE', #17163, #40952 ) ;
#41672 = CARTESIAN_POINT ( 'NONE',  ( 0.8182917201112819283, 0.000000000000000000, -0.4724409448818889246 ) ) ;
#41673 = ADVANCED_FACE ( 'NONE', ( #2770 ), #22143, .F. ) ;
#41674 = ORIENTED_EDGE ( 'NONE', *, *, #16731, .F. ) ;
#41675 = ORIENTED_EDGE ( 'NONE', *, *, #42368, .F. ) ;
#41676 = LINE ( 'NONE', #6312, #36187 ) ;
#41677 = PLANE ( 'NONE',  #34855 ) ;
#41678 = CARTESIAN_POINT ( 'NONE',  ( 0.9845150457423212931, 0.000000000000000000, -1.438794182654551390 ) ) ;
#41679 = ORIENTED_EDGE ( 'NONE', *, *, #43858, .F. ) ;
#41680 = CARTESIAN_POINT ( 'NONE',  ( 1.091055626815042645, 3.267716535433071279, -0.1968503937007883287 ) ) ;
#41681 = LINE ( 'NONE', #29806, #5456 ) ;
#41682 = VECTOR ( 'NONE', #34777, 39.37007874015748143 ) ;
#41683 = ORIENTED_EDGE ( 'NONE', *, *, #43640, .F. ) ;
#41684 = AXIS2_PLACEMENT_3D ( 'NONE', #7255, #30495, #34621 ) ;
#41685 = DIRECTION ( 'NONE',  ( 1.000000000000000000, -0.000000000000000000, 0.000000000000000000 ) ) ;
#41686 = ORIENTED_EDGE ( 'NONE', *, *, #4852, .T. ) ;
#41687 = VERTEX_POINT ( 'NONE', #38152 ) ;
#41688 = LINE ( 'NONE', #18705, #16356 ) ;
#41689 = DIRECTION ( 'NONE',  ( 1.000000000000000000, 0.000000000000000000, 0.000000000000000000 ) ) ;
#41690 = VECTOR ( 'NONE', #32592, 39.37007874015748143 ) ;
#41691 = CARTESIAN_POINT ( 'NONE',  ( -0.7832715154832613491, 2.755905511811024056, 0.8840183951921659622 ) ) ;
#41692 = VECTOR ( 'NONE', #14571, 39.37007874015748854 ) ;
#41693 = ORIENTED_EDGE ( 'NONE', *, *, #45268, .T. ) ;
#41694 = DIRECTION ( 'NONE',  ( 0.9839295885986321100, 1.288287287306305037E-16, -0.1785568947986229116 ) ) ;
#41695 = FACE_OUTER_BOUND ( 'NONE', #45088, .T. ) ;
#41696 = EDGE_LOOP ( 'NONE', ( #27687, #1134, #21419, #16289 ) ) ;
#41697 = CIRCLE ( 'NONE', #37612, 2.165354330708661568 ) ;
#41698 = ORIENTED_EDGE ( 'NONE', *, *, #20496, .F. ) ;
#41699 = CARTESIAN_POINT ( 'NONE',  ( 1.174087487603958202, -2.119814714969965171E-16, 1.869141625116386818 ) ) ;
#41700 = DIRECTION ( 'NONE',  ( -0.000000000000000000, 0.000000000000000000, 1.000000000000000000 ) ) ;
#41701 = DIRECTION ( 'NONE',  ( -1.000000000000000000, 0.000000000000000000, -0.000000000000000000 ) ) ;
#41702 = EDGE_CURVE ( 'NONE', #36271, #23504, #12939, .T. ) ;
#41703 = DIRECTION ( 'NONE',  ( -1.000000000000000000, 0.000000000000000000, -0.000000000000000000 ) ) ;
#41704 = CARTESIAN_POINT ( 'NONE',  ( 0.000000000000000000, 0.000000000000000000, 0.000000000000000000 ) ) ;
#41705 = VERTEX_POINT ( 'NONE', #34021 ) ;
#41706 = EDGE_CURVE ( 'NONE', #45979, #24001, #10012, .T. ) ;
#41707 = CARTESIAN_POINT ( 'NONE',  ( 2.074049943651431693, 6.692913385826772199, 0.6221544894624241318 ) ) ;
#41708 = PLANE ( 'NONE',  #19070 ) ;
#41709 = ADVANCED_FACE ( 'NONE', ( #5878 ), #18261, .T. ) ;
#41710 = ORIENTED_EDGE ( 'NONE', *, *, #34010, .T. ) ;
#41711 = DIRECTION ( 'NONE',  ( 0.000000000000000000, 0.000000000000000000, -1.000000000000000000 ) ) ;
#41712 = CARTESIAN_POINT ( 'NONE',  ( -0.3486774197067340486, 3.267716535433071279, -0.5118110236220467790 ) ) ;
#41713 = VERTEX_POINT ( 'NONE', #25754 ) ;
#41714 = LINE ( 'NONE', #6351, #8965 ) ;
#41715 = EDGE_CURVE ( 'NONE', #8542, #3630, #45100, .T. ) ;
#41716 = DIRECTION ( 'NONE',  ( 1.000000000000000000, 0.000000000000000000, 0.000000000000000000 ) ) ;
#41717 = DIRECTION ( 'NONE',  ( 0.000000000000000000, 0.000000000000000000, 1.000000000000000000 ) ) ;
#41718 = VECTOR ( 'NONE', #32059, 39.37007874015748143 ) ;
#41719 = VECTOR ( 'NONE', #41717, 39.37007874015748143 ) ;
#41720 = VERTEX_POINT ( 'NONE', #6137 ) ;
#41721 = CARTESIAN_POINT ( 'NONE',  ( 0.000000000000000000, 3.267716535433071279, 1.102362204724403938 ) ) ;
#41722 = ORIENTED_EDGE ( 'NONE', *, *, #9689, .T. ) ;
#41723 = FACE_BOUND ( 'NONE', #37727, .T. ) ;
#41724 = AXIS2_PLACEMENT_3D ( 'NONE', #3874, #23481, #243 ) ;
#41725 = CARTESIAN_POINT ( 'NONE',  ( 0.08139965876239094178, 1.610780518492231694, 0.000000000000000000 ) ) ;
#41726 = CARTESIAN_POINT ( 'NONE',  ( 1.636583440222563635, 3.346456692913386100, -1.325930245594399537 ) ) ;
#41727 = EDGE_CURVE ( 'NONE', #50444, #42699, #49964, .T. ) ;
#41728 = CARTESIAN_POINT ( 'NONE',  ( 0.1968503937007873017, 3.346456692913386100, 0.3149606299212576177 ) ) ;
#41729 = AXIS2_PLACEMENT_3D ( 'NONE', #27187, #7331, #18945 ) ;
#41730 = VECTOR ( 'NONE', #2742, 39.37007874015748143 ) ;
#41731 = VERTEX_POINT ( 'NONE', #41504 ) ;
#41732 = ORIENTED_EDGE ( 'NONE', *, *, #49862, .T. ) ;
#41733 = DIRECTION ( 'NONE',  ( 0.000000000000000000, -1.000000000000000000, 0.000000000000000000 ) ) ;
#41734 = EDGE_CURVE ( 'NONE', #35545, #122, #37647, .T. ) ;
#41735 = DIRECTION ( 'NONE',  ( -0.9998717552508122886, -0.01601477604151180928, 0.000000000000000000 ) ) ;
#41736 = ORIENTED_EDGE ( 'NONE', *, *, #17940, .F. ) ;
#41737 = CARTESIAN_POINT ( 'NONE',  ( -1.428156070725274951, 1.693047415430531721, 2.294380806141768758 ) ) ;
#41738 = ORIENTED_EDGE ( 'NONE', *, *, #48780, .T. ) ;
#41739 = DIRECTION ( 'NONE',  ( 1.000000000000000000, 0.000000000000000000, 0.000000000000000000 ) ) ;
#41740 = DIRECTION ( 'NONE',  ( -0.000000000000000000, 1.000000000000000000, -0.000000000000000000 ) ) ;
#41741 = ORIENTED_EDGE ( 'NONE', *, *, #1851, .T. ) ;
#41742 = DIRECTION ( 'NONE',  ( -3.469446951953613696E-16, 0.000000000000000000, -1.000000000000000000 ) ) ;
#41743 = ORIENTED_EDGE ( 'NONE', *, *, #826, .T. ) ;
#41744 = ORIENTED_EDGE ( 'NONE', *, *, #24420, .F. ) ;
#41745 = EDGE_CURVE ( 'NONE', #13697, #14697, #18012, .T. ) ;
#41746 = ORIENTED_EDGE ( 'NONE', *, *, #5959, .F. ) ;
#41747 = ORIENTED_EDGE ( 'NONE', *, *, #5871, .F. ) ;
#41748 = CARTESIAN_POINT ( 'NONE',  ( 0.5905511811023627100, 0.000000000000000000, 0.000000000000000000 ) ) ;
#41749 = VECTOR ( 'NONE', #44925, 39.37007874015748854 ) ;
#41750 = VECTOR ( 'NONE', #11017, 39.37007874015748854 ) ;
#41751 = VERTEX_POINT ( 'NONE', #21383 ) ;
#41752 = CARTESIAN_POINT ( 'NONE',  ( 0.1968503937007873017, 3.346456692913386100, 0.6299212598425161236 ) ) ;
#41753 = AXIS2_PLACEMENT_3D ( 'NONE', #36980, #9859, #36724 ) ;
#41754 = FACE_OUTER_BOUND ( 'NONE', #46281, .T. ) ;
#41755 = AXIS2_PLACEMENT_3D ( 'NONE', #21058, #40935, #41440 ) ;
#41756 = CARTESIAN_POINT ( 'NONE',  ( -1.195183497228115035E-16, 0.000000000000000000, 0.3149606299212576177 ) ) ;
#41757 = VECTOR ( 'NONE', #32733, 39.37007874015748143 ) ;
#41758 = DIRECTION ( 'NONE',  ( 0.000000000000000000, 1.000000000000000000, 0.000000000000000000 ) ) ;
#41759 = CARTESIAN_POINT ( 'NONE',  ( -1.281152772984899713, 5.905511811023623991, -2.660341145381166506 ) ) ;
#41760 = ORIENTED_EDGE ( 'NONE', *, *, #49095, .T. ) ;
#41761 = EDGE_CURVE ( 'NONE', #22865, #7418, #37136, .T. ) ;
#41762 = CARTESIAN_POINT ( 'NONE',  ( 0.5344736634771639627, 1.625426382409501436, 2.669579653780858930 ) ) ;
#41763 = LINE ( 'NONE', #42016, #4418 ) ;
#41764 = CARTESIAN_POINT ( 'NONE',  ( 2.951990591674675368, 1.765258879000601855, -0.08331184815398361143 ) ) ;
#41765 = FACE_OUTER_BOUND ( 'NONE', #6235, .T. ) ;
#41766 = ADVANCED_FACE ( 'NONE', ( #1748 ), #4728, .T. ) ;
#41767 = VERTEX_POINT ( 'NONE', #13633 ) ;
#41768 = LINE ( 'NONE', #1758, #16593 ) ;
#41769 = EDGE_CURVE ( 'NONE', #3690, #50140, #47360, .T. ) ;
#41770 = CARTESIAN_POINT ( 'NONE',  ( -1.091055626815042645, 0.000000000000000000, -1.574803149606293529 ) ) ;
#41771 = ORIENTED_EDGE ( 'NONE', *, *, #47020, .F. ) ;
#41772 = LINE ( 'NONE', #49721, #707 ) ;
#41773 = EDGE_CURVE ( 'NONE', #4193, #25793, #3529, .T. ) ;
#41774 = B_SPLINE_CURVE_WITH_KNOTS ( 'NONE', 3,
 ( #42224, #22866, #46577, #2738 ),
 .UNSPECIFIED., .F., .F.,
 ( 4, 4 ),
 ( 7.087756405766085514E-05, 0.002570929063738525318 ),
 .UNSPECIFIED. ) ;
#41775 = DIRECTION ( 'NONE',  ( -0.8345732537212999791, 0.000000000000000000, -0.5508969814521065267 ) ) ;
#41776 = VERTEX_POINT ( 'NONE', #46861 ) ;
#41777 = VERTEX_POINT ( 'NONE', #35031 ) ;
#41778 = CARTESIAN_POINT ( 'NONE',  ( -1.363819533518803473, 3.346456692913386100, -0.4724409448818886470 ) ) ;
#41779 = LINE ( 'NONE', #6417, #39910 ) ;
#41780 = CARTESIAN_POINT ( 'NONE',  ( 1.091055626815042423, 3.346456692913386100, -1.574803149606294417 ) ) ;
#41781 = LINE ( 'NONE', #2794, #26749 ) ;
#41782 = EDGE_CURVE ( 'NONE', #28296, #23553, #49314, .T. ) ;
#41783 = LINE ( 'NONE', #26289, #42596 ) ;
#41784 = ORIENTED_EDGE ( 'NONE', *, *, #12405, .F. ) ;
#41785 = AXIS2_PLACEMENT_3D ( 'NONE', #36435, #32572, #21640 ) ;
#41786 = CARTESIAN_POINT ( 'NONE',  ( 0.7423782071083087075, 0.000000000000000000, -0.6299212598425181220 ) ) ;
#41787 = AXIS2_PLACEMENT_3D ( 'NONE', #13886, #34525, #27264 ) ;
#41788 = ORIENTED_EDGE ( 'NONE', *, *, #31871, .T. ) ;
#41789 = ORIENTED_EDGE ( 'NONE', *, *, #46008, .F. ) ;
#41790 = DIRECTION ( 'NONE',  ( -0.000000000000000000, 1.000000000000000000, -0.000000000000000000 ) ) ;
#41791 = VERTEX_POINT ( 'NONE', #39405 ) ;
#41792 = EDGE_CURVE ( 'NONE', #32442, #22912, #50964, .T. ) ;
#41793 = CARTESIAN_POINT ( 'NONE',  ( 1.363819533518803251, 3.346456692913386100, -0.03937007874015908959 ) ) ;
#41794 = DIRECTION ( 'NONE',  ( -1.000000000000000000, 0.000000000000000000, 1.734723475976806848E-16 ) ) ;
#41795 = ORIENTED_EDGE ( 'NONE', *, *, #8974, .T. ) ;
#41796 = CARTESIAN_POINT ( 'NONE',  ( 1.833433833923351353, 3.346456692913386100, 1.377952755905504256 ) ) ;
#41797 = VECTOR ( 'NONE', #12468, 39.37007874015748143 ) ;
#41798 = EDGE_CURVE ( 'NONE', #44322, #42262, #50447, .T. ) ;
#41799 = CARTESIAN_POINT ( 'NONE',  ( 1.157218145390799258, 2.755905511811024056, 0.2363238328731523119 ) ) ;
#41801 = CARTESIAN_POINT ( 'NONE',  ( 0.5455278134075212115, 0.000000000000000000, -0.3149606299212593941 ) ) ;
#41800 = B_SPLINE_CURVE_WITH_KNOTS ( 'NONE', 3,
 ( #25771, #33541, #21649, #48459 ),
 .UNSPECIFIED., .F., .F.,
 ( 4, 4 ),
 ( 2.558223237824230539E-07, 0.002500373809894031792 ),
 .UNSPECIFIED. ) ;
#41802 = ORIENTED_EDGE ( 'NONE', *, *, #45928, .T. ) ;
#41803 = ORIENTED_EDGE ( 'NONE', *, *, #27981, .T. ) ;
#41804 = CARTESIAN_POINT ( 'NONE',  ( 0.2156685157584260770, 1.624173731825095723, -2.945280361644574185 ) ) ;
#41805 = FACE_BOUND ( 'NONE', #28635, .T. ) ;
#41806 = VERTEX_POINT ( 'NONE', #26762 ) ;
#41807 = EDGE_CURVE ( 'NONE', #25781, #6769, #15399, .T. ) ;
#41808 = CARTESIAN_POINT ( 'NONE',  ( 0.9432913529151772947, 1.723010488186151878, -2.072188145589165753 ) ) ;
#41809 = DIRECTION ( 'NONE',  ( 1.000000000000000000, 0.000000000000000000, -3.469446951953613696E-16 ) ) ;
#41810 = VERTEX_POINT ( 'NONE', #31664 ) ;
#41811 = ORIENTED_EDGE ( 'NONE', *, *, #24467, .F. ) ;
#41812 = DIRECTION ( 'NONE',  ( 0.000000000000000000, 0.000000000000000000, 1.000000000000000000 ) ) ;
#41813 = CARTESIAN_POINT ( 'NONE',  ( 1.287906020515829919, 0.000000000000000000, -2.086614173228339641 ) ) ;
#41814 = EDGE_CURVE ( 'NONE', #27359, #50834, #12038, .T. ) ;
#41815 = ORIENTED_EDGE ( 'NONE', *, *, #28855, .F. ) ;
#41816 = EDGE_LOOP ( 'NONE', ( #29817, #18650, #27570, #34190 ) ) ;
#41818 = EDGE_CURVE ( 'NONE', #29455, #41810, #38814, .T. ) ;
#41817 = ORIENTED_EDGE ( 'NONE', *, *, #7719, .F. ) ;
#41819 = CARTESIAN_POINT ( 'NONE',  ( -0.5455278134075214336, 3.346456692913386100, -0.1968503937007883287 ) ) ;
#41820 = DIRECTION ( 'NONE',  ( -0.000000000000000000, 1.000000000000000000, -0.000000000000000000 ) ) ;
#41821 = VECTOR ( 'NONE', #17776, 39.37007874015748143 ) ;
#41823 = CARTESIAN_POINT ( 'NONE',  ( 1.818390528211208945, 3.346456692913386100, 1.062992125984245639 ) ) ;
#41822 = VECTOR ( 'NONE', #38293, 39.37007874015748143 ) ;
#41824 = CARTESIAN_POINT ( 'NONE',  ( -1.477691947303356290, 1.684234009953186728, 1.616556376299586706 ) ) ;
#41825 = ORIENTED_EDGE ( 'NONE', *, *, #36369, .F. ) ;
#41826 = ORIENTED_EDGE ( 'NONE', *, *, #22824, .T. ) ;
#41828 = VECTOR ( 'NONE', #50902, 39.37007874015748143 ) ;
#41827 = CARTESIAN_POINT ( 'NONE',  ( -0.8192648851572477131, 1.600279018255590158, 2.322980749500460185 ) ) ;
#41829 = CARTESIAN_POINT ( 'NONE',  ( 1.785493683324574254, 0.000000000000000000, -1.119626681005672530 ) ) ;
#41830 = CARTESIAN_POINT ( 'NONE',  ( -0.8942052331142552601, 3.346456692913386100, -0.5118110236220467790 ) ) ;
#41831 = CARTESIAN_POINT ( 'NONE',  ( -0.2627480064045953911, 0.000000000000000000, 1.723473835155032274 ) ) ;
#41832 = CARTESIAN_POINT ( 'NONE',  ( 0.000000000000000000, 1.574803149606302854, 0.000000000000000000 ) ) ;
#41833 = EDGE_CURVE ( 'NONE', #42163, #1464, #27087, .T. ) ;
#41834 = LINE ( 'NONE', #22218, #15247 ) ;
#41835 = EDGE_CURVE ( 'NONE', #31188, #21069, #24639, .T. ) ;
#41836 = CARTESIAN_POINT ( 'NONE',  ( -0.5455278134075214336, 3.267716535433071279, 2.034427629037600660 ) ) ;
#41837 = ORIENTED_EDGE ( 'NONE', *, *, #28777, .T. ) ;
#41838 = CARTESIAN_POINT ( 'NONE',  ( -0.3486774197067334380, 3.346456692913386100, 1.259842519685033357 ) ) ;
#41839 = CARTESIAN_POINT ( 'NONE',  ( -0.2086445790628121688, 0.000000000000000000, 0.3067337401345523462 ) ) ;
#41840 = AXIS2_PLACEMENT_3D ( 'NONE', #7466, #3593, #31725 ) ;
#41841 = ORIENTED_EDGE ( 'NONE', *, *, #47110, .F. ) ;
#41842 = ORIENTED_EDGE ( 'NONE', *, *, #24030, .F. ) ;
#41843 = DIRECTION ( 'NONE',  ( 1.734723475976806848E-16, -0.000000000000000000, 1.000000000000000000 ) ) ;
#41844 = VERTEX_POINT ( 'NONE', #30902 ) ;
#41845 = EDGE_LOOP ( 'NONE', ( #30611, #18447, #22946, #8566 ) ) ;
#41846 = CARTESIAN_POINT ( 'NONE',  ( 1.909347346926324462, 3.346456692913386100, -1.299212598425194320 ) ) ;
#41847 = ORIENTED_EDGE ( 'NONE', *, *, #22145, .F. ) ;
#41848 = CARTESIAN_POINT ( 'NONE',  ( -1.536664496436148184E-16, 3.346456692913386100, 0.4330708661417287386 ) ) ;
#41849 = CARTESIAN_POINT ( 'NONE',  ( -0.3486774197067339376, 0.000000000000000000, -8.878505979408855953E-16 ) ) ;
#41850 = AXIS2_PLACEMENT_3D ( 'NONE', #12626, #47184, #39484 ) ;
#41851 = EDGE_CURVE ( 'NONE', #47418, #50807, #6389, .T. ) ;
#41852 = VERTEX_POINT ( 'NONE', #43260 ) ;
#41853 = VERTEX_POINT ( 'NONE', #11281 ) ;
#41854 = DIRECTION ( 'NONE',  ( -5.207613805427244364E-18, -1.000000000000000000, -1.159565308550900415E-16 ) ) ;
#41855 = EDGE_LOOP ( 'NONE', ( #1386, #34673, #15759, #31529 ) ) ;
#41856 = VERTEX_POINT ( 'NONE', #18772 ) ;
#41857 = CARTESIAN_POINT ( 'NONE',  ( 0.000000000000000000, 3.267716535433071279, -0.4724409448818889246 ) ) ;
#41858 = CARTESIAN_POINT ( 'NONE',  ( -0.2727639067037611054, 0.000000000000000000, -2.244094488188968395 ) ) ;
#41859 = DIRECTION ( 'NONE',  ( -0.000000000000000000, 1.000000000000000000, -0.000000000000000000 ) ) ;
#41860 = DIRECTION ( 'NONE',  ( -0.4738686624730094055, 0.000000000000000000, 0.8805955318567321166 ) ) ;
#41861 = AXIS2_PLACEMENT_3D ( 'NONE', #12917, #16789, #39760 ) ;
#41862 = EDGE_CURVE ( 'NONE', #39550, #25006, #7407, .T. ) ;
#41863 = ORIENTED_EDGE ( 'NONE', *, *, #8211, .T. ) ;
#41864 = ADVANCED_FACE ( 'NONE', ( #39149 ), #38564, .T. ) ;
#41865 = CARTESIAN_POINT ( 'NONE',  ( 0.000000000000000000, 3.267716535433071279, 0.3149606299212576177 ) ) ;
#41866 = DIRECTION ( 'NONE',  ( 1.734723475976806848E-16, 0.000000000000000000, 1.000000000000000000 ) ) ;
#41867 = FACE_OUTER_BOUND ( 'NONE', #47133, .T. ) ;
#41868 = ADVANCED_FACE ( 'NONE', ( #23144 ), #19265, .F. ) ;
#41869 = VERTEX_POINT ( 'NONE', #3785 ) ;
#41870 = VECTOR ( 'NONE', #27064, 39.37007874015748143 ) ;
#41871 = DIRECTION ( 'NONE',  ( -0.000000000000000000, -1.000000000000000000, -0.000000000000000000 ) ) ;
#41872 = FACE_OUTER_BOUND ( 'NONE', #28887, .T. ) ;
#41873 = CARTESIAN_POINT ( 'NONE',  ( -0.5455278134075208785, 0.000000000000000000, 0.9448818897637749625 ) ) ;
#41874 = ORIENTED_EDGE ( 'NONE', *, *, #36428, .T. ) ;
#41875 = ORIENTED_EDGE ( 'NONE', *, *, #45770, .T. ) ;
#41876 =( NAMED_UNIT ( * ) PLANE_ANGLE_UNIT ( ) SI_UNIT ( $, .RADIAN. ) );
#41877 = VECTOR ( 'NONE', #19713, 39.37007874015748143 ) ;
#41878 = PLANE ( 'NONE',  #35481 ) ;
#41879 = CARTESIAN_POINT ( 'NONE',  ( -1.977157105026591699, 1.676234161373136189, -0.8985969286390745880 ) ) ;
#41880 = ADVANCED_FACE ( 'NONE', ( #7653 ), #11022, .F. ) ;
#41881 = CARTESIAN_POINT ( 'NONE',  ( 1.950008968278537091, -1.129616514605691021E-16, 0.9934589848971179249 ) ) ;
#41882 = ORIENTED_EDGE ( 'NONE', *, *, #28681, .F. ) ;
#41883 = ORIENTED_EDGE ( 'NONE', *, *, #6, .T. ) ;
#41884 = LINE ( 'NONE', #37769, #10278 ) ;
#41885 = ORIENTED_EDGE ( 'NONE', *, *, #22416, .T. ) ;
#41886 = CARTESIAN_POINT ( 'NONE',  ( -2.071704270381554913, 3.346456692913386100, 0.6299212598425164567 ) ) ;
#41887 = CARTESIAN_POINT ( 'NONE',  ( 0.4696143004045476577, 3.346456692913386100, -2.053280005709960054 ) ) ;
#41888 = EDGE_CURVE ( 'NONE', #41557, #37648, #23915, .T. ) ;
#41889 = VECTOR ( 'NONE', #22795, 39.37007874015748143 ) ;
#41890 = VECTOR ( 'NONE', #20756, 39.37007874015748143 ) ;
#41891 = EDGE_CURVE ( 'NONE', #41040, #18225, #36819, .T. ) ;
#41892 = DIRECTION ( 'NONE',  ( 0.000000000000000000, 1.000000000000000000, 0.000000000000000000 ) ) ;
#41893 = LINE ( 'NONE', #18904, #10421 ) ;
#41894 = DIRECTION ( 'NONE',  ( -3.986037398843765983E-20, -1.000000000000000000, -1.160734090543304660E-16 ) ) ;
#41895 = VERTEX_POINT ( 'NONE', #24174 ) ;
#41896 = DIRECTION ( 'NONE',  ( -1.000000000000000000, 0.000000000000000000, 1.734723475976806848E-16 ) ) ;
#41897 = VECTOR ( 'NONE', #48176, 39.37007874015748143 ) ;
#41898 = DIRECTION ( 'NONE',  ( -1.000000000000000000, 0.000000000000000000, 0.000000000000000000 ) ) ;
#41899 = ORIENTED_EDGE ( 'NONE', *, *, #41376, .F. ) ;
#41901 = CARTESIAN_POINT ( 'NONE',  ( -0.5455278134075214336, 3.346456692913386100, -1.889763779527552146 ) ) ;
#41900 = VECTOR ( 'NONE', #9848, 39.37007874015748143 ) ;
#41902 = CARTESIAN_POINT ( 'NONE',  ( -1.220415235146723676, 0.5160455853568218787, -0.4330136603435745246 ) ) ;
#41903 = DIRECTION ( 'NONE',  ( -1.000000000000000000, -0.000000000000000000, -0.000000000000000000 ) ) ;
#41904 = VERTEX_POINT ( 'NONE', #12299 ) ;
#41905 = AXIS2_PLACEMENT_3D ( 'NONE', #35783, #47868, #24164 ) ;
#41906 = CARTESIAN_POINT ( 'NONE',  ( -1.909347346926324462, 0.000000000000000000, 0.2755905511810996522 ) ) ;
#41907 = ORIENTED_EDGE ( 'NONE', *, *, #15002, .F. ) ;
#41908 = DIRECTION ( 'NONE',  ( 0.000000000000000000, -1.000000000000000000, -0.000000000000000000 ) ) ;
#41909 = EDGE_LOOP ( 'NONE', ( #27419, #10506, #10537, #33608 ) ) ;
#41910 = VECTOR ( 'NONE', #18905, 39.37007874015748143 ) ;
#41911 = CARTESIAN_POINT ( 'NONE',  ( 0.2727639067037604947, 3.346456692913386100, -0.7874015748031473194 ) ) ;
#41912 = CARTESIAN_POINT ( 'NONE',  ( -0.5455278134075216556, 3.267716535433071279, -2.204724409448810540 ) ) ;
#41913 = LINE ( 'NONE', #30295, #20600 ) ;
#41914 = DIRECTION ( 'NONE',  ( -0.000000000000000000, 1.000000000000000000, -0.000000000000000000 ) ) ;
#41915 = ORIENTED_EDGE ( 'NONE', *, *, #2340, .T. ) ;
#41916 = ORIENTED_EDGE ( 'NONE', *, *, #14149, .F. ) ;
#41917 = CARTESIAN_POINT ( 'NONE',  ( -1.636583440222563635, 3.267716535433071279, 1.259842519685033357 ) ) ;
#41918 = DIRECTION ( 'NONE',  ( -0.000000000000000000, 1.000000000000000000, -0.000000000000000000 ) ) ;
#41919 = ORIENTED_EDGE ( 'NONE', *, *, #43337, .F. ) ;
#41920 = CARTESIAN_POINT ( 'NONE',  ( -1.091055626815042645, 0.000000000000000000, 1.692913385826762873 ) ) ;
#41921 = CARTESIAN_POINT ( 'NONE',  ( -1.022165783835742969, 1.604882761207047759, 2.770237110760823462 ) ) ;
#41922 = DIRECTION ( 'NONE',  ( -1.000000000000000000, -0.000000000000000000, -0.000000000000000000 ) ) ;
#41923 = ORIENTED_EDGE ( 'NONE', *, *, #14181, .T. ) ;
#41924 = VERTEX_POINT ( 'NONE', #43772 ) ;
#41925 = EDGE_CURVE ( 'NONE', #1039, #12446, #44294, .T. ) ;
#41926 = CARTESIAN_POINT ( 'NONE',  ( -2.182111253630085290, 3.226699998040846395, -1.141732283464563791 ) ) ;
#41927 = CARTESIAN_POINT ( 'NONE',  ( 0.000000000000000000, 1.574803149606302854, 0.000000000000000000 ) ) ;
#41928 = VECTOR ( 'NONE', #4074, 39.37007874015748143 ) ;
#41929 = PLANE ( 'NONE',  #5772 ) ;
#41930 = EDGE_CURVE ( 'NONE', #47925, #39171, #44541, .T. ) ;
#41931 = ORIENTED_EDGE ( 'NONE', *, *, #32567, .T. ) ;
#41932 = FILL_AREA_STYLE_COLOUR ( '', #7540 ) ;
#41933 = EDGE_CURVE ( 'NONE', #12607, #32732, #36308, .T. ) ;
#41934 = FACE_BOUND ( 'NONE', #8282, .T. ) ;
#41935 = ORIENTED_EDGE ( 'NONE', *, *, #25198, .T. ) ;
#41936 = DIRECTION ( 'NONE',  ( 1.000000000000000000, 0.000000000000000000, 0.000000000000000000 ) ) ;
#41937 = VERTEX_POINT ( 'NONE', #48638 ) ;
#41939 = ORIENTED_EDGE ( 'NONE', *, *, #36834, .T. ) ;
#41938 = VECTOR ( 'NONE', #30982, 39.37007874015748143 ) ;
#41940 = CARTESIAN_POINT ( 'NONE',  ( 0.08139965876239094178, 1.610780518492231694, 0.000000000000000000 ) ) ;
#41941 = CARTESIAN_POINT ( 'NONE',  ( -2.437180031585919782, 1.566133505135788750, -1.667735833703134274 ) ) ;
#41942 = EDGE_CURVE ( 'NONE', #13750, #12775, #50992, .T. ) ;
#41943 = VECTOR ( 'NONE', #13663, 39.37007874015748143 ) ;
#41944 = DIRECTION ( 'NONE',  ( -0.9998717552508122886, -0.01601477604151180928, 0.000000000000000000 ) ) ;
#41945 = VERTEX_POINT ( 'NONE', #28034 ) ;
#41946 = CARTESIAN_POINT ( 'NONE',  ( 0.07982360342473591996, 1.709180471932028711, 0.000000000000000000 ) ) ;
#41947 = CARTESIAN_POINT ( 'NONE',  ( 0.000000000000000000, 3.267716535433071279, 1.062992125984246083 ) ) ;
#41948 = ORIENTED_EDGE ( 'NONE', *, *, #27629, .T. ) ;
#41949 = EDGE_CURVE ( 'NONE', #10297, #50880, #39918, .T. ) ;
#41950 = VECTOR ( 'NONE', #8942, 39.37007874015748143 ) ;
#41951 = ORIENTED_EDGE ( 'NONE', *, *, #25790, .T. ) ;
#41952 = DIRECTION ( 'NONE',  ( -0.000000000000000000, 1.000000000000000000, -0.000000000000000000 ) ) ;
#41953 = PLANE ( 'NONE',  #11921 ) ;
#41954 = EDGE_CURVE ( 'NONE', #29231, #11067, #16431, .T. ) ;
#41955 = CARTESIAN_POINT ( 'NONE',  ( -0.2727639067037607723, 3.267716535433071279, -0.4724409448818883694 ) ) ;
#41956 = EDGE_CURVE ( 'NONE', #41000, #46126, #12159, .T. ) ;
#41957 = CARTESIAN_POINT ( 'NONE',  ( 0.8182917201112819283, 3.346456692913386100, 0.2755905511810994302 ) ) ;
#41958 = PLANE ( 'NONE',  #17958 ) ;
#41959 = EDGE_LOOP ( 'NONE', ( #22066, #4, #5426, #35179, #25723, #9277, #17496, #10503, #35701, #710, #45063 ) ) ;
#41960 = CARTESIAN_POINT ( 'NONE',  ( 1.281152772984937682, 0.000000000000000000, -2.660341145381147854 ) ) ;
#41961 = EDGE_CURVE ( 'NONE', #9086, #36296, #47874, .T. ) ;
#41962 = EDGE_CURVE ( 'NONE', #35465, #25743, #4808, .T. ) ;
#41963 = FACE_OUTER_BOUND ( 'NONE', #48142, .T. ) ;
#41964 = ORIENTED_EDGE ( 'NONE', *, *, #23702, .F. ) ;
#41965 = LINE ( 'NONE', #6604, #17479 ) ;
#41966 = CARTESIAN_POINT ( 'NONE',  ( 0.000000000000000000, 3.267716535433071279, 0.6299212598425161236 ) ) ;
#41967 = ORIENTED_EDGE ( 'NONE', *, *, #41006, .T. ) ;
#41968 = CARTESIAN_POINT ( 'NONE',  ( -1.738729679588005617, 0.000000000000000000, -0.1273486421340072894 ) ) ;
#41969 = AXIS2_PLACEMENT_3D ( 'NONE', #47840, #24134, #4513 ) ;
#41970 = DIRECTION ( 'NONE',  ( -0.000000000000000000, 1.000000000000000000, -0.000000000000000000 ) ) ;
#41971 = CARTESIAN_POINT ( 'NONE',  ( 0.4696143004045476022, 3.267716535433071279, -2.244094488188969727 ) ) ;
#41972 = ORIENTED_EDGE ( 'NONE', *, *, #21361, .F. ) ;
#41973 = DIRECTION ( 'NONE',  ( 1.000000000000000000, 0.000000000000000000, -3.469446951953613696E-16 ) ) ;
#41974 = ORIENTED_EDGE ( 'NONE', *, *, #48401, .T. ) ;
#41975 = FACE_BOUND ( 'NONE', #4705, .T. ) ;
#41976 = CARTESIAN_POINT ( 'NONE',  ( 0.1968503937007874127, 3.267716535433071279, -6.829619984160656814E-17 ) ) ;
#41977 = AXIS2_PLACEMENT_3D ( 'NONE', #21546, #5798, #2684 ) ;
#41978 = CIRCLE ( 'NONE', #8175, 2.246510896728926010 ) ;
#41979 = LINE ( 'NONE', #19230, #28430 ) ;
#41980 = LINE ( 'NONE', #10737, #38381 ) ;
#41981 = VECTOR ( 'NONE', #22267, 39.37007874015748143 ) ;
#41982 = VERTEX_POINT ( 'NONE', #8169 ) ;
#41983 = EDGE_LOOP ( 'NONE', ( #23570, #44878, #9328, #30598 ) ) ;
#41984 = CARTESIAN_POINT ( 'NONE',  ( 1.761907912426849521, 1.644691605102268195, 2.091464020505111154 ) ) ;
#41985 = CARTESIAN_POINT ( 'NONE',  ( -1.676283831994445306, 0.001070912127414903967, 0.4929124452910598198 ) ) ;
#41986 = LINE ( 'NONE', #17289, #7084 ) ;
#41987 = AXIS2_PLACEMENT_3D ( 'NONE', #49353, #25138, #14026 ) ;
#41988 = CARTESIAN_POINT ( 'NONE',  ( -0.07591351300297366489, 3.267716535433071279, -2.244094488188968395 ) ) ;
#41989 = FACE_OUTER_BOUND ( 'NONE', #19919, .T. ) ;
#41990 = ORIENTED_EDGE ( 'NONE', *, *, #31451, .F. ) ;
#41991 = CARTESIAN_POINT ( 'NONE',  ( 0.2727639067037609943, 3.346456692913386100, 1.535433070866133898 ) ) ;
#41992 = CARTESIAN_POINT ( 'NONE',  ( 1.909347346926324462, 3.346456692913386100, -1.299212598425194320 ) ) ;
#41993 = EDGE_CURVE ( 'NONE', #12580, #7930, #48385, .T. ) ;
#41994 = VERTEX_POINT ( 'NONE', #35791 ) ;
#41995 = EDGE_CURVE ( 'NONE', #12211, #50070, #31930, .T. ) ;
#41996 = CARTESIAN_POINT ( 'NONE',  ( -0.5455278134075208785, 3.346456692913386100, 0.6299212598425164567 ) ) ;
#41997 = EDGE_LOOP ( 'NONE', ( #3663, #17805, #3056, #48180 ) ) ;
#41998 = ORIENTED_EDGE ( 'NONE', *, *, #36119, .F. ) ;
#41999 = EDGE_CURVE ( 'NONE', #456, #22772, #4292, .T. ) ;
#42000 = VECTOR ( 'NONE', #41918, 39.37007874015748143 ) ;
#42001 = ORIENTED_EDGE ( 'NONE', *, *, #43277, .T. ) ;
#42002 = ORIENTED_EDGE ( 'NONE', *, *, #3103, .T. ) ;
#42003 = CARTESIAN_POINT ( 'NONE',  ( -1.536664496436148184E-16, 3.346456692913386100, -1.456692913385822630 ) ) ;
#42004 = ORIENTED_EDGE ( 'NONE', *, *, #7329, .T. ) ;
#42005 = LINE ( 'NONE', #29101, #20485 ) ;
#42006 = LINE ( 'NONE', #49957, #504 ) ;
#42007 = AXIS2_PLACEMENT_3D ( 'NONE', #49827, #45978, #38520 ) ;
#42008 = EDGE_CURVE ( 'NONE', #31067, #16368, #32441, .T. ) ;
#42009 = CARTESIAN_POINT ( 'NONE',  ( -1.985260859929298016, 3.267716535433071279, -0.6299212598425177889 ) ) ;
#42010 = AXIS2_PLACEMENT_3D ( 'NONE', #2729, #6856, #10732 ) ;
#42011 = CARTESIAN_POINT ( 'NONE',  ( 1.243905582186644043, 1.632961070568905715, 2.177897092110659294 ) ) ;
#42012 = CARTESIAN_POINT ( 'NONE',  ( 0.4696143004045476577, 3.346456692913386100, -2.047244094488182231 ) ) ;
#42013 = ORIENTED_EDGE ( 'NONE', *, *, #15545, .T. ) ;
#42014 = EDGE_CURVE ( 'NONE', #32787, #18949, #32704, .T. ) ;
#42015 = DIRECTION ( 'NONE',  ( -0.000000000000000000, -1.000000000000000000, -0.000000000000000000 ) ) ;
#42016 = CARTESIAN_POINT ( 'NONE',  ( -1.363819533518803029, 3.346456692913386100, 0.5905511811023582691 ) ) ;
#42017 = EDGE_CURVE ( 'NONE', #24291, #23949, #36562, .T. ) ;
#42018 = AXIS2_PLACEMENT_3D ( 'NONE', #48092, #14925, #377 ) ;
#42019 = CARTESIAN_POINT ( 'NONE',  ( 1.909347346926324684, 0.000000000000000000, -0.6692913385826764205 ) ) ;
#42020 = DIRECTION ( 'NONE',  ( -0.5773502691896266192, 0.5773502691896260641, -0.5773502691896246208 ) ) ;
#42021 = EDGE_LOOP ( 'NONE', ( #5256, #29584, #11176, #15676 ) ) ;
#42022 = CARTESIAN_POINT ( 'NONE',  ( 2.074049943651431693, 6.692913385826772199, 0.6221544894624241318 ) ) ;
#42023 = CARTESIAN_POINT ( 'NONE',  ( -0.3486774197067339376, 3.346456692913386100, -1.889763779527552146 ) ) ;
#42024 = ORIENTED_EDGE ( 'NONE', *, *, #21888, .T. ) ;
#42025 = CARTESIAN_POINT ( 'NONE',  ( -1.002140947543763705, 1.626234033651570821, -1.967543651896755508 ) ) ;
#42026 = DIRECTION ( 'NONE',  ( 0.000000000000000000, 0.000000000000000000, -1.000000000000000000 ) ) ;
#42027 = ORIENTED_EDGE ( 'NONE', *, *, #21898, .F. ) ;
#42028 = DIRECTION ( 'NONE',  ( -1.000000000000000000, -0.000000000000000000, -0.000000000000000000 ) ) ;
#42029 = ORIENTED_EDGE ( 'NONE', *, *, #48495, .F. ) ;
#42030 = FACE_OUTER_BOUND ( 'NONE', #48095, .T. ) ;
#42031 = CARTESIAN_POINT ( 'NONE',  ( -1.312248418042854192, 6.692913385826772199, -1.722429524498108933 ) ) ;
#42032 = LINE ( 'NONE', #14157, #24565 ) ;
#42033 = FACE_OUTER_BOUND ( 'NONE', #43613, .T. ) ;
#42034 = CARTESIAN_POINT ( 'NONE',  ( -0.2727639067037602172, 0.000000000000000000, 1.732283464566921172 ) ) ;
#42035 = VECTOR ( 'NONE', #39239, 39.37007874015748143 ) ;
#42036 = ORIENTED_EDGE ( 'NONE', *, *, #23383, .T. ) ;
#42037 = CARTESIAN_POINT ( 'NONE',  ( 0.08139965876239094178, 1.610780518492231694, 0.000000000000000000 ) ) ;
#42038 = ORIENTED_EDGE ( 'NONE', *, *, #25936, .T. ) ;
#42039 = ORIENTED_EDGE ( 'NONE', *, *, #5922, .T. ) ;
#42040 = LINE ( 'NONE', #34307, #16350 ) ;
#42041 = ORIENTED_EDGE ( 'NONE', *, *, #11922, .F. ) ;
#42042 = DIRECTION ( 'NONE',  ( 1.000000000000000000, -0.000000000000000000, 0.000000000000000000 ) ) ;
#42043 = FACE_OUTER_BOUND ( 'NONE', #1502, .T. ) ;
#42044 = ORIENTED_EDGE ( 'NONE', *, *, #45335, .T. ) ;
#42045 = AXIS2_PLACEMENT_3D ( 'NONE', #21694, #37452, #2074 ) ;
#42046 = DIRECTION ( 'NONE',  ( 1.000000000000000000, 0.000000000000000000, 0.000000000000000000 ) ) ;
#42047 = FACE_OUTER_BOUND ( 'NONE', #37490, .T. ) ;
#42048 = ADVANCED_FACE ( 'NONE', ( #47623 ), #40442, .F. ) ;
#42049 = DIRECTION ( 'NONE',  ( -1.000000000000000000, 0.000000000000000000, 0.000000000000000000 ) ) ;
#42050 = ORIENTED_EDGE ( 'NONE', *, *, #49746, .F. ) ;
#42052 = ORIENTED_EDGE ( 'NONE', *, *, #48782, .T. ) ;
#42051 = ADVANCED_FACE ( 'NONE', ( #30085 ), #41958, .F. ) ;
#42053 = CARTESIAN_POINT ( 'NONE',  ( 0.1526763070133267952, 1.611922144458495687, -2.245379599360889600 ) ) ;
#42054 = FACE_BOUND ( 'NONE', #21662, .T. ) ;
#42055 = ORIENTED_EDGE ( 'NONE', *, *, #7485, .T. ) ;
#42056 = VECTOR ( 'NONE', #37736, 39.37007874015748143 ) ;
#42057 = EDGE_CURVE ( 'NONE', #44367, #45040, #34220, .T. ) ;
#42058 = DIRECTION ( 'NONE',  ( -0.000000000000000000, 0.000000000000000000, 1.000000000000000000 ) ) ;
#42059 = LINE ( 'NONE', #15889, #48923 ) ;
#42060 = EDGE_CURVE ( 'NONE', #16832, #37208, #634, .T. ) ;
#42062 = ORIENTED_EDGE ( 'NONE', *, *, #5982, .F. ) ;
#42061 = EDGE_CURVE ( 'NONE', #34736, #26467, #33469, .T. ) ;
#42063 = ORIENTED_EDGE ( 'NONE', *, *, #36162, .T. ) ;
#42064 = DIRECTION ( 'NONE',  ( 0.000000000000000000, 0.000000000000000000, 1.000000000000000000 ) ) ;
#42065 = CARTESIAN_POINT ( 'NONE',  ( 0.7423782071083084855, 3.267716535433071279, -1.971134437475891454 ) ) ;
#42066 = ORIENTED_EDGE ( 'NONE', *, *, #41538, .F. ) ;
#42067 = EDGE_LOOP ( 'NONE', ( #33507, #42401, #17043, #12174 ) ) ;
#42068 = ORIENTED_EDGE ( 'NONE', *, *, #10557, .F. ) ;
#42069 = DIRECTION ( 'NONE',  ( 1.734723475976806848E-16, 0.000000000000000000, 1.000000000000000000 ) ) ;
#42070 = CARTESIAN_POINT ( 'NONE',  ( -1.636583440222563635, 0.000000000000000000, 0.9448818897637749625 ) ) ;
#42071 = EDGE_CURVE ( 'NONE', #21408, #23810, #46716, .T. ) ;
#42072 = LINE ( 'NONE', #50024, #37119 ) ;
#42073 = VERTEX_POINT ( 'NONE', #22340 ) ;
#42074 = ORIENTED_EDGE ( 'NONE', *, *, #38588, .F. ) ;
#42075 = PLANE ( 'NONE',  #49640 ) ;
#42076 = CARTESIAN_POINT ( 'NONE',  ( 0.07982360342473591996, 1.709180471932028711, 0.000000000000000000 ) ) ;
#42077 = DIRECTION ( 'NONE',  ( -1.000000000000000000, 0.000000000000000000, 0.000000000000000000 ) ) ;
#42078 = EDGE_CURVE ( 'NONE', #4136, #12830, #49152, .T. ) ;
#42079 = DIRECTION ( 'NONE',  ( -0.000000000000000000, 0.000000000000000000, 1.000000000000000000 ) ) ;
#42080 = CARTESIAN_POINT ( 'NONE',  ( -0.6087643519215788501, 1.702044864518692746, -2.390792234956752083 ) ) ;
#42081 = VECTOR ( 'NONE', #41447, 39.37007874015748143 ) ;
#42082 = AXIS2_PLACEMENT_3D ( 'NONE', #36869, #10194, #18707 ) ;
#42083 = CARTESIAN_POINT ( 'NONE',  ( 1.833433833923351353, 3.346456692913386100, 0.4330708661417290162 ) ) ;
#42084 = ADVANCED_FACE ( 'NONE', ( #49406 ), #3949, .T. ) ;
#42085 = CARTESIAN_POINT ( 'NONE',  ( -1.166969139818015533, 3.267716535433071279, 1.102362204724404160 ) ) ;
#42086 = ORIENTED_EDGE ( 'NONE', *, *, #23207, .T. ) ;
#42087 = CARTESIAN_POINT ( 'NONE',  ( -0.8182917201112819283, 3.346456692913386100, -1.732283464566922726 ) ) ;
#42088 = CARTESIAN_POINT ( 'NONE',  ( -0.2483604914213126402, 1.519985912000072936, -2.942338030579628061 ) ) ;
#42089 = VECTOR ( 'NONE', #1785, 39.37007874015748143 ) ;
#42090 = VERTEX_POINT ( 'NONE', #2470 ) ;
#42091 = EDGE_CURVE ( 'NONE', #20029, #46385, #37542, .T. ) ;
#42092 = ORIENTED_EDGE ( 'NONE', *, *, #39443, .T. ) ;
#42093 = DIRECTION ( 'NONE',  ( -0.9749279121818227312, 0.000000000000000000, -0.2225209339563184452 ) ) ;
#42094 = VERTEX_POINT ( 'NONE', #33722 ) ;
#42095 = VERTEX_POINT ( 'NONE', #37076 ) ;
#42096 = CARTESIAN_POINT ( 'NONE',  ( -1.636583440222563857, 3.267716535433071279, 2.839019714148966584E-16 ) ) ;
#42097 = VERTEX_POINT ( 'NONE', #6341 ) ;
#42098 = DIRECTION ( 'NONE',  ( 0.000000000000000000, -1.000000000000000000, 0.000000000000000000 ) ) ;
#42099 = CARTESIAN_POINT ( 'NONE',  ( 0.8446807076687119498, 1.721431058233622746, 2.110586427442081803 ) ) ;
#42100 = ORIENTED_EDGE ( 'NONE', *, *, #15975, .F. ) ;
#42101 = DIRECTION ( 'NONE',  ( 0.000000000000000000, 0.000000000000000000, -1.000000000000000000 ) ) ;
#42102 = ORIENTED_EDGE ( 'NONE', *, *, #30498, .F. ) ;
#42103 = ORIENTED_EDGE ( 'NONE', *, *, #18349, .F. ) ;
#42104 = CARTESIAN_POINT ( 'NONE',  ( -2.152441353505195387, 0.000000000000000000, -0.2419059403265113872 ) ) ;
#42105 = CARTESIAN_POINT ( 'NONE',  ( 0.04921259842519667971, 1.708690180665275005, 2.244725876464058523 ) ) ;
#42106 = CARTESIAN_POINT ( 'NONE',  ( 0.8182917201112824834, 0.000000000000000000, 1.535433070866133898 ) ) ;
#42107 = DIRECTION ( 'NONE',  ( -0.000000000000000000, 0.000000000000000000, 1.000000000000000000 ) ) ;
#42108 = EDGE_CURVE ( 'NONE', #1339, #46515, #37848, .T. ) ;
#42109 = VECTOR ( 'NONE', #6402, 39.37007874015748854 ) ;
#42110 = EDGE_LOOP ( 'NONE', ( #32222, #46, #1795, #10027 ) ) ;
#42111 = AXIS2_PLACEMENT_3D ( 'NONE', #31567, #31063, #26672 ) ;
#42112 = DIRECTION ( 'NONE',  ( -0.01601477604151182663, 0.9998717552508123996, -0.000000000000000000 ) ) ;
#42113 = CARTESIAN_POINT ( 'NONE',  ( -1.091055626815042645, 0.000000000000000000, -0.8267716535433052849 ) ) ;
#42114 = ADVANCED_FACE ( 'NONE', ( #10463 ), #29832, .T. ) ;
#42115 = LINE ( 'NONE', #22752, #29469 ) ;
#42116 = EDGE_CURVE ( 'NONE', #35907, #22479, #45799, .T. ) ;
#42117 = ORIENTED_EDGE ( 'NONE', *, *, #29274, .F. ) ;
#42118 = CARTESIAN_POINT ( 'NONE',  ( 0.000000000000000000, 3.346456692913386100, 0.000000000000000000 ) ) ;
#42119 = VERTEX_POINT ( 'NONE', #6074 ) ;
#42120 = ORIENTED_EDGE ( 'NONE', *, *, #37064, .F. ) ;
#42121 = VECTOR ( 'NONE', #12584, 39.37007874015748143 ) ;
#42122 =( NAMED_UNIT ( * ) SI_UNIT ( $, .STERADIAN. ) SOLID_ANGLE_UNIT ( ) );
#42123 = DIRECTION ( 'NONE',  ( -0.5407162030609373726, -0.6444004775717706579, 0.5407162030609373726 ) ) ;
#42124 = DIRECTION ( 'NONE',  ( -1.000000000000000000, 0.000000000000000000, 0.000000000000000000 ) ) ;
#42125 = LINE ( 'NONE', #41373, #11526 ) ;
#42126 = ORIENTED_EDGE ( 'NONE', *, *, #8419, .T. ) ;
#42127 = ORIENTED_EDGE ( 'NONE', *, *, #29921, .T. ) ;
#42128 = DIRECTION ( 'NONE',  ( 1.734723475976806848E-16, -0.000000000000000000, 1.000000000000000000 ) ) ;
#42129 = CARTESIAN_POINT ( 'NONE',  ( -0.8329809839909438907, 1.607838722253305486, -2.833254665166566877 ) ) ;
#42130 = EDGE_LOOP ( 'NONE', ( #49112, #22726, #16011, #27929 ) ) ;
#42131 = PLANE ( 'NONE',  #29075 ) ;
#42132 = LINE ( 'NONE', #23023, #46543 ) ;
#42133 = ADVANCED_FACE ( 'NONE', ( #1951 ), #4762, .T. ) ;
#42134 = DIRECTION ( 'NONE',  ( 0.000000000000000000, 1.160734090543304660E-16, -1.000000000000000000 ) ) ;
#42135 = CARTESIAN_POINT ( 'NONE',  ( -3.927031490892378253E-16, 0.000000000000000000, -2.204724409448811429 ) ) ;
#42136 = LINE ( 'NONE', #42640, #46806 ) ;
#42137 = ORIENTED_EDGE ( 'NONE', *, *, #32959, .F. ) ;
#42138 = DIRECTION ( 'NONE',  ( -1.000000000000000000, 0.000000000000000000, 1.734723475976806848E-16 ) ) ;
#42139 = PLANE ( 'NONE',  #5444 ) ;
#42140 = DIRECTION ( 'NONE',  ( -0.000000000000000000, 0.000000000000000000, 1.000000000000000000 ) ) ;
#42141 = EDGE_CURVE ( 'NONE', #25262, #41036, #30758, .T. ) ;
#42142 = AXIS2_PLACEMENT_3D ( 'NONE', #29835, #9193, #24941 ) ;
#42143 = EDGE_LOOP ( 'NONE', ( #41741, #47680, #13772, #17768 ) ) ;
#42144 = PLANE ( 'NONE',  #20746 ) ;
#42145 = VECTOR ( 'NONE', #6114, 39.37007874015748143 ) ;
#42146 = CARTESIAN_POINT ( 'NONE',  ( 1.287906020515830585, 3.267716535433071279, 1.740706023381843659 ) ) ;
#42147 = CARTESIAN_POINT ( 'NONE',  ( -0.3486774197067342151, 3.346456692913386100, -2.204724409448810540 ) ) ;
#42149 = ADVANCED_FACE ( 'NONE', ( #45294 ), #9957, .F. ) ;
#42148 = ORIENTED_EDGE ( 'NONE', *, *, #41933, .F. ) ;
#42150 = DIRECTION ( 'NONE',  ( 1.734723475976806848E-16, 0.000000000000000000, 1.000000000000000000 ) ) ;
#42151 = EDGE_CURVE ( 'NONE', #49700, #33556, #21832, .T. ) ;
#42152 = ORIENTED_EDGE ( 'NONE', *, *, #30796, .F. ) ;
#42153 = FACE_OUTER_BOUND ( 'NONE', #31308, .T. ) ;
#42154 = VECTOR ( 'NONE', #35632, 39.37007874015748143 ) ;
#42155 = ORIENTED_EDGE ( 'NONE', *, *, #43252, .F. ) ;
#42156 = CARTESIAN_POINT ( 'NONE',  ( -1.985260859929298016, 0.000000000000000000, -0.9448818897637762948 ) ) ;
#42157 = EDGE_CURVE ( 'NONE', #975, #29609, #33635, .T. ) ;
#42158 = VECTOR ( 'NONE', #31671, 39.37007874015748143 ) ;
#42159 = DIRECTION ( 'NONE',  ( -1.000000000000000000, 0.000000000000000000, 0.000000000000000000 ) ) ;
#42160 = CARTESIAN_POINT ( 'NONE',  ( -1.439733046521776361, 3.346456692913386100, 0.4330708661417290162 ) ) ;
#42161 = DIRECTION ( 'NONE',  ( 1.000000000000000000, -0.000000000000000000, 0.000000000000000000 ) ) ;
#42162 = ORIENTED_EDGE ( 'NONE', *, *, #40432, .F. ) ;
#42163 = VERTEX_POINT ( 'NONE', #46553 ) ;
#42164 = CARTESIAN_POINT ( 'NONE',  ( -1.078729122356643755, 3.244501632956205306, 2.204724409448808764 ) ) ;
#42165 = CARTESIAN_POINT ( 'NONE',  ( -0.07591351300297340121, 3.346456692913386100, -0.3543307086614175816 ) ) ;
#42166 = VERTEX_POINT ( 'NONE', #3725 ) ;
#42167 = CARTESIAN_POINT ( 'NONE',  ( -1.439733046521776361, 0.000000000000000000, -0.1968503937007879123 ) ) ;
#42168 = CARTESIAN_POINT ( 'NONE',  ( -0.3465944589516558594, -2.479472480830696451E-16, 2.185505870675810147 ) ) ;
#42169 = CARTESIAN_POINT ( 'NONE',  ( -1.636583440222564301, 3.267716535433071279, -1.325930245594398871 ) ) ;
#42170 = EDGE_CURVE ( 'NONE', #1056, #6843, #34470, .T. ) ;
#42171 = EDGE_LOOP ( 'NONE', ( #35398, #22034, #43153, #19977 ) ) ;
#42172 = EDGE_LOOP ( 'NONE', ( #15309, #32975, #39880, #49760 ) ) ;
#42173 = DIRECTION ( 'NONE',  ( -1.000000000000000000, 0.000000000000000000, 0.000000000000000000 ) ) ;
#42174 = DIRECTION ( 'NONE',  ( 1.734723475976806848E-16, -0.000000000000000000, 1.000000000000000000 ) ) ;
#42175 = CARTESIAN_POINT ( 'NONE',  ( -0.5455278134075214336, 0.000000000000000000, 0.3149606299212577287 ) ) ;
#42176 = ADVANCED_FACE ( 'NONE', ( #26705 ), #2970, .F. ) ;
#42177 = ORIENTED_EDGE ( 'NONE', *, *, #457, .F. ) ;
#42178 = SURFACE_STYLE_USAGE ( .BOTH. , #49880 ) ;
#42179 = CARTESIAN_POINT ( 'NONE',  ( 0.08139965876239094178, 1.610780518492231694, 0.000000000000000000 ) ) ;
#42180 = VERTEX_POINT ( 'NONE', #15347 ) ;
#42181 = LINE ( 'NONE', #49386, #19149 ) ;
#42182 = ORIENTED_EDGE ( 'NONE', *, *, #1239, .F. ) ;
#42183 = ORIENTED_EDGE ( 'NONE', *, *, #28940, .F. ) ;
#42184 = CARTESIAN_POINT ( 'NONE',  ( 0.1155636338427008941, -0.5222242541845523167, 0.000000000000000000 ) ) ;
#42185 = LINE ( 'NONE', #42688, #14369 ) ;
#42186 = VECTOR ( 'NONE', #30534, 39.37007874015748143 ) ;
#42188 = VECTOR ( 'NONE', #45775, 39.37007874015748143 ) ;
#42187 = FACE_OUTER_BOUND ( 'NONE', #6875, .T. ) ;
#42189 = DIRECTION ( 'NONE',  ( -0.000000000000000000, 1.000000000000000000, -0.000000000000000000 ) ) ;
#42190 = DIRECTION ( 'NONE',  ( -3.469446951953613696E-16, 0.000000000000000000, -1.000000000000000000 ) ) ;
#42191 = VERTEX_POINT ( 'NONE', #31097 ) ;
#42192 = VECTOR ( 'NONE', #38180, 39.37007874015748143 ) ;
#42193 = ORIENTED_EDGE ( 'NONE', *, *, #49519, .F. ) ;
#42194 = LINE ( 'NONE', #27203, #26920 ) ;
#42195 = FACE_OUTER_BOUND ( 'NONE', #7240, .T. ) ;
#42196 = VECTOR ( 'NONE', #49351, 39.37007874015748143 ) ;
#42197 = EDGE_CURVE ( 'NONE', #1553, #37294, #21524, .T. ) ;
#42198 = CARTESIAN_POINT ( 'NONE',  ( -1.500384104969938459, 1.597432260198647480, 2.543203506735845831 ) ) ;
#42199 = FACE_OUTER_BOUND ( 'NONE', #44219, .T. ) ;
#42200 = LINE ( 'NONE', #32122, #23727 ) ;
#42201 = ORIENTED_EDGE ( 'NONE', *, *, #38424, .T. ) ;
#42202 = DIRECTION ( 'NONE',  ( 1.734723475976806848E-16, -0.000000000000000000, 1.000000000000000000 ) ) ;
#42203 = CARTESIAN_POINT ( 'NONE',  ( 0.000000000000000000, 3.267716535433071279, 0.7874015748031456541 ) ) ;
#42204 = VERTEX_POINT ( 'NONE', #22585 ) ;
#42205 = DIRECTION ( 'NONE',  ( 1.000000000000000000, -0.000000000000000000, 0.000000000000000000 ) ) ;
#42206 = EDGE_CURVE ( 'NONE', #44848, #2534, #9182, .T. ) ;
#42207 = DIRECTION ( 'NONE',  ( -2.891205793294678326E-16, 0.000000000000000000, 1.000000000000000000 ) ) ;
#42208 = ORIENTED_EDGE ( 'NONE', *, *, #10921, .F. ) ;
#42209 = CARTESIAN_POINT ( 'NONE',  ( 1.363819533518803695, 3.346456692913386100, 1.732283464566921172 ) ) ;
#42210 = EDGE_CURVE ( 'NONE', #9666, #27229, #30592, .T. ) ;
#42211 = DIRECTION ( 'NONE',  ( 1.734723475976806848E-16, 0.000000000000000000, 1.000000000000000000 ) ) ;
#42212 = ADVANCED_FACE ( 'NONE', ( #38347 ), #15599, .F. ) ;
#42213 = CARTESIAN_POINT ( 'NONE',  ( -1.977157105026591699, 1.676234161373136189, -0.8985969286390745880 ) ) ;
#42214 = VERTEX_POINT ( 'NONE', #6842 ) ;
#42215 = CARTESIAN_POINT ( 'NONE',  ( 1.695772546416037807, 5.905511811023623991, -2.417756147381349141 ) ) ;
#42216 = EDGE_LOOP ( 'NONE', ( #29877, #48667, #11438, #34461 ) ) ;
#42217 = FACE_BOUND ( 'NONE', #21295, .T. ) ;
#42218 = CONICAL_SURFACE ( 'NONE', #3457, 2.244934639244524632, 1.554780866114618743 ) ;
#42219 = CARTESIAN_POINT ( 'NONE',  ( -0.3486774197067339376, 0.000000000000000000, -1.889763779527552146 ) ) ;
#42220 = CARTESIAN_POINT ( 'NONE',  ( -1.985260859929298016, 3.346456692913386100, -0.7037298423582233342 ) ) ;
#42221 = AXIS2_PLACEMENT_3D ( 'NONE', #7810, #23550, #34057 ) ;
#42222 = ORIENTED_EDGE ( 'NONE', *, *, #13217, .F. ) ;
#42223 = VERTEX_POINT ( 'NONE', #27457 ) ;
#42224 = CARTESIAN_POINT ( 'NONE',  ( 2.150824344285287459, 1.742351338968239238, -0.8657870173518766865 ) ) ;
#42225 = CARTESIAN_POINT ( 'NONE',  ( 1.062992125984251635, 0.4724409448818890911, 1.181102362204724088 ) ) ;
#42226 = VECTOR ( 'NONE', #18189, 39.37007874015748143 ) ;
#42227 = PLANE ( 'NONE',  #11209 ) ;
#42228 = ADVANCED_FACE ( 'NONE', ( #39342 ), #39399, .T. ) ;
#42229 = PLANE ( 'NONE',  #26890 ) ;
#42230 = DIRECTION ( 'NONE',  ( 0.01601477604151182663, -0.9998717552508123996, 0.000000000000000000 ) ) ;
#42231 = VECTOR ( 'NONE', #22413, 39.37007874015748143 ) ;
#42232 = ADVANCED_FACE ( 'NONE', ( #3215 ), #38841, .F. ) ;
#42233 = ORIENTED_EDGE ( 'NONE', *, *, #34591, .T. ) ;
#42234 = ORIENTED_EDGE ( 'NONE', *, *, #39146, .F. ) ;
#42235 = CARTESIAN_POINT ( 'NONE',  ( -2.708693778673423758, 1.578604444535609108, -1.175591149347226194 ) ) ;
#42236 = EDGE_CURVE ( 'NONE', #48626, #30224, #18415, .T. ) ;
#42237 = FACE_OUTER_BOUND ( 'NONE', #21682, .T. ) ;
#42238 = EDGE_LOOP ( 'NONE', ( #29037, #7520, #13619, #35246 ) ) ;
#42239 = EDGE_CURVE ( 'NONE', #38076, #36543, #11475, .T. ) ;
#42240 = DIRECTION ( 'NONE',  ( -3.469446951953613696E-16, 0.000000000000000000, -1.000000000000000000 ) ) ;
#42241 = EDGE_LOOP ( 'NONE', ( #7565, #30552, #41274, #25980 ) ) ;
#42242 = ORIENTED_EDGE ( 'NONE', *, *, #23933, .F. ) ;
#42243 = ORIENTED_EDGE ( 'NONE', *, *, #2747, .F. ) ;
#42244 = ORIENTED_EDGE ( 'NONE', *, *, #49204, .T. ) ;
#42245 = CARTESIAN_POINT ( 'NONE',  ( -2.164823134740036181, 1.574803149606301966, 0.000000000000000000 ) ) ;
#42246 = DIRECTION ( 'NONE',  ( 1.000000000000000000, 0.000000000000000000, -3.469446951953613696E-16 ) ) ;
#42247 = DIRECTION ( 'NONE',  ( 1.000000000000000000, -0.000000000000000000, 0.000000000000000000 ) ) ;
#42248 = AXIS2_PLACEMENT_3D ( 'NONE', #18883, #18634, #50813 ) ;
#42249 =( BOUNDED_CURVE ( )  B_SPLINE_CURVE ( 3, ( #6805, #18687, #42420, #7063 ),
 .UNSPECIFIED., .F., .F. ) 
 B_SPLINE_CURVE_WITH_KNOTS ( ( 4, 4 ),
 ( 5.231528604247587033, 5.282403893493373026 ),
 .UNSPECIFIED. ) 
 CURVE ( )  GEOMETRIC_REPRESENTATION_ITEM ( )  RATIONAL_B_SPLINE_CURVE ( ( 1.000000000000000000, 0.9997843203757749153, 0.9997843203757749153, 1.000000000000000000 ) ) 
 REPRESENTATION_ITEM ( '' )  );
#42250 = CARTESIAN_POINT ( 'NONE',  ( -1.152568299495734694, 6.692913385826772199, 1.833124570921535801 ) ) ;
#42251 = CONICAL_SURFACE ( 'NONE', #32365, 1.850107469027523210, 0.6386652850508578450 ) ;
#42252 = DIRECTION ( 'NONE',  ( 0.000000000000000000, 0.000000000000000000, 1.000000000000000000 ) ) ;
#42253 = CARTESIAN_POINT ( 'NONE',  ( 0.5455278134075213226, 3.267716535433071279, -9.463399047163221947E-17 ) ) ;
#42254 = EDGE_LOOP ( 'NONE', ( #46975, #49604, #12805, #49750 ) ) ;
#42255 = LINE ( 'NONE', #46612, #39845 ) ;
#42256 = PLANE ( 'NONE',  #31621 ) ;
#42257 = AXIS2_PLACEMENT_3D ( 'NONE', #28716, #5225, #35968 ) ;
#42258 = LINE ( 'NONE', #50214, #20213 ) ;
#42259 = CARTESIAN_POINT ( 'NONE',  ( 1.625502936149584077, 0.000000000000000000, 1.317350029429052771 ) ) ;
#42260 = CIRCLE ( 'NONE', #24957, 2.165354330708661568 ) ;
#42261 = AXIS2_PLACEMENT_3D ( 'NONE', #43887, #8538, #40037 ) ;
#42262 = VERTEX_POINT ( 'NONE', #43197 ) ;
#42263 = LINE ( 'NONE', #31161, #3388 ) ;
#42264 = EDGE_CURVE ( 'NONE', #43429, #35595, #26955, .T. ) ;
#42265 = CARTESIAN_POINT ( 'NONE',  ( -1.985260859929298016, 3.267716535433071279, -0.9448818897637762948 ) ) ;
#42266 = ORIENTED_EDGE ( 'NONE', *, *, #35647, .T. ) ;
#42267 = DIRECTION ( 'NONE',  ( -0.000000000000000000, 1.000000000000000000, -0.000000000000000000 ) ) ;
#42268 = LINE ( 'NONE', #14912, #27553 ) ;
#42269 = EDGE_CURVE ( 'NONE', #41945, #11695, #23089, .T. ) ;
#42270 = ORIENTED_EDGE ( 'NONE', *, *, #3778, .T. ) ;
#42271 = EDGE_CURVE ( 'NONE', #30486, #7592, #19209, .T. ) ;
#42272 = LINE ( 'NONE', #22663, #27364 ) ;
#42273 = ORIENTED_EDGE ( 'NONE', *, *, #4908, .T. ) ;
#42274 = PLANE ( 'NONE',  #23948 ) ;
#42275 = EDGE_CURVE ( 'NONE', #39958, #373, #19457, .T. ) ;
#42276 = FACE_OUTER_BOUND ( 'NONE', #11454, .T. ) ;
#42277 = DIRECTION ( 'NONE',  ( 1.734723475976806848E-16, 0.000000000000000000, 1.000000000000000000 ) ) ;
#42278 = LINE ( 'NONE', #46877, #11888 ) ;
#42279 = PLANE ( 'NONE',  #14567 ) ;
#42280 = ORIENTED_EDGE ( 'NONE', *, *, #24751, .T. ) ;
#42281 = CARTESIAN_POINT ( 'NONE',  ( 0.2727639067037604947, 3.346456692913386100, -0.4724409448818886470 ) ) ;
#42282 = EDGE_LOOP ( 'NONE', ( #16582, #5876, #5797, #37221 ) ) ;
#42283 = EDGE_LOOP ( 'NONE', ( #29558, #704, #6658, #19146 ) ) ;
#42284 = LINE ( 'NONE', #50482, #13083 ) ;
#42285 = VERTEX_POINT ( 'NONE', #26455 ) ;
#42286 = CARTESIAN_POINT ( 'NONE',  ( 1.363819533518803251, 0.000000000000000000, -0.1574803149606304187 ) ) ;
#42287 = EDGE_CURVE ( 'NONE', #30224, #17224, #584, .T. ) ;
#42288 = CARTESIAN_POINT ( 'NONE',  ( 0.8949303405208902662, 6.692913385826772199, -1.971765468592529880 ) ) ;
#42289 = ORIENTED_EDGE ( 'NONE', *, *, #48756, .F. ) ;
#42290 = FACE_OUTER_BOUND ( 'NONE', #35344, .T. ) ;
#42291 = EDGE_CURVE ( 'NONE', #46532, #10670, #42200, .T. ) ;
#42292 = DIRECTION ( 'NONE',  ( 0.000000000000000000, -1.000000000000000000, 0.000000000000000000 ) ) ;
#42293 = VECTOR ( 'NONE', #31069, 39.37007874015748143 ) ;
#42294 = DIRECTION ( 'NONE',  ( -0.000000000000000000, 0.000000000000000000, 1.000000000000000000 ) ) ;
#42295 = VERTEX_POINT ( 'NONE', #5246 ) ;
#42296 = VERTEX_POINT ( 'NONE', #24621 ) ;
#42297 = EDGE_CURVE ( 'NONE', #20924, #344, #93, .T. ) ;
#42298 = CYLINDRICAL_SURFACE ( 'NONE', #7547, 2.164630168518208109 ) ;
#42299 = FACE_BOUND ( 'NONE', #40284, .T. ) ;
#42300 = VERTEX_POINT ( 'NONE', #27970 ) ;
#42301 = VECTOR ( 'NONE', #34392, 39.37007874015748143 ) ;
#42302 = VECTOR ( 'NONE', #24746, 39.37007874015748143 ) ;
#42303 = DIRECTION ( 'NONE',  ( 1.000000000000000000, 0.000000000000000000, 0.000000000000000000 ) ) ;
#42304 = VERTEX_POINT ( 'NONE', #13005 ) ;
#42305 = EDGE_LOOP ( 'NONE', ( #33254, #29799, #17999, #29330 ) ) ;
#42306 = B_SPLINE_CURVE_WITH_KNOTS ( 'NONE', 3,
 ( #14461, #30205, #45925, #10590 ),
 .UNSPECIFIED., .F., .F.,
 ( 4, 4 ),
 ( 2.137724770886416802E-07, 0.002500774150297437569 ),
 .UNSPECIFIED. ) ;
#42307 = PLANE ( 'NONE',  #41421 ) ;
#42308 = AXIS2_PLACEMENT_3D ( 'NONE', #32964, #45546, #48640 ) ;
#42309 = DIRECTION ( 'NONE',  ( -0.000000000000000000, -1.000000000000000000, -0.000000000000000000 ) ) ;
#42310 = ORIENTED_EDGE ( 'NONE', *, *, #13681, .F. ) ;
#42311 = CARTESIAN_POINT ( 'NONE',  ( -2.182111253630085290, 3.346456692913386100, 0.9448818897637749625 ) ) ;
#42312 = ORIENTED_EDGE ( 'NONE', *, *, #37240, .T. ) ;
#42313 = DIRECTION ( 'NONE',  ( 1.734723475976806848E-16, -0.000000000000000000, 1.000000000000000000 ) ) ;
#42314 = LINE ( 'NONE', #35339, #37424 ) ;
#42315 = DIRECTION ( 'NONE',  ( -1.000000000000000000, 0.000000000000000000, 0.000000000000000000 ) ) ;
#42316 = ORIENTED_EDGE ( 'NONE', *, *, #262, .T. ) ;
#42317 = EDGE_LOOP ( 'NONE', ( #24779, #2564, #10291, #33765 ) ) ;
#42318 = DIRECTION ( 'NONE',  ( 1.000000000000000000, 0.000000000000000000, 0.000000000000000000 ) ) ;
#42319 = CARTESIAN_POINT ( 'NONE',  ( -1.166969139818015533, 0.000000000000000000, 0.1574803149606287811 ) ) ;
#42320 = LINE ( 'NONE', #6965, #29931 ) ;
#42321 = CARTESIAN_POINT ( 'NONE',  ( 0.1155636338427008941, -0.5222242541845523167, 0.000000000000000000 ) ) ;
#42322 = CARTESIAN_POINT ( 'NONE',  ( 2.164658444855302122, 5.905511811023623991, -0.04795272066889885720 ) ) ;
#42323 = CARTESIAN_POINT ( 'NONE',  ( 1.372667653987894809, 0.000000000000000000, 1.546304799276380981 ) ) ;
#42324 = LINE ( 'NONE', #2086, #27513 ) ;
#42325 = VECTOR ( 'NONE', #27367, 39.37007874015748143 ) ;
#42326 = ADVANCED_FACE ( 'NONE', ( #613 ), #48325, .F. ) ;
#42327 = ORIENTED_EDGE ( 'NONE', *, *, #20123, .T. ) ;
#42328 = DIRECTION ( 'NONE',  ( 0.000000000000000000, -0.000000000000000000, 1.000000000000000000 ) ) ;
#42329 = DIRECTION ( 'NONE',  ( -0.000000000000000000, 1.000000000000000000, -0.000000000000000000 ) ) ;
#42330 = EDGE_CURVE ( 'NONE', #41046, #795, #16624, .T. ) ;
#42331 = AXIS2_PLACEMENT_3D ( 'NONE', #6087, #18221, #33733 ) ;
#42332 = VERTEX_POINT ( 'NONE', #40378 ) ;
#42333 = EDGE_CURVE ( 'NONE', #26538, #39358, #28737, .T. ) ;
#42334 = CIRCLE ( 'NONE', #11819, 2.165354330708661568 ) ;
#42335 = VERTEX_POINT ( 'NONE', #36246 ) ;
#42337 = VECTOR ( 'NONE', #37395, 39.37007874015748854 ) ;
#42336 = CARTESIAN_POINT ( 'NONE',  ( 1.068075307999459822, 6.692913385826772199, 1.883606783264653028 ) ) ;
#42338 = CARTESIAN_POINT ( 'NONE',  ( 0.8314045656493375125, 1.724861346829795750, 2.355326812497060107 ) ) ;
#42339 = ORIENTED_EDGE ( 'NONE', *, *, #43569, .T. ) ;
#42340 = EDGE_CURVE ( 'NONE', #30098, #39633, #8612, .T. ) ;
#42341 = VECTOR ( 'NONE', #33406, 39.37007874015748143 ) ;
#42342 = ORIENTED_EDGE ( 'NONE', *, *, #39649, .T. ) ;
#42343 = CARTESIAN_POINT ( 'NONE',  ( -0.8182917201112819283, 3.346456692913386100, -1.299212598425193210 ) ) ;
#42344 = VERTEX_POINT ( 'NONE', #40625 ) ;
#42345 = LINE ( 'NONE', #41848, #48233 ) ;
#42346 = LINE ( 'NONE', #38741, #6612 ) ;
#42347 = EDGE_CURVE ( 'NONE', #15273, #919, #39598, .T. ) ;
#42348 = ORIENTED_EDGE ( 'NONE', *, *, #37768, .T. ) ;
#42349 = LINE ( 'NONE', #38496, #5705 ) ;
#42350 = EDGE_LOOP ( 'NONE', ( #49677, #28313, #7646, #10319 ) ) ;
#42351 = ORIENTED_EDGE ( 'NONE', *, *, #14442, .F. ) ;
#42352 = EDGE_CURVE ( 'NONE', #5817, #4778, #35724, .T. ) ;
#42353 = DIRECTION ( 'NONE',  ( -1.000000000000000000, 0.000000000000000000, 1.734723475976806848E-16 ) ) ;
#42354 = CARTESIAN_POINT ( 'NONE',  ( 1.325491792074624087, 1.641458297549746037, -2.638988599164732385 ) ) ;
#42355 = DIRECTION ( 'NONE',  ( -0.000000000000000000, 1.000000000000000000, -0.000000000000000000 ) ) ;
#42356 = FACE_OUTER_BOUND ( 'NONE', #29129, .T. ) ;
#42357 = EDGE_LOOP ( 'NONE', ( #38505, #37660, #21316, #15644 ) ) ;
#42358 = CARTESIAN_POINT ( 'NONE',  ( 2.808237744965994320, 5.905511811023623991, 0.9124517550441686442 ) ) ;
#42359 = PLANE ( 'NONE',  #36560 ) ;
#42360 = DIRECTION ( 'NONE',  ( -0.000000000000000000, 1.000000000000000000, -0.000000000000000000 ) ) ;
#42361 = ORIENTED_EDGE ( 'NONE', *, *, #11485, .F. ) ;
#42362 = DIRECTION ( 'NONE',  ( 1.000000000000000000, 0.000000000000000000, 0.000000000000000000 ) ) ;
#42363 = VECTOR ( 'NONE', #27443, 39.37007874015748143 ) ;
#42364 = AXIS2_PLACEMENT_3D ( 'NONE', #24682, #4038, #31926 ) ;
#42365 = ORIENTED_EDGE ( 'NONE', *, *, #13967, .F. ) ;
#42366 = VECTOR ( 'NONE', #41524, 39.37007874015748143 ) ;
#42367 = VERTEX_POINT ( 'NONE', #31600 ) ;
#42368 = EDGE_CURVE ( 'NONE', #34396, #32442, #27713, .T. ) ;
#42369 = LINE ( 'NONE', #39517, #26789 ) ;
#42370 = AXIS2_PLACEMENT_3D ( 'NONE', #26832, #43075, #19839 ) ;
#42371 = CARTESIAN_POINT ( 'NONE',  ( 0.000000000000000000, 3.267716535433071279, 0.9448818897637746295 ) ) ;
#42372 = CARTESIAN_POINT ( 'NONE',  ( 0.4696143004045478797, 0.000000000000000000, -1.299212598425193210 ) ) ;
#42373 = FACE_OUTER_BOUND ( 'NONE', #46871, .T. ) ;
#42374 = ORIENTED_EDGE ( 'NONE', *, *, #21837, .F. ) ;
#42375 = ORIENTED_EDGE ( 'NONE', *, *, #6912, .F. ) ;
#42376 = VECTOR ( 'NONE', #50528, 39.37007874015748143 ) ;
#42377 = CARTESIAN_POINT ( 'NONE',  ( -0.2727639067037602172, 3.346456692913386100, 1.417322834645662777 ) ) ;
#42378 = CARTESIAN_POINT ( 'NONE',  ( 0.2727639067037605503, 3.267716535433071279, -4.731699523581609741E-17 ) ) ;
#42379 = ORIENTED_EDGE ( 'NONE', *, *, #38114, .T. ) ;
#42380 = DIRECTION ( 'NONE',  ( 0.000000000000000000, 1.000000000000000000, 0.000000000000000000 ) ) ;
#42381 = CARTESIAN_POINT ( 'NONE',  ( -0.8942052331142552601, 3.267716535433071279, -0.1968503937007881899 ) ) ;
#42382 = CARTESIAN_POINT ( 'NONE',  ( 2.138649790787681138, 0.000000000000000000, -0.1124749717369803448 ) ) ;
#42383 = CARTESIAN_POINT ( 'NONE',  ( 0.8182917201112824834, 3.346456692913386100, 1.732283464566921172 ) ) ;
#42384 = LINE ( 'NONE', #14527, #40255 ) ;
#42385 = VERTEX_POINT ( 'NONE', #12746 ) ;
#42386 = CARTESIAN_POINT ( 'NONE',  ( 2.437180031585944207, 1.658768335924418080, -1.667735833703099191 ) ) ;
#42387 = DIRECTION ( 'NONE',  ( -0.000000000000000000, 1.000000000000000000, -0.000000000000000000 ) ) ;
#42388 = ADVANCED_FACE ( 'NONE', ( #20222 ), #16104, .F. ) ;
#42389 = DIRECTION ( 'NONE',  ( -0.9998717552508122886, -0.01601477604151181275, 0.000000000000000000 ) ) ;
#42390 = ADVANCED_FACE ( 'NONE', ( #20998 ), #4744, .F. ) ;
#42391 = ORIENTED_EDGE ( 'NONE', *, *, #20431, .F. ) ;
#42392 = DIRECTION ( 'NONE',  ( -3.469446951953613696E-16, 0.000000000000000000, -1.000000000000000000 ) ) ;
#42393 = CARTESIAN_POINT ( 'NONE',  ( -0.7145799201509080989, 6.692913385826772199, 2.044048657746648789 ) ) ;
#42394 = LINE ( 'NONE', #18666, #20538 ) ;
#42395 = EDGE_CURVE ( 'NONE', #45868, #24633, #28222, .T. ) ;
#42396 = ORIENTED_EDGE ( 'NONE', *, *, #29572, .T. ) ;
#42397 = EDGE_CURVE ( 'NONE', #17674, #2006, #47558, .T. ) ;
#42398 = DIRECTION ( 'NONE',  ( -1.000000000000000000, 0.000000000000000000, -0.000000000000000000 ) ) ;
#42399 = AXIS2_PLACEMENT_3D ( 'NONE', #14829, #30576, #48307 ) ;
#42400 = VECTOR ( 'NONE', #8864, 39.37007874015748143 ) ;
#42401 = ORIENTED_EDGE ( 'NONE', *, *, #4287, .T. ) ;
#42402 = VECTOR ( 'NONE', #33487, 39.37007874015748143 ) ;
#42403 = CARTESIAN_POINT ( 'NONE',  ( -0.2438126009205185685, 0.000000000000000000, -0.2787034377076138547 ) ) ;
#42404 = EDGE_LOOP ( 'NONE', ( #32227, #24417, #18540, #2516 ) ) ;
#42405 = DIRECTION ( 'NONE',  ( 1.000000000000000000, 0.000000000000000000, -3.469446951953613696E-16 ) ) ;
#42406 = VECTOR ( 'NONE', #6419, 39.37007874015748143 ) ;
#42407 = EDGE_LOOP ( 'NONE', ( #47352, #14721, #27110, #27230 ) ) ;
#42408 = CIRCLE ( 'NONE', #39952, 2.164630168518208109 ) ;
#42409 = CARTESIAN_POINT ( 'NONE',  ( -1.772999178993743152, 5.118110236220475784, -1.009977129983215427 ) ) ;
#42410 = LINE ( 'NONE', #22044, #24736 ) ;
#42411 = CARTESIAN_POINT ( 'NONE',  ( -1.712496953225537188, 0.000000000000000000, -0.3543307086614171930 ) ) ;
#42412 = EDGE_CURVE ( 'NONE', #8577, #33170, #43965, .T. ) ;
#42413 = VERTEX_POINT ( 'NONE', #24364 ) ;
#42414 = ORIENTED_EDGE ( 'NONE', *, *, #259, .F. ) ;
#42415 = ORIENTED_EDGE ( 'NONE', *, *, #48601, .T. ) ;
#42416 = LINE ( 'NONE', #10680, #10898 ) ;
#42417 = PLANE ( 'NONE',  #18889 ) ;
#42418 = ORIENTED_EDGE ( 'NONE', *, *, #43800, .F. ) ;
#42419 = EDGE_CURVE ( 'NONE', #721, #46932, #24106, .T. ) ;
#42420 = CARTESIAN_POINT ( 'NONE',  ( 1.219713223144859748, 0.000000000000000000, -1.650995057222538254 ) ) ;
#42421 = CARTESIAN_POINT ( 'NONE',  ( 1.958513403246152640, 1.640845930445798073, -1.233835998176425308 ) ) ;
#42422 = CARTESIAN_POINT ( 'NONE',  ( 0.000000000000000000, 3.346456692913386100, 0.000000000000000000 ) ) ;
#42423 = B_SPLINE_CURVE_WITH_KNOTS ( 'NONE', 3,
 ( #5930, #17807, #41555, #14184 ),
 .UNSPECIFIED., .F., .F.,
 ( 4, 4 ),
 ( 3.460281517023109080E-07, 0.04793831677642486355 ),
 .UNSPECIFIED. ) ;
#42424 = VERTEX_POINT ( 'NONE', #36754 ) ;
#42425 = ORIENTED_EDGE ( 'NONE', *, *, #36990, .F. ) ;
#42426 = CARTESIAN_POINT ( 'NONE',  ( 0.1067246931122726866, 0.02962905676920215767, 0.000000000000000000 ) ) ;
#42427 = DIRECTION ( 'NONE',  ( 1.734723475976806848E-16, 0.000000000000000000, 1.000000000000000000 ) ) ;
#42428 = EDGE_CURVE ( 'NONE', #28289, #6369, #48828, .T. ) ;
#42429 = CARTESIAN_POINT ( 'NONE',  ( 1.599172890215259546, 0.000000000000000000, 1.460879300779193590 ) ) ;
#42430 = ORIENTED_EDGE ( 'NONE', *, *, #35514, .F. ) ;
#42431 = DIRECTION ( 'NONE',  ( -0.000000000000000000, 1.000000000000000000, -0.000000000000000000 ) ) ;
#42432 = DIRECTION ( 'NONE',  ( -0.000000000000000000, -1.000000000000000000, -0.000000000000000000 ) ) ;
#42433 = B_SPLINE_CURVE_WITH_KNOTS ( 'NONE', 3,
 ( #23159, #33794, #14408, #42533 ),
 .UNSPECIFIED., .F., .F.,
 ( 4, 4 ),
 ( 0.01179318187808457187, 0.03073709326239987966 ),
 .UNSPECIFIED. ) ;
#42434 = VERTEX_POINT ( 'NONE', #2144 ) ;
#42435 = CARTESIAN_POINT ( 'NONE',  ( 0.8182917201112817063, 0.000000000000000000, -1.614173228346451605 ) ) ;
#42436 = ORIENTED_EDGE ( 'NONE', *, *, #14482, .T. ) ;
#42437 = ORIENTED_EDGE ( 'NONE', *, *, #42683, .T. ) ;
#42438 = CARTESIAN_POINT ( 'NONE',  ( 1.091055626815042423, 0.000000000000000000, -1.456692913385822630 ) ) ;
#42439 = DIRECTION ( 'NONE',  ( -1.000000000000000000, 0.000000000000000000, 0.000000000000000000 ) ) ;
#42440 = EDGE_CURVE ( 'NONE', #30165, #18246, #45164, .T. ) ;
#42441 = CARTESIAN_POINT ( 'NONE',  ( -1.738955188402737440, 0.000000000000000000, -0.1273587697465547175 ) ) ;
#42442 = CARTESIAN_POINT ( 'NONE',  ( -2.454875160333845674, 3.241704813874235480, 0.09245170100039766525 ) ) ;
#42443 = LINE ( 'NONE', #19703, #30445 ) ;
#42444 = VERTEX_POINT ( 'NONE', #9379 ) ;
#42445 = VECTOR ( 'NONE', #36687, 39.37007874015748143 ) ;
#42446 = ADVANCED_FACE ( 'NONE', ( #17381 ), #22131, .T. ) ;
#42447 = VECTOR ( 'NONE', #44417, 39.37007874015748143 ) ;
#42448 = ORIENTED_EDGE ( 'NONE', *, *, #7192, .T. ) ;
#42449 = CARTESIAN_POINT ( 'NONE',  ( -0.8182917201112814842, 3.346456692913386100, 1.417322834645662777 ) ) ;
#42450 = CARTESIAN_POINT ( 'NONE',  ( -2.277873973731453727, 1.683757167080951245, 1.879489153247634992 ) ) ;
#42451 = VECTOR ( 'NONE', #21023, 39.37007874015748143 ) ;
#42452 = ADVANCED_FACE ( 'NONE', ( #33651 ), #33403, .T. ) ;
#42453 = CARTESIAN_POINT ( 'NONE',  ( 2.106197740627111514, 3.346456692913386100, -1.102362204724406602 ) ) ;
#42454 = DIRECTION ( 'NONE',  ( -1.000000000000000000, 0.000000000000000000, -0.000000000000000000 ) ) ;
#42455 = AXIS2_PLACEMENT_3D ( 'NONE', #34635, #7766, #39007 ) ;
#42456 = ORIENTED_EDGE ( 'NONE', *, *, #13683, .F. ) ;
#42457 = LINE ( 'NONE', #42707, #30823 ) ;
#42458 = CARTESIAN_POINT ( 'NONE',  ( 0.000000000000000000, 3.267716535433071279, -0.3149606299212589500 ) ) ;
#42459 = ADVANCED_FACE ( 'NONE', ( #49342 ), #13512, .T. ) ;
#42460 = EDGE_LOOP ( 'NONE', ( #32839, #16839, #44551, #14183 ) ) ;
#42461 = DIRECTION ( 'NONE',  ( -0.000000000000000000, 1.000000000000000000, -0.000000000000000000 ) ) ;
#42462 = PLANE ( 'NONE',  #3890 ) ;
#42463 = CARTESIAN_POINT ( 'NONE',  ( -1.175769893759974538, 0.000000000000000000, 1.370616677507177972 ) ) ;
#42464 = CARTESIAN_POINT ( 'NONE',  ( -1.547114303032252502, 1.584696887024839906, -1.547279266820049237 ) ) ;
#42465 = ADVANCED_FACE ( 'NONE', ( #33144 ), #3137, .T. ) ;
#42466 = DIRECTION ( 'NONE',  ( 2.866708903754509961E-17, 1.000000000000000000, -1.255987235303920130E-16 ) ) ;
#42467 = EDGE_CURVE ( 'NONE', #29752, #31368, #10142, .T. ) ;
#42468 = CARTESIAN_POINT ( 'NONE',  ( 0.000000000000000000, 3.267716535433071279, 1.102362204724404160 ) ) ;
#42469 = VERTEX_POINT ( 'NONE', #10401 ) ;
#42470 = DIRECTION ( 'NONE',  ( -3.469446951953613696E-16, 0.000000000000000000, -1.000000000000000000 ) ) ;
#42471 = ORIENTED_EDGE ( 'NONE', *, *, #45281, .F. ) ;
#42472 = FACE_OUTER_BOUND ( 'NONE', #50574, .T. ) ;
#42473 = CARTESIAN_POINT ( 'NONE',  ( -0.8182917201112819283, 0.000000000000000000, -1.929133858267710000 ) ) ;
#42474 = CARTESIAN_POINT ( 'NONE',  ( 0.4330136603435738585, 0.5160455853568214346, -1.535490276664301046 ) ) ;
#42475 = VERTEX_POINT ( 'NONE', #33901 ) ;
#42476 = ORIENTED_EDGE ( 'NONE', *, *, #16038, .T. ) ;
#42477 = CARTESIAN_POINT ( 'NONE',  ( 1.953585199828835828, 3.346456692913386100, 0.7874015748031456541 ) ) ;
#42478 = VECTOR ( 'NONE', #15969, 39.37007874015748143 ) ;
#42479 = DIRECTION ( 'NONE',  ( 0.1785568947986229116, 0.000000000000000000, 0.9839295885986321100 ) ) ;
#42480 = B_SPLINE_CURVE_WITH_KNOTS ( 'NONE', 3,
 ( #33137, #17126, #29506, #25373 ),
 .UNSPECIFIED., .F., .F.,
 ( 4, 4 ),
 ( 3.370817529537171183E-07, 0.05037949722401796615 ),
 .UNSPECIFIED. ) ;
#42481 = VECTOR ( 'NONE', #23666, 39.37007874015748143 ) ;
#42482 = VECTOR ( 'NONE', #19334, 39.37007874015748143 ) ;
#42483 = LINE ( 'NONE', #11502, #15948 ) ;
#42484 = CARTESIAN_POINT ( 'NONE',  ( 0.5662636741187413447, 0.000000000000000000, 1.648861433446464186 ) ) ;
#42485 = CARTESIAN_POINT ( 'NONE',  ( -0.07591351300297333182, 3.346456692913386100, -0.7874015748031470974 ) ) ;
#42486 = VECTOR ( 'NONE', #2606, 39.37007874015748143 ) ;
#42487 = DIRECTION ( 'NONE',  ( -3.469446951953613696E-16, 0.000000000000000000, -1.000000000000000000 ) ) ;
#42488 = ORIENTED_EDGE ( 'NONE', *, *, #27237, .F. ) ;
#42489 = DIRECTION ( 'NONE',  ( 0.000000000000000000, -1.000000000000000000, 0.000000000000000000 ) ) ;
#42490 = DIRECTION ( 'NONE',  ( -0.000000000000000000, 1.000000000000000000, -0.000000000000000000 ) ) ;
#42491 = EDGE_CURVE ( 'NONE', #19150, #38271, #45450, .T. ) ;
#42492 = CARTESIAN_POINT ( 'NONE',  ( 2.706338173250262269, 5.118110236220475784, -1.181102362204724310 ) ) ;
#42493 = AXIS2_PLACEMENT_3D ( 'NONE', #5082, #13094, #20831 ) ;
#42494 = ORIENTED_EDGE ( 'NONE', *, *, #49675, .F. ) ;
#42495 = DIRECTION ( 'NONE',  ( -0.9998717552508121775, -0.01601477604151182316, 0.000000000000000000 ) ) ;
#42496 = VERTEX_POINT ( 'NONE', #21766 ) ;
#42497 = VERTEX_POINT ( 'NONE', #37015 ) ;
#42498 = EDGE_CURVE ( 'NONE', #2006, #970, #40878, .T. ) ;
#42499 = EDGE_CURVE ( 'NONE', #2677, #14952, #9638, .T. ) ;
#42500 = EDGE_CURVE ( 'NONE', #46482, #44152, #13258, .T. ) ;
#42501 = ORIENTED_EDGE ( 'NONE', *, *, #31984, .T. ) ;
#42502 = ORIENTED_EDGE ( 'NONE', *, *, #32735, .T. ) ;
#42503 = CARTESIAN_POINT ( 'NONE',  ( 0.5544985201248122664, 1.716783259433079856, -2.194164409418295048 ) ) ;
#42504 = B_SPLINE_CURVE_WITH_KNOTS ( 'NONE', 3,
 ( #46593, #38636, #11512, #27246 ),
 .UNSPECIFIED., .F., .F.,
 ( 4, 4 ),
 ( 0.1211775127643062860, 0.1625894504277921315 ),
 .UNSPECIFIED. ) ;
#42505 = B_SPLINE_CURVE_WITH_KNOTS ( 'NONE', 3,
 ( #37533, #9900, #2153, #33662 ),
 .UNSPECIFIED., .F., .F.,
 ( 4, 4 ),
 ( 2.471499816278681188E-07, 0.002500687884645799025 ),
 .UNSPECIFIED. ) ;
#42506 = CARTESIAN_POINT ( 'NONE',  ( -2.793030215715272213, 1.577298709702483093, 0.9592557174602283077 ) ) ;
#42507 = CARTESIAN_POINT ( 'NONE',  ( 0.5455278134075217666, 0.000000000000000000, 1.574803149606291974 ) ) ;
#42508 = DIRECTION ( 'NONE',  ( -0.000000000000000000, 1.000000000000000000, -0.000000000000000000 ) ) ;
#42509 = EDGE_CURVE ( 'NONE', #4391, #33442, #13066, .T. ) ;
#42510 = DIRECTION ( 'NONE',  ( 0.01601477604151182663, -0.9998717552508123996, 0.000000000000000000 ) ) ;
#42511 = CARTESIAN_POINT ( 'NONE',  ( 1.645881266606342708, 1.741324525431280135, -2.181635745336127474 ) ) ;
#42512 = AXIS2_PLACEMENT_3D ( 'NONE', #15538, #46984, #11656 ) ;
#42513 = ORIENTED_EDGE ( 'NONE', *, *, #24296, .T. ) ;
#42514 = DIRECTION ( 'NONE',  ( -3.986037398843765983E-20, -1.000000000000000000, -1.160734090543304660E-16 ) ) ;
#42515 = CARTESIAN_POINT ( 'NONE',  ( -1.780101451746625152, 0.000000000000000000, 1.234002060668493828 ) ) ;
#42516 = CARTESIAN_POINT ( 'NONE',  ( 2.182111253630085290, 3.346456692913386100, -0.3149606299212596716 ) ) ;
#42517 = VECTOR ( 'NONE', #14621, 39.37007874015748143 ) ;
#42518 = FACE_OUTER_BOUND ( 'NONE', #19124, .T. ) ;
#42519 = EDGE_CURVE ( 'NONE', #26476, #15306, #29511, .T. ) ;
#42520 = ORIENTED_EDGE ( 'NONE', *, *, #27918, .F. ) ;
#42521 = CARTESIAN_POINT ( 'NONE',  ( -1.636583440222563635, 0.000000000000000000, 0.7480314960629874665 ) ) ;
#42522 = DIRECTION ( 'NONE',  ( -1.000000000000000000, 0.000000000000000000, 0.000000000000000000 ) ) ;
#42523 = ORIENTED_EDGE ( 'NONE', *, *, #25909, .T. ) ;
#42524 = CARTESIAN_POINT ( 'NONE',  ( 0.2727639067037610499, 3.346456692913386100, 2.362204724409437961 ) ) ;
#42525 = CIRCLE ( 'NONE', #26023, 2.164630168518208109 ) ;
#42526 = ADVANCED_FACE ( 'NONE', ( #44729 ), #2401, .F. ) ;
#42527 = FACE_OUTER_BOUND ( 'NONE', #23629, .T. ) ;
#42528 = EDGE_CURVE ( 'NONE', #43953, #37676, #1631, .T. ) ;
#42529 = AXIS2_PLACEMENT_3D ( 'NONE', #2426, #22299, #18168 ) ;
#42530 = EDGE_CURVE ( 'NONE', #23553, #5850, #41386, .T. ) ;
#42531 = CARTESIAN_POINT ( 'NONE',  ( 1.091055626815042645, 3.346456692913386100, -0.3149606299212596716 ) ) ;
#42532 = VERTEX_POINT ( 'NONE', #50337 ) ;
#42533 = CARTESIAN_POINT ( 'NONE',  ( -1.325491792074585451, 1.698604322780517650, -2.638988599164751481 ) ) ;
#42534 = CARTESIAN_POINT ( 'NONE',  ( 0.7423782071083085965, 0.000000000000000000, 0.4330708661417287386 ) ) ;
#42535 = DIRECTION ( 'NONE',  ( -0.9998717552508122886, -0.01601477604151185785, 0.000000000000000000 ) ) ;
#42536 = LINE ( 'NONE', #7176, #4492 ) ;
#42537 = CARTESIAN_POINT ( 'NONE',  ( 2.151809081513405442, 6.692913385826772199, 0.2418202932658665705 ) ) ;
#42538 = ORIENTED_EDGE ( 'NONE', *, *, #37474, .T. ) ;
#42539 = DIRECTION ( 'NONE',  ( -1.000000000000000000, 0.000000000000000000, 0.000000000000000000 ) ) ;
#42540 = EDGE_LOOP ( 'NONE', ( #50734, #36453, #20602, #35012 ) ) ;
#42541 = ORIENTED_EDGE ( 'NONE', *, *, #27058, .F. ) ;
#42542 = CYLINDRICAL_SURFACE ( 'NONE', #37816, 2.164630168518208109 ) ;
#42543 = ORIENTED_EDGE ( 'NONE', *, *, #917, .F. ) ;
#42544 = LINE ( 'NONE', #22428, #46042 ) ;
#42545 = DIRECTION ( 'NONE',  ( 1.734723475976806848E-16, 0.000000000000000000, 1.000000000000000000 ) ) ;
#42546 = VERTEX_POINT ( 'NONE', #39026 ) ;
#42547 = DIRECTION ( 'NONE',  ( -0.000000000000000000, 0.000000000000000000, 1.000000000000000000 ) ) ;
#42548 = CARTESIAN_POINT ( 'NONE',  ( 0.000000000000000000, 3.267716535433071279, 0.6299212598425161236 ) ) ;
#42549 = VECTOR ( 'NONE', #47747, 39.37007874015748143 ) ;
#42550 = DIRECTION ( 'NONE',  ( -0.9465353838348410376, 0.000000000000000000, -0.3226000110797114240 ) ) ;
#42551 = VECTOR ( 'NONE', #12949, 39.37007874015748143 ) ;
#42552 = ORIENTED_EDGE ( 'NONE', *, *, #38554, .T. ) ;
#42553 = ORIENTED_EDGE ( 'NONE', *, *, #17469, .F. ) ;
#42554 = AXIS2_PLACEMENT_3D ( 'NONE', #43001, #15401, #6646 ) ;
#42555 = DIRECTION ( 'NONE',  ( 1.734723475976806848E-16, -0.000000000000000000, 1.000000000000000000 ) ) ;
#42556 = FACE_BOUND ( 'NONE', #1078, .T. ) ;
#42557 = ORIENTED_EDGE ( 'NONE', *, *, #34204, .F. ) ;
#42558 = VECTOR ( 'NONE', #34187, 39.37007874015748143 ) ;
#42559 = DIRECTION ( 'NONE',  ( -0.000000000000000000, 0.000000000000000000, 1.000000000000000000 ) ) ;
#42560 = EDGE_CURVE ( 'NONE', #11282, #23897, #21276, .T. ) ;
#42561 = VECTOR ( 'NONE', #17025, 39.37007874015748143 ) ;
#42562 = EDGE_LOOP ( 'NONE', ( #9771, #48603, #41546, #9166, #3129, #6230, #45528, #16964, #20047, #41788, #27600, #14375, #33738, #35587, #12635, #3073 ) ) ;
#42563 = VERTEX_POINT ( 'NONE', #34405 ) ;
#42564 = CARTESIAN_POINT ( 'NONE',  ( -0.6233543567505162031, 1.574803149606302854, -2.073689640095379705 ) ) ;
#42565 = ADVANCED_FACE ( 'NONE', ( #11406 ), #7286, .F. ) ;
#42566 = VECTOR ( 'NONE', #12843, 39.37007874015748143 ) ;
#42567 = CARTESIAN_POINT ( 'NONE',  ( 1.015142113812069091, 3.267716535433071279, -1.732283464566923614 ) ) ;
#42568 = VERTEX_POINT ( 'NONE', #30274 ) ;
#42569 = LINE ( 'NONE', #31459, #17144 ) ;
#42570 = ORIENTED_EDGE ( 'NONE', *, *, #27196, .F. ) ;
#42571 = LINE ( 'NONE', #7964, #5411 ) ;
#42572 = CARTESIAN_POINT ( 'NONE',  ( 0.08119777152254364916, 1.623385212329073957, 0.000000000000000000 ) ) ;
#42573 = CARTESIAN_POINT ( 'NONE',  ( -0.8942052331142547050, 3.267716535433071279, 0.3149606299212580063 ) ) ;
#42574 = EDGE_LOOP ( 'NONE', ( #41795, #11075, #20158, #41972 ) ) ;
#42575 = EDGE_LOOP ( 'NONE', ( #30349, #31954, #1669, #49305 ) ) ;
#42576 = CARTESIAN_POINT ( 'NONE',  ( -1.985260859929297794, 3.267716535433071279, 0.4330708661417290162 ) ) ;
#42577 = CARTESIAN_POINT ( 'NONE',  ( -2.947574761915765063, 1.673315526576397261, -0.1816379373805333819 ) ) ;
#42578 = CARTESIAN_POINT ( 'NONE',  ( -2.946551303128973842, 1.574890269766889617, -0.1815919737934194866 ) ) ;
#42579 = ADVANCED_FACE ( 'NONE', ( #22780 ), #11152, .F. ) ;
#42580 = FACE_OUTER_BOUND ( 'NONE', #40998, .T. ) ;
#42581 = CARTESIAN_POINT ( 'NONE',  ( 0.04921259842519689481, 0.000000000000000000, 1.742692369722729895 ) ) ;
#42582 = EDGE_CURVE ( 'NONE', #31004, #2919, #38778, .T. ) ;
#42583 = DIRECTION ( 'NONE',  ( 1.734723475976806848E-16, 0.000000000000000000, 1.000000000000000000 ) ) ;
#42584 = LINE ( 'NONE', #225, #16851 ) ;
#42585 = EDGE_CURVE ( 'NONE', #4245, #29967, #46239, .T. ) ;
#42586 = EDGE_LOOP ( 'NONE', ( #27551, #5537, #10778, #31975 ) ) ;
#42587 = AXIS2_PLACEMENT_3D ( 'NONE', #41007, #26262, #22142 ) ;
#42588 = CARTESIAN_POINT ( 'NONE',  ( -2.353647019958005071, 1.172985819482486924, -0.9842519685039374799 ) ) ;
#42589 = DIRECTION ( 'NONE',  ( -0.000000000000000000, 1.000000000000000000, -0.000000000000000000 ) ) ;
#42590 = VECTOR ( 'NONE', #43450, 39.37007874015748143 ) ;
#42591 = EDGE_CURVE ( 'NONE', #17636, #33691, #19145, .T. ) ;
#42592 = EDGE_LOOP ( 'NONE', ( #42686, #43088, #38628, #9301 ) ) ;
#42593 = EDGE_LOOP ( 'NONE', ( #6126, #12026, #19708, #38499 ) ) ;
#42594 = DIRECTION ( 'NONE',  ( 1.160706738777435820E-16, 1.000000000000000000, 5.589669052740852391E-17 ) ) ;
#42595 = PLANE ( 'NONE',  #45948 ) ;
#42596 = VECTOR ( 'NONE', #37669, 39.37007874015748143 ) ;
#42597 = EDGE_LOOP ( 'NONE', ( #41837, #16355, #34210, #45959 ) ) ;
#42598 = AXIS2_PLACEMENT_3D ( 'NONE', #40915, #5540, #17164 ) ;
#42599 = EDGE_LOOP ( 'NONE', ( #45124, #34385, #25588, #3411 ) ) ;
#42600 = CARTESIAN_POINT ( 'NONE',  ( 0.1968503937007872462, 0.000000000000000000, -0.5118110236220465570 ) ) ;
#42601 = EDGE_LOOP ( 'NONE', ( #40338, #7537, #30756, #39323 ) ) ;
#42602 = DIRECTION ( 'NONE',  ( 0.2225209339563041788, -1.160734090543304660E-16, 0.9749279121818259508 ) ) ;
#42603 = DIRECTION ( 'NONE',  ( 1.000000000000000000, 0.000000000000000000, 0.000000000000000000 ) ) ;
#42604 = ORIENTED_EDGE ( 'NONE', *, *, #41961, .T. ) ;
#42605 = LINE ( 'NONE', #15498, #12330 ) ;
#42606 = VERTEX_POINT ( 'NONE', #15535 ) ;
#42607 = ORIENTED_EDGE ( 'NONE', *, *, #48182, .F. ) ;
#42608 = CARTESIAN_POINT ( 'NONE',  ( -1.363819533518803473, 0.000000000000000000, 1.732283464566920950 ) ) ;
#42609 = DIRECTION ( 'NONE',  ( 0.9998717552508121775, 0.01601477604151182663, 0.000000000000000000 ) ) ;
#42610 = CARTESIAN_POINT ( 'NONE',  ( 1.363819533518803029, 0.000000000000000000, -1.614173228346452715 ) ) ;
#42611 = ORIENTED_EDGE ( 'NONE', *, *, #3612, .F. ) ;
#42612 = FACE_OUTER_BOUND ( 'NONE', #37675, .T. ) ;
#42613 = CARTESIAN_POINT ( 'NONE',  ( 0.5455278134075211005, 0.000000000000000000, 0.1181102362204701633 ) ) ;
#42614 = CONICAL_SURFACE ( 'NONE', #29436, 1.850107469027523210, 0.6386652850508578450 ) ;
#42615 = ORIENTED_EDGE ( 'NONE', *, *, #45812, .T. ) ;
#42616 = DIRECTION ( 'NONE',  ( 0.000000000000000000, 0.000000000000000000, 1.000000000000000000 ) ) ;
#42617 = ADVANCED_FACE ( 'NONE', ( #30529 ), #10657, .F. ) ;
#42618 = VECTOR ( 'NONE', #10207, 39.37007874015748143 ) ;
#42619 = EDGE_CURVE ( 'NONE', #22241, #43639, #42384, .T. ) ;
#42620 = VERTEX_POINT ( 'NONE', #38531 ) ;
#42621 = ORIENTED_EDGE ( 'NONE', *, *, #2423, .T. ) ;
#42622 = DIRECTION ( 'NONE',  ( -0.1460985142560857764, 0.7522015574985962960, 0.6425325213783736888 ) ) ;
#42623 = ADVANCED_FACE ( 'NONE', ( #22521 ), #22276, .F. ) ;
#42624 = DIRECTION ( 'NONE',  ( -0.000000000000000000, 1.000000000000000000, -0.000000000000000000 ) ) ;
#42625 = CARTESIAN_POINT ( 'NONE',  ( -0.8182917201112819283, 0.000000000000000000, -2.244094488188968395 ) ) ;
#42626 = FACE_OUTER_BOUND ( 'NONE', #27300, .T. ) ;
#42627 = CARTESIAN_POINT ( 'NONE',  ( -2.010517631316633747, 1.205361022782829114E-17, 0.8058170502102087740 ) ) ;
#42628 = ORIENTED_EDGE ( 'NONE', *, *, #31167, .T. ) ;
#42629 = ORIENTED_EDGE ( 'NONE', *, *, #14831, .F. ) ;
#42630 = CARTESIAN_POINT ( 'NONE',  ( 2.100190309385009169, 1.205361022782829114E-17, 0.5298329251847523347 ) ) ;
#42631 = DIRECTION ( 'NONE',  ( 0.000000000000000000, 0.000000000000000000, 1.000000000000000000 ) ) ;
#42632 = VECTOR ( 'NONE', #481, 39.37007874015748143 ) ;
#42633 = ORIENTED_EDGE ( 'NONE', *, *, #21188, .T. ) ;
#42634 = DIRECTION ( 'NONE',  ( -1.000000000000000000, -0.000000000000000000, -0.000000000000000000 ) ) ;
#42635 = CARTESIAN_POINT ( 'NONE',  ( -2.867773316779185677, 1.574658946938755522, -0.7050287376752426560 ) ) ;
#42636 = EDGE_CURVE ( 'NONE', #14507, #36538, #7532, .T. ) ;
#42637 = EDGE_CURVE ( 'NONE', #47200, #706, #26889, .T. ) ;
#42638 = CARTESIAN_POINT ( 'NONE',  ( -0.2783729501556720387, 0.02346101323895649626, 1.809574371873096110 ) ) ;
#42639 = PLANE ( 'NONE',  #35143 ) ;
#42640 = CARTESIAN_POINT ( 'NONE',  ( 0.7317238754971220338, 0.1411726943947593793, 1.345337514773770948 ) ) ;
#42641 = ORIENTED_EDGE ( 'NONE', *, *, #45585, .F. ) ;
#42642 = CARTESIAN_POINT ( 'NONE',  ( 1.909347346926324684, 0.000000000000000000, -0.3543307086614178592 ) ) ;
#42643 = DIRECTION ( 'NONE',  ( 1.000000000000000000, -0.000000000000000000, 0.000000000000000000 ) ) ;
#42644 = EDGE_CURVE ( 'NONE', #23981, #17210, #42136, .T. ) ;
#42645 = CARTESIAN_POINT ( 'NONE',  ( -0.2727639067037608278, 3.346456692913386100, -1.299212598425193210 ) ) ;
#42646 = VERTEX_POINT ( 'NONE', #15279 ) ;
#42647 = DIRECTION ( 'NONE',  ( -3.986037398843765983E-20, -1.000000000000000000, -1.160734090543304660E-16 ) ) ;
#42648 = CARTESIAN_POINT ( 'NONE',  ( 0.5762653268100312864, 0.000000000000000000, -1.903066372058335620 ) ) ;
#42649 = VECTOR ( 'NONE', #29991, 39.37007874015748143 ) ;
#42650 = ORIENTED_EDGE ( 'NONE', *, *, #31422, .F. ) ;
#42651 = VECTOR ( 'NONE', #2349, 39.37007874015748143 ) ;
#42652 = CARTESIAN_POINT ( 'NONE',  ( 0.4696143004045481018, 3.267716535433071279, -1.629301903132388246E-16 ) ) ;
#42653 = AXIS2_PLACEMENT_3D ( 'NONE', #18719, #50157, #30337 ) ;
#42654 = ORIENTED_EDGE ( 'NONE', *, *, #5815, .F. ) ;
#42655 = CARTESIAN_POINT ( 'NONE',  ( 1.363819533518803251, 3.346456692913386100, -0.3543307086614178592 ) ) ;
#42656 = ORIENTED_EDGE ( 'NONE', *, *, #43321, .F. ) ;
#42657 = LINE ( 'NONE', #11927, #34456 ) ;
#42658 = EDGE_CURVE ( 'NONE', #44522, #14656, #15514, .T. ) ;
#42659 = ORIENTED_EDGE ( 'NONE', *, *, #37764, .T. ) ;
#42660 = DIRECTION ( 'NONE',  ( -0.000000000000000000, 1.000000000000000000, -0.000000000000000000 ) ) ;
#42661 = DIRECTION ( 'NONE',  ( -1.000000000000000000, 0.000000000000000000, 1.734723475976806848E-16 ) ) ;
#42662 = CARTESIAN_POINT ( 'NONE',  ( 2.158170387640339527, -2.691217175373896062E-17, 0.2426819907294796574 ) ) ;
#42663 = VERTEX_POINT ( 'NONE', #31029 ) ;
#42664 = ORIENTED_EDGE ( 'NONE', *, *, #28535, .F. ) ;
#42665 = EDGE_LOOP ( 'NONE', ( #41951, #18147, #48189, #1479 ) ) ;
#42666 = CARTESIAN_POINT ( 'NONE',  ( 0.000000000000000000, 3.267716535433071279, 0.000000000000000000 ) ) ;
#42667 = CARTESIAN_POINT ( 'NONE',  ( 1.091055626815042645, 0.000000000000000000, 0.4330708661417287386 ) ) ;
#42668 = ORIENTED_EDGE ( 'NONE', *, *, #5843, .F. ) ;
#42669 = ORIENTED_EDGE ( 'NONE', *, *, #10105, .F. ) ;
#42670 = DIRECTION ( 'NONE',  ( 1.000000000000000000, 0.000000000000000000, 0.000000000000000000 ) ) ;
#42671 = FACE_OUTER_BOUND ( 'NONE', #25294, .T. ) ;
#42672 = PLANE ( 'NONE',  #2227 ) ;
#42673 = VECTOR ( 'NONE', #16687, 39.37007874015748143 ) ;
#42674 = ORIENTED_EDGE ( 'NONE', *, *, #33205, .F. ) ;
#42675 = EDGE_LOOP ( 'NONE', ( #32986, #17236, #2861, #24381, #22301, #1356, #10010, #35670, #46668, #28135, #34917, #24961, #41802, #7178, #12768, #10529, #21186, #39576, #39713, #16982, #16432, #46398, #33292, #48305, #42437, #28789, #30980, #43342, #40416, #45276, #12840, #38182, #7450, #30802, #119, #36671, #43679, #3187, #18635, #6334, #21879, #21993, #23789, #8527, #40801, #1978, #24733, #14992, #19820, #25075, #41583, #48917, #33573, #18444, #910, #14301, #13611, #36911, #13767, #14396, #37250, #47388, #28065, #49617, #27821, #14213, #31939, #46489, #48536, #22992, #29612, #50812, #24343, #47771, #35187, #44138, #17670, #50170, #8692, #32790, #34357, #23526, #24304, #408, #15492, #29940, #38700 ) ) ;
#42676 = DIRECTION ( 'NONE',  ( -1.000000000000000000, -0.000000000000000000, -0.000000000000000000 ) ) ;
#42677 = CARTESIAN_POINT ( 'NONE',  ( 0.1968503937007873017, 3.346456692913386100, -1.259842519685035134 ) ) ;
#42678 = CARTESIAN_POINT ( 'NONE',  ( 1.636583440222563857, 0.000000000000000000, 0.4330708661417290162 ) ) ;
#42679 = ORIENTED_EDGE ( 'NONE', *, *, #8178, .T. ) ;
#42680 = FACE_OUTER_BOUND ( 'NONE', #6439, .T. ) ;
#42681 = DIRECTION ( 'NONE',  ( -0.000000000000000000, 0.000000000000000000, 1.000000000000000000 ) ) ;
#42682 = ORIENTED_EDGE ( 'NONE', *, *, #12605, .T. ) ;
#42683 = EDGE_CURVE ( 'NONE', #20401, #19154, #50906, .T. ) ;
#42684 = LINE ( 'NONE', #42435, #19190 ) ;
#42685 = ORIENTED_EDGE ( 'NONE', *, *, #30041, .F. ) ;
#42686 = ORIENTED_EDGE ( 'NONE', *, *, #36049, .T. ) ;
#42687 = FACE_OUTER_BOUND ( 'NONE', #24613, .T. ) ;
#42688 = CARTESIAN_POINT ( 'NONE',  ( 1.091055626815042645, 0.000000000000000000, 0.3149606299212578953 ) ) ;
#42689 = EDGE_CURVE ( 'NONE', #50201, #2264, #47247, .T. ) ;
#42690 = DIRECTION ( 'NONE',  ( 0.9998717552508121775, 0.01601477604151182663, 0.000000000000000000 ) ) ;
#42691 = ADVANCED_FACE ( 'NONE', ( #19387 ), #2902, .F. ) ;
#42692 = VECTOR ( 'NONE', #32656, 39.37007874015748143 ) ;
#42693 = CIRCLE ( 'NONE', #22908, 2.106299212598425008 ) ;
#42694 = DIRECTION ( 'NONE',  ( -0.9998717552508122886, -0.01601477604151182316, 0.000000000000000000 ) ) ;
#42695 = ADVANCED_FACE ( 'NONE', ( #19893 ), #35413, .F. ) ;
#42696 = DIRECTION ( 'NONE',  ( -3.469446951953613696E-16, 0.000000000000000000, -1.000000000000000000 ) ) ;
#42697 = ORIENTED_EDGE ( 'NONE', *, *, #35685, .F. ) ;
#42698 = VECTOR ( 'NONE', #40020, 39.37007874015748143 ) ;
#42699 = VERTEX_POINT ( 'NONE', #25004 ) ;
#42700 = LINE ( 'NONE', #7349, #3019 ) ;
#42701 = CARTESIAN_POINT ( 'NONE',  ( -1.909347346926324462, 3.267716535433071279, 1.021348170950612255 ) ) ;
#42702 = EDGE_CURVE ( 'NONE', #3958, #11368, #7784, .T. ) ;
#42703 = AXIS2_PLACEMENT_3D ( 'NONE', #18825, #22950, #46661 ) ;
#42704 = DIRECTION ( 'NONE',  ( 1.734723475976806848E-16, 0.000000000000000000, 1.000000000000000000 ) ) ;
#42705 = CARTESIAN_POINT ( 'NONE',  ( 1.091055626815042645, 3.346456692913386100, 1.259842519685033357 ) ) ;
#42706 = ORIENTED_EDGE ( 'NONE', *, *, #34378, .F. ) ;
#42707 = CARTESIAN_POINT ( 'NONE',  ( 0.4696143004045479907, 3.267716535433071279, -1.629301903132387999E-16 ) ) ;
#42708 = EDGE_CURVE ( 'NONE', #24890, #45264, #15776, .T. ) ;
#42709 = VECTOR ( 'NONE', #8103, 39.37007874015748143 ) ;
#42710 = DIRECTION ( 'NONE',  ( 1.000000000000000000, -0.000000000000000000, 0.000000000000000000 ) ) ;
#42711 = ORIENTED_EDGE ( 'NONE', *, *, #27233, .F. ) ;
#42712 = CARTESIAN_POINT ( 'NONE',  ( -0.5455278134075212115, 3.267716535433071279, 9.463399047163220715E-17 ) ) ;
#42713 = CARTESIAN_POINT ( 'NONE',  ( 1.561199273709754642, 0.01720004865961270724, 1.307960151495090262 ) ) ;
#42714 = FACE_OUTER_BOUND ( 'NONE', #4442, .T. ) ;
#42715 = EDGE_CURVE ( 'NONE', #10781, #11701, #12882, .T. ) ;
#42716 = DIRECTION ( 'NONE',  ( -3.469446951953613696E-16, 0.000000000000000000, -1.000000000000000000 ) ) ;
#42717 = DIRECTION ( 'NONE',  ( -3.469446951953613696E-16, 0.000000000000000000, -1.000000000000000000 ) ) ;
#42718 = LINE ( 'NONE', #23346, #30983 ) ;
#42719 = ORIENTED_EDGE ( 'NONE', *, *, #36660, .T. ) ;
#42720 = LINE ( 'NONE', #7612, #10654 ) ;
#42721 = EDGE_LOOP ( 'NONE', ( #30075, #35807, #4769, #27628, #8922, #43759 ) ) ;
#42722 = CARTESIAN_POINT ( 'NONE',  ( -0.4460728916448887249, 1.700757277111965449, 2.182451250484750638 ) ) ;
#42723 = EDGE_CURVE ( 'NONE', #23450, #41713, #17267, .T. ) ;
#42724 = CARTESIAN_POINT ( 'NONE',  ( 1.636583440222563857, 0.000000000000000000, 0.6299212598425164567 ) ) ;
#42725 = DIRECTION ( 'NONE',  ( 1.000000000000000000, 0.000000000000000000, 0.000000000000000000 ) ) ;
#42726 = VECTOR ( 'NONE', #20319, 39.37007874015748143 ) ;
#42727 = ORIENTED_EDGE ( 'NONE', *, *, #50514, .F. ) ;
#42728 = VERTEX_POINT ( 'NONE', #1255 ) ;
#42729 = PLANE ( 'NONE',  #5083 ) ;
#42730 = PLANE ( 'NONE',  #32881 ) ;
#42731 = EDGE_CURVE ( 'NONE', #44818, #42300, #20792, .T. ) ;
#42732 = DIRECTION ( 'NONE',  ( 1.000000000000000000, 0.000000000000000000, 0.000000000000000000 ) ) ;
#42733 = VECTOR ( 'NONE', #31333, 39.37007874015748143 ) ;
#42734 = DIRECTION ( 'NONE',  ( 1.000000000000000000, 0.000000000000000000, -3.469446951953613696E-16 ) ) ;
#42735 = FACE_OUTER_BOUND ( 'NONE', #4430, .T. ) ;
#42736 = LINE ( 'NONE', #47334, #16553 ) ;
#42737 = VECTOR ( 'NONE', #35763, 39.37007874015748143 ) ;
#42738 = CIRCLE ( 'NONE', #46797, 2.165354330708661568 ) ;
#42739 = ORIENTED_EDGE ( 'NONE', *, *, #25331, .F. ) ;
#42740 = VERTEX_POINT ( 'NONE', #24753 ) ;
#42741 = CARTESIAN_POINT ( 'NONE',  ( 1.556712866041120247, 1.743522182421873401, 2.509548638715870084 ) ) ;
#42742 = VECTOR ( 'NONE', #6390, 39.37007874015748143 ) ;
#42743 = CARTESIAN_POINT ( 'NONE',  ( 0.000000000000000000, 3.267716535433071279, 1.220472440944875281 ) ) ;
#42744 = VERTEX_POINT ( 'NONE', #44359 ) ;
#42745 = DIRECTION ( 'NONE',  ( 1.734723475976806848E-16, -0.000000000000000000, 1.000000000000000000 ) ) ;
#42746 = ORIENTED_EDGE ( 'NONE', *, *, #13803, .T. ) ;
#42747 = EDGE_LOOP ( 'NONE', ( #34172, #46345, #11587, #40476 ) ) ;
#42748 = AXIS2_PLACEMENT_3D ( 'NONE', #39928, #12559, #32972 ) ;
#42749 = ADVANCED_FACE ( 'NONE', ( #13646 ), #33024, .F. ) ;
#42750 = AXIS2_PLACEMENT_3D ( 'NONE', #23453, #19829, #218 ) ;
#42751 = EDGE_LOOP ( 'NONE', ( #44337, #27566, #46330, #48037 ) ) ;
#42752 = ORIENTED_EDGE ( 'NONE', *, *, #36156, .T. ) ;
#42753 = DIRECTION ( 'NONE',  ( -1.000000000000000000, -0.000000000000000000, -0.000000000000000000 ) ) ;
#42754 = EDGE_CURVE ( 'NONE', #41115, #47582, #49724, .T. ) ;
#42755 = CARTESIAN_POINT ( 'NONE',  ( 2.565025421079572876, 0.9854942283129086711, -0.5349721219160458174 ) ) ;
#42756 = LINE ( 'NONE', #22641, #48302 ) ;
#42757 = CARTESIAN_POINT ( 'NONE',  ( 0.5756566573088583993, 1.728235332270611879, 2.896516654582643291 ) ) ;
#42758 = VECTOR ( 'NONE', #1979, 39.37007874015748143 ) ;
#42759 = DIRECTION ( 'NONE',  ( 1.000000000000000000, -0.000000000000000000, 0.000000000000000000 ) ) ;
#42760 = CARTESIAN_POINT ( 'NONE',  ( -1.636583440222564301, 0.000000000000000000, -1.456692913385822186 ) ) ;
#42761 = DIRECTION ( 'NONE',  ( -0.000000000000000000, 1.000000000000000000, -0.000000000000000000 ) ) ;
#42762 = EDGE_LOOP ( 'NONE', ( #32252, #878, #28896, #42668 ) ) ;
#42763 = CARTESIAN_POINT ( 'NONE',  ( 0.4696143004045484903, 3.346456692913386100, 1.102362204724404160 ) ) ;
#42764 = FACE_OUTER_BOUND ( 'NONE', #8093, .T. ) ;
#42765 = CARTESIAN_POINT ( 'NONE',  ( -1.166969139818016199, 3.346456692913386100, -0.6692913385826760875 ) ) ;
#42766 = PLANE ( 'NONE',  #47077 ) ;
#42767 = VECTOR ( 'NONE', #40347, 39.37007874015748143 ) ;
#42768 = AXIS2_PLACEMENT_3D ( 'NONE', #42286, #37681, #29668 ) ;
#42769 = ORIENTED_EDGE ( 'NONE', *, *, #8184, .F. ) ;
#42770 = CARTESIAN_POINT ( 'NONE',  ( -0.2042174104418111591, 2.755905511811024056, -0.3133417129078099328 ) ) ;
#42771 = CARTESIAN_POINT ( 'NONE',  ( -2.491402175429631605, 1.205361022782829114E-17, -1.585592796919542025 ) ) ;
#42772 = ORIENTED_EDGE ( 'NONE', *, *, #30788, .F. ) ;
#42773 = DIRECTION ( 'NONE',  ( -3.469446951953613696E-16, 0.000000000000000000, -1.000000000000000000 ) ) ;
#42774 = EDGE_CURVE ( 'NONE', #37198, #47182, #9515, .T. ) ;
#42775 = CARTESIAN_POINT ( 'NONE',  ( 0.000000000000000000, 2.755905511811023612, 0.000000000000000000 ) ) ;
#42776 =( GEOMETRIC_REPRESENTATION_CONTEXT ( 3 ) GLOBAL_UNCERTAINTY_ASSIGNED_CONTEXT ( ( #10198 ) ) GLOBAL_UNIT_ASSIGNED_CONTEXT ( ( #43383, #275, #15523 ) ) REPRESENTATION_CONTEXT ( 'NONE', 'WORKASPACE' ) );
#42777 = DIRECTION ( 'NONE',  ( 1.000000000000000000, 0.000000000000000000, 0.000000000000000000 ) ) ;
#42778 = ORIENTED_EDGE ( 'NONE', *, *, #30176, .F. ) ;
#42779 = DIRECTION ( 'NONE',  ( -1.495358972789985422E-32, 1.160734090543304660E-16, -1.000000000000000000 ) ) ;
#42780 = ADVANCED_FACE ( 'NONE', ( #23784 ), #31186, .T. ) ;
#42781 = CARTESIAN_POINT ( 'NONE',  ( -1.439733046521777027, 0.000000000000000000, -1.141732283464563791 ) ) ;
#42782 = EDGE_CURVE ( 'NONE', #15190, #24926, #17190, .T. ) ;
#42783 = CARTESIAN_POINT ( 'NONE',  ( 0.1968503937007878568, 0.000000000000000000, 1.889763779527550369 ) ) ;
#42784 = CARTESIAN_POINT ( 'NONE',  ( -1.166969139818015533, 0.000000000000000000, 0.7874015748031456541 ) ) ;
#42785 = ORIENTED_EDGE ( 'NONE', *, *, #8985, .T. ) ;
#42786 = EDGE_CURVE ( 'NONE', #21618, #50651, #36948, .T. ) ;
#42787 = ORIENTED_EDGE ( 'NONE', *, *, #29666, .T. ) ;
#42788 = EDGE_LOOP ( 'NONE', ( #46392, #27392, #38590, #6036 ) ) ;
#42789 = CARTESIAN_POINT ( 'NONE',  ( 0.2727639067037610499, 3.346456692913386100, 2.047244094488179567 ) ) ;
#42790 = ORIENTED_EDGE ( 'NONE', *, *, #24784, .F. ) ;
#42791 = EDGE_CURVE ( 'NONE', #9101, #48909, #35663, .T. ) ;
#42792 = CARTESIAN_POINT ( 'NONE',  ( -1.636583440222564301, 3.346456692913386100, -1.771653543307080581 ) ) ;
#42793 = CARTESIAN_POINT ( 'NONE',  ( -0.6214413264104939882, 3.267716535433071279, 0.2755905511810998187 ) ) ;
#42794 = VERTEX_POINT ( 'NONE', #21393 ) ;
#42795 = EDGE_CURVE ( 'NONE', #11317, #5956, #48707, .T. ) ;
#42796 = DIRECTION ( 'NONE',  ( -2.891205793294678326E-16, 0.000000000000000000, 1.000000000000000000 ) ) ;
#42797 = VECTOR ( 'NONE', #7314, 39.37007874015748143 ) ;
#42798 = ORIENTED_EDGE ( 'NONE', *, *, #28064, .F. ) ;
#42799 = CARTESIAN_POINT ( 'NONE',  ( 0.8182917201112819283, 3.267716535433071279, -1.419509857074483292E-16 ) ) ;
#42800 = EDGE_LOOP ( 'NONE', ( #47258, #12308, #11217, #5192 ) ) ;
#42801 = VERTEX_POINT ( 'NONE', #13388 ) ;
#42802 = CARTESIAN_POINT ( 'NONE',  ( -1.363819533518803473, 3.346456692913386100, -1.417322834645664109 ) ) ;
#42803 = VERTEX_POINT ( 'NONE', #48451 ) ;
#42804 = EDGE_CURVE ( 'NONE', #41352, #17988, #13138, .T. ) ;
#42805 = AXIS2_PLACEMENT_3D ( 'NONE', #19446, #31086, #7587 ) ;
#42806 = CARTESIAN_POINT ( 'NONE',  ( 0.000000000000000000, 3.267716535433071279, -1.574803149606293529 ) ) ;
#42807 = ORIENTED_EDGE ( 'NONE', *, *, #49236, .F. ) ;
#42808 = ORIENTED_EDGE ( 'NONE', *, *, #40942, .T. ) ;
#42809 = EDGE_CURVE ( 'NONE', #11414, #24015, #17515, .T. ) ;
#42810 = VECTOR ( 'NONE', #40893, 39.37007874015748143 ) ;
#42811 = CARTESIAN_POINT ( 'NONE',  ( 1.015142113812069313, 0.000000000000000000, 0.1574803149606286423 ) ) ;
#42812 = CARTESIAN_POINT ( 'NONE',  ( -2.443991082961025185, 3.256070107886888110, -0.1574803149606298636 ) ) ;
#42813 = ORIENTED_EDGE ( 'NONE', *, *, #7491, .F. ) ;
#42814 = LINE ( 'NONE', #35586, #11381 ) ;
#42815 = ORIENTED_EDGE ( 'NONE', *, *, #28012, .F. ) ;
#42816 = CARTESIAN_POINT ( 'NONE',  ( 2.122891901563675354, 1.466501505047771436, -2.052405154120522379 ) ) ;
#42817 = CARTESIAN_POINT ( 'NONE',  ( 0.000000000000000000, 3.346456692913386100, 0.000000000000000000 ) ) ;
#42818 = CARTESIAN_POINT ( 'NONE',  ( 1.636583440222563635, 0.000000000000000000, -1.259842519685035800 ) ) ;
#42819 = ORIENTED_EDGE ( 'NONE', *, *, #8616, .F. ) ;
#42820 = VERTEX_POINT ( 'NONE', #18274 ) ;
#42821 = CARTESIAN_POINT ( 'NONE',  ( 0.5756566573088583993, 1.502670515430445386, 2.896516654582643291 ) ) ;
#42822 = LINE ( 'NONE', #46920, #12988 ) ;
#42823 = DIRECTION ( 'NONE',  ( -3.986037398843765983E-20, -1.000000000000000000, -1.160734090543304660E-16 ) ) ;
#42824 = CARTESIAN_POINT ( 'NONE',  ( -2.735162923786631950, 2.755905511811027164, -0.4201650439732181885 ) ) ;
#42825 = DIRECTION ( 'NONE',  ( -0.000000000000000000, 1.000000000000000000, -0.000000000000000000 ) ) ;
#42826 = DIRECTION ( 'NONE',  ( -0.000000000000000000, 1.000000000000000000, -0.000000000000000000 ) ) ;
#42827 = AXIS2_PLACEMENT_3D ( 'NONE', #4267, #12275, #12016 ) ;
#42828 = CARTESIAN_POINT ( 'NONE',  ( 2.106197740627111958, 0.000000000000000000, 0.5905511811023582691 ) ) ;
#42829 = ORIENTED_EDGE ( 'NONE', *, *, #37151, .T. ) ;
#42830 = DIRECTION ( 'NONE',  ( -1.000000000000000000, 0.000000000000000000, 0.000000000000000000 ) ) ;
#42831 = ORIENTED_EDGE ( 'NONE', *, *, #5987, .F. ) ;
#42832 = VERTEX_POINT ( 'NONE', #10530 ) ;
#42833 = CARTESIAN_POINT ( 'NONE',  ( -2.952069331832154919, 2.755905511811027164, -1.181102362204724088 ) ) ;
#42834 = VECTOR ( 'NONE', #45157, 39.37007874015748143 ) ;
#42835 = FACE_OUTER_BOUND ( 'NONE', #8011, .T. ) ;
#42836 = EDGE_CURVE ( 'NONE', #22772, #21459, #33787, .T. ) ;
#42837 = VERTEX_POINT ( 'NONE', #2275 ) ;
#42838 = EDGE_CURVE ( 'NONE', #9111, #9804, #6908, .T. ) ;
#42839 = EDGE_CURVE ( 'NONE', #27124, #15499, #30408, .T. ) ;
#42840 = CARTESIAN_POINT ( 'NONE',  ( 0.4696143004045476577, 0.000000000000000000, -2.047244094488182231 ) ) ;
#42841 = ORIENTED_EDGE ( 'NONE', *, *, #6165, .F. ) ;
#42842 = DIRECTION ( 'NONE',  ( 1.000000000000000000, 0.000000000000000000, 0.000000000000000000 ) ) ;
#42843 = AXIS2_PLACEMENT_3D ( 'NONE', #25590, #12699, #29203 ) ;
#42844 = VERTEX_POINT ( 'NONE', #29647 ) ;
#42845 = FACE_OUTER_BOUND ( 'NONE', #1720, .T. ) ;
#42846 = CARTESIAN_POINT ( 'NONE',  ( 1.091055626815042645, 3.346456692913386100, 0.4330708661417287386 ) ) ;
#42847 = VERTEX_POINT ( 'NONE', #38165 ) ;
#42848 = DIRECTION ( 'NONE',  ( 1.000000000000000000, 0.000000000000000000, 0.000000000000000000 ) ) ;
#42849 = EDGE_LOOP ( 'NONE', ( #9839, #23029, #24107, #7577 ) ) ;
#42850 = EDGE_LOOP ( 'NONE', ( #3422, #37027, #31390, #43561 ) ) ;
#42851 = CARTESIAN_POINT ( 'NONE',  ( -1.166969139818015533, 0.000000000000000000, 1.102362204724404160 ) ) ;
#42852 = CARTESIAN_POINT ( 'NONE',  ( 0.5455278134075212115, 0.000000000000000000, 0.9448818897637746295 ) ) ;
#42853 = CARTESIAN_POINT ( 'NONE',  ( 0.000000000000000000, 6.692913385826772199, 0.000000000000000000 ) ) ;
#42854 = B_SPLINE_CURVE_WITH_KNOTS ( 'NONE', 3,
 ( #18501, #45330, #17991, #33758 ),
 .UNSPECIFIED., .F., .F.,
 ( 4, 4 ),
 ( 2.396528199383891172E-07, 0.002500331713901011391 ),
 .UNSPECIFIED. ) ;
#42855 = ADVANCED_FACE ( 'NONE', ( #49467 ), #25511, .F. ) ;
#42856 = ORIENTED_EDGE ( 'NONE', *, *, #26136, .F. ) ;
#42857 = EDGE_CURVE ( 'NONE', #11491, #40469, #30150, .T. ) ;
#42858 = CARTESIAN_POINT ( 'NONE',  ( 0.1968503937007878568, 0.000000000000000000, 2.204724409448808764 ) ) ;
#42859 = DIRECTION ( 'NONE',  ( 1.734723475976806848E-16, -0.000000000000000000, 1.000000000000000000 ) ) ;
#42860 = VERTEX_POINT ( 'NONE', #2531 ) ;
#42861 = EDGE_CURVE ( 'NONE', #28846, #38729, #41772, .T. ) ;
#42862 = CARTESIAN_POINT ( 'NONE',  ( -1.439733046521777027, 3.267716535433071279, -1.456692913385822186 ) ) ;
#42863 = EDGE_CURVE ( 'NONE', #42295, #162, #45995, .T. ) ;
#42864 = EDGE_LOOP ( 'NONE', ( #43657, #37742, #8717, #30903 ) ) ;
#42865 = EDGE_LOOP ( 'NONE', ( #3028, #33803, #8023, #27855 ) ) ;
#42866 = DIRECTION ( 'NONE',  ( 1.000000000000000000, 0.000000000000000000, 0.000000000000000000 ) ) ;
#42867 = VERTEX_POINT ( 'NONE', #17769 ) ;
#42868 = CARTESIAN_POINT ( 'NONE',  ( 0.000000000000000000, 0.000000000000000000, 0.000000000000000000 ) ) ;
#42869 = VECTOR ( 'NONE', #17499, 39.37007874015748143 ) ;
#42870 = CARTESIAN_POINT ( 'NONE',  ( 0.000000000000000000, 5.905511811023623991, 0.000000000000000000 ) ) ;
#42871 = CIRCLE ( 'NONE', #15686, 2.165354330708661568 ) ;
#42872 = LINE ( 'NONE', #39773, #10475 ) ;
#42873 = CARTESIAN_POINT ( 'NONE',  ( 0.8182917201112817063, 0.000000000000000000, -1.614173228346451605 ) ) ;
#42874 = EDGE_LOOP ( 'NONE', ( #39815, #4216, #28980, #26357, #24352 ) ) ;
#42875 = ORIENTED_EDGE ( 'NONE', *, *, #45524, .F. ) ;
#42876 = CARTESIAN_POINT ( 'NONE',  ( 3.616083068348484413E-16, 3.346456692913386100, 2.952755905511811552 ) ) ;
#42877 = CARTESIAN_POINT ( 'NONE',  ( -1.091055626815042645, 3.267716535433071279, -0.8267716535433052849 ) ) ;
#42878 = VECTOR ( 'NONE', #36654, 39.37007874015748143 ) ;
#42879 = ORIENTED_EDGE ( 'NONE', *, *, #27428, .T. ) ;
#42880 = DIRECTION ( 'NONE',  ( 1.000000000000000000, 0.000000000000000000, -3.469446951953613696E-16 ) ) ;
#42881 = CARTESIAN_POINT ( 'NONE',  ( 2.042485253772177156, 1.205361022782829114E-17, 0.6118985000151695441 ) ) ;
#42882 = CARTESIAN_POINT ( 'NONE',  ( -0.2727639067037607723, 3.346456692913386100, 0.1574803149606283648 ) ) ;
#42883 = LINE ( 'NONE', #23270, #47443 ) ;
#42884 = CARTESIAN_POINT ( 'NONE',  ( 3.927031490892378253E-16, 0.000000000000000000, 1.377952755905504256 ) ) ;
#42885 = ORIENTED_EDGE ( 'NONE', *, *, #48210, .F. ) ;
#42886 = PLANE ( 'NONE',  #41505 ) ;
#42887 = CARTESIAN_POINT ( 'NONE',  ( -0.04921259842519689481, 2.794703227806734062E-17, 1.924024829198930364 ) ) ;
#42888 = B_SPLINE_CURVE_WITH_KNOTS ( 'NONE', 3,
 ( #30095, #34230, #25707, #5835 ),
 .UNSPECIFIED., .F., .F.,
 ( 4, 4 ),
 ( 0.001714960275793771249, 0.003045713467573901712 ),
 .UNSPECIFIED. ) ;
#42889 = ORIENTED_EDGE ( 'NONE', *, *, #20394, .T. ) ;
#42890 = FACE_OUTER_BOUND ( 'NONE', #21815, .T. ) ;
#42891 = CARTESIAN_POINT ( 'NONE',  ( -0.2727639067037607723, 3.346456692913386100, -1.732283464566922726 ) ) ;
#42892 = DIRECTION ( 'NONE',  ( -0.9998717552508122886, -0.01601477604151182316, 0.000000000000000000 ) ) ;
#42893 = ORIENTED_EDGE ( 'NONE', *, *, #38236, .T. ) ;
#42894 = EDGE_CURVE ( 'NONE', #24866, #30287, #34035, .T. ) ;
#42895 = ADVANCED_FACE ( 'NONE', ( #34286 ), #6148, .F. ) ;
#42896 = ORIENTED_EDGE ( 'NONE', *, *, #40130, .F. ) ;
#42897 = CARTESIAN_POINT ( 'NONE',  ( 0.2727639067037607168, 3.267716535433071279, -4.731699523581612206E-17 ) ) ;
#42898 = VERTEX_POINT ( 'NONE', #22158 ) ;
#42899 = CARTESIAN_POINT ( 'NONE',  ( 0.2727639067037609943, 3.346456692913386100, 1.850393700787392293 ) ) ;
#42900 = EDGE_CURVE ( 'NONE', #49899, #42214, #49975, .T. ) ;
#42901 = EDGE_LOOP ( 'NONE', ( #4414, #48485, #41351, #43913 ) ) ;
#42902 = VECTOR ( 'NONE', #4928, 39.37007874015748143 ) ;
#42903 = DIRECTION ( 'NONE',  ( 1.000000000000000000, 0.000000000000000000, 0.000000000000000000 ) ) ;
#42904 = CARTESIAN_POINT ( 'NONE',  ( 1.466506618346834934, 1.205361022782829114E-17, -1.470210429041567401 ) ) ;
#42905 = DIRECTION ( 'NONE',  ( -1.000000000000000000, 0.000000000000000000, -0.000000000000000000 ) ) ;
#42906 = AXIS2_PLACEMENT_3D ( 'NONE', #9265, #25010, #5134 ) ;
#42907 = VERTEX_POINT ( 'NONE', #26022 ) ;
#42908 = ORIENTED_EDGE ( 'NONE', *, *, #23870, .F. ) ;
#42909 = EDGE_LOOP ( 'NONE', ( #32652, #8746, #31384, #24814 ) ) ;
#42910 = DIRECTION ( 'NONE',  ( -0.000000000000000000, 1.000000000000000000, -0.000000000000000000 ) ) ;
#42911 = CARTESIAN_POINT ( 'NONE',  ( -1.344120862506149594, 3.256110399587370807, 2.047244094488179567 ) ) ;
#42912 = ORIENTED_EDGE ( 'NONE', *, *, #16036, .T. ) ;
#42913 = ORIENTED_EDGE ( 'NONE', *, *, #20932, .F. ) ;
#42914 = CARTESIAN_POINT ( 'NONE',  ( 0.4001787029124908024, 1.205361022782829114E-17, 1.929553426015793605 ) ) ;
#42915 = CARTESIAN_POINT ( 'NONE',  ( 2.932638728931774352, 5.118110236220475784, 0.3475908556738230293 ) ) ;
#42916 = AXIS2_PLACEMENT_3D ( 'NONE', #27493, #15125, #30877 ) ;
#42917 = CARTESIAN_POINT ( 'NONE',  ( -1.091055626815042645, 3.267716535433071279, -0.5118110236220467790 ) ) ;
#42918 = ORIENTED_EDGE ( 'NONE', *, *, #34956, .F. ) ;
#42919 = EDGE_LOOP ( 'NONE', ( #38875, #28700, #26873, #46369 ) ) ;
#42920 = EDGE_CURVE ( 'NONE', #20320, #17100, #10024, .T. ) ;
#42921 = DIRECTION ( 'NONE',  ( 0.000000000000000000, 1.000000000000000000, 0.000000000000000000 ) ) ;
#42922 = CARTESIAN_POINT ( 'NONE',  ( -1.363819533518803029, 0.000000000000000000, 0.1574803149606287811 ) ) ;
#42923 = DIRECTION ( 'NONE',  ( 1.734723475976806848E-16, -0.000000000000000000, 1.000000000000000000 ) ) ;
#42924 = ORIENTED_EDGE ( 'NONE', *, *, #43317, .F. ) ;
#42925 = DIRECTION ( 'NONE',  ( 3.324886662288880100E-16, -5.168407336632174847E-17, -1.000000000000000000 ) ) ;
#42926 = PLANE ( 'NONE',  #45824 ) ;
#42927 = ORIENTED_EDGE ( 'NONE', *, *, #8498, .F. ) ;
#42928 = EDGE_CURVE ( 'NONE', #19691, #1644, #18841, .T. ) ;
#42929 = CARTESIAN_POINT ( 'NONE',  ( -1.088097428176262760, 1.690474079180120492, 1.917118167796188821 ) ) ;
#42930 = ORIENTED_EDGE ( 'NONE', *, *, #6634, .T. ) ;
#42931 = ORIENTED_EDGE ( 'NONE', *, *, #36585, .F. ) ;
#42932 = DIRECTION ( 'NONE',  ( -3.469446951953613696E-16, 0.000000000000000000, -1.000000000000000000 ) ) ;
#42933 = FACE_OUTER_BOUND ( 'NONE', #19609, .T. ) ;
#42934 = CYLINDRICAL_SURFACE ( 'NONE', #7440, 2.165354330708661568 ) ;
#42935 = CARTESIAN_POINT ( 'NONE',  ( -2.454875160333845674, 3.232777166330581320, 0.1574803149606286423 ) ) ;
#42936 = PLANE ( 'NONE',  #16437 ) ;
#42937 = ORIENTED_EDGE ( 'NONE', *, *, #13743, .F. ) ;
#42938 = ORIENTED_EDGE ( 'NONE', *, *, #49675, .T. ) ;
#42939 = PRODUCT_DEFINITION_SHAPE ( 'NONE', 'NONE',  #23739 ) ;
#42940 = VERTEX_POINT ( 'NONE', #49219 ) ;
#42941 = CARTESIAN_POINT ( 'NONE',  ( -1.363819533518803473, 3.346456692913386100, -1.102362204724405270 ) ) ;
#42942 = DIRECTION ( 'NONE',  ( -0.000000000000000000, -1.000000000000000000, 0.000000000000000000 ) ) ;
#42943 = VECTOR ( 'NONE', #39728, 39.37007874015748143 ) ;
#42944 = VECTOR ( 'NONE', #49438, 39.37007874015748143 ) ;
#42945 = CARTESIAN_POINT ( 'NONE',  ( 1.636583440222563635, 3.267716535433071279, -1.456692913385823296 ) ) ;
#42946 = CARTESIAN_POINT ( 'NONE',  ( 0.9243200180699869817, 1.726337457326624580, 2.322784611151789136 ) ) ;
#42947 = ORIENTED_EDGE ( 'NONE', *, *, #35278, .T. ) ;
#42948 = CARTESIAN_POINT ( 'NONE',  ( 0.000000000000000000, 3.267716535433071279, 0.000000000000000000 ) ) ;
#42949 = AXIS2_PLACEMENT_3D ( 'NONE', #33565, #25034, #45140 ) ;
#42950 = DIRECTION ( 'NONE',  ( 0.9909497617679331460, 0.000000000000000000, 0.1342332658176667026 ) ) ;
#42951 = EDGE_LOOP ( 'NONE', ( #11174, #41126, #29421 ) ) ;
#42952 = VECTOR ( 'NONE', #6083, 39.37007874015748143 ) ;
#42953 = LINE ( 'NONE', #44736, #24060 ) ;
#42954 = DIRECTION ( 'NONE',  ( 0.000000000000000000, 1.000000000000000000, -0.000000000000000000 ) ) ;
#42955 = LINE ( 'NONE', #23343, #39505 ) ;
#42956 = CARTESIAN_POINT ( 'NONE',  ( 1.091055626815042423, 3.267716535433071279, -1.259842519685035134 ) ) ;
#42957 = LINE ( 'NONE', #15610, #49813 ) ;
#42958 = LINE ( 'NONE', #3227, #16133 ) ;
#42959 = EDGE_CURVE ( 'NONE', #46022, #23992, #46124, .T. ) ;
#42960 = EDGE_CURVE ( 'NONE', #50349, #9679, #45109, .T. ) ;
#42961 = ORIENTED_EDGE ( 'NONE', *, *, #20476, .T. ) ;
#42962 = LINE ( 'NONE', #23351, #14777 ) ;
#42963 = ORIENTED_EDGE ( 'NONE', *, *, #31882, .T. ) ;
#42964 = LINE ( 'NONE', #4246, #36104 ) ;
#42965 = EDGE_CURVE ( 'NONE', #18815, #40626, #14911, .T. ) ;
#42966 = CARTESIAN_POINT ( 'NONE',  ( 0.000000000000000000, 1.585169487999011917, 0.000000000000000000 ) ) ;
#42967 = DIRECTION ( 'NONE',  ( 1.000000000000000000, -0.000000000000000000, 0.000000000000000000 ) ) ;
#42968 = ADVANCED_FACE ( 'NONE', ( #5889 ), #28740, .F. ) ;
#42969 = B_SPLINE_CURVE_WITH_KNOTS ( 'NONE', 3,
 ( #12102, #8229, #24489, #40239 ),
 .UNSPECIFIED., .F., .F.,
 ( 4, 4 ),
 ( 0.001547042765121542287, 0.004047202068159086626 ),
 .UNSPECIFIED. ) ;
#42970 = EDGE_LOOP ( 'NONE', ( #42991, #25145, #45697, #4408 ) ) ;
#42971 = VERTEX_POINT ( 'NONE', #23925 ) ;
#42972 = CARTESIAN_POINT ( 'NONE',  ( -1.636583440222563857, 3.267716535433071279, 2.839019714148966584E-16 ) ) ;
#42973 = CARTESIAN_POINT ( 'NONE',  ( 1.700185224778670401, 1.636708331897141377, -1.557456981387029149 ) ) ;
#42974 = DIRECTION ( 'NONE',  ( -0.000000000000000000, 1.000000000000000000, -0.000000000000000000 ) ) ;
#42975 = LINE ( 'NONE', #49933, #35926 ) ;
#42976 = DIRECTION ( 'NONE',  ( -0.9998717552508122886, -0.01601477604151185785, 0.000000000000000000 ) ) ;
#42977 = VECTOR ( 'NONE', #30344, 39.37007874015748143 ) ;
#42978 = DIRECTION ( 'NONE',  ( -1.000000000000000000, 0.000000000000000000, 0.000000000000000000 ) ) ;
#42979 = VECTOR ( 'NONE', #46839, 39.37007874015748143 ) ;
#42980 = VERTEX_POINT ( 'NONE', #43017 ) ;
#42981 = EDGE_CURVE ( 'NONE', #33170, #4557, #7169, .T. ) ;
#42982 = CARTESIAN_POINT ( 'NONE',  ( 2.950518610523430674, 1.446690190534351661, -0.1160880551001583216 ) ) ;
#42983 = CARTESIAN_POINT ( 'NONE',  ( -1.712496953225537188, 3.346456692913386100, 0.4724409448818871482 ) ) ;
#42984 = FACE_OUTER_BOUND ( 'NONE', #12208, .T. ) ;
#42985 = VECTOR ( 'NONE', #14675, 39.37007874015748143 ) ;
#42986 = EDGE_LOOP ( 'NONE', ( #45482, #14473, #716, #30425 ) ) ;
#42987 = ADVANCED_FACE ( 'NONE', ( #20033 ), #163, .F. ) ;
#42988 = DIRECTION ( 'NONE',  ( 0.5773502691896261751, 0.5773502691896261751, 0.5773502691896248429 ) ) ;
#42989 = ORIENTED_EDGE ( 'NONE', *, *, #31487, .T. ) ;
#42990 = VECTOR ( 'NONE', #39959, 39.37007874015748143 ) ;
#42991 = ORIENTED_EDGE ( 'NONE', *, *, #3776, .F. ) ;
#42992 = DIRECTION ( 'NONE',  ( -0.9998717552508122886, -0.01601477604151182316, 0.000000000000000000 ) ) ;
#42993 = VECTOR ( 'NONE', #6281, 39.37007874015748143 ) ;
#42994 = EDGE_LOOP ( 'NONE', ( #31718, #9911, #41506, #11309 ) ) ;
#42995 = VERTEX_POINT ( 'NONE', #46373 ) ;
#42996 = DIRECTION ( 'NONE',  ( -1.000000000000000000, -0.000000000000000000, -0.000000000000000000 ) ) ;
#42997 = ORIENTED_EDGE ( 'NONE', *, *, #26254, .F. ) ;
#42998 = CARTESIAN_POINT ( 'NONE',  ( 0.000000000000000000, 3.267716535433071279, -1.574803149606293529 ) ) ;
#42999 = B_SPLINE_CURVE_WITH_KNOTS ( 'NONE', 3,
 ( #24334, #1343, #48036, #21227 ),
 .UNSPECIFIED., .F., .F.,
 ( 4, 4 ),
 ( 0.01435888398627585376, 0.03074837528792711411 ),
 .UNSPECIFIED. ) ;
#43000 = EDGE_CURVE ( 'NONE', #22173, #7931, #22906, .T. ) ;
#43001 = CARTESIAN_POINT ( 'NONE',  ( 1.091055626815042423, 0.000000000000000000, -1.574803149606294417 ) ) ;
#43002 = LINE ( 'NONE', #7649, #21779 ) ;
#43003 = DIRECTION ( 'NONE',  ( -0.9998717552508122886, -0.01601477604151181275, 0.000000000000000000 ) ) ;
#43004 = B_SPLINE_CURVE_WITH_KNOTS ( 'NONE', 3,
 ( #43922, #570, #50854, #24061 ),
 .UNSPECIFIED., .F., .F.,
 ( 4, 4 ),
 ( 0.0006814467624810971891, 0.003181736896792887459 ),
 .UNSPECIFIED. ) ;
#43005 = DIRECTION ( 'NONE',  ( -0.5407162030609373726, -0.6444004775717706579, -0.5407162030609373726 ) ) ;
#43006 = DIRECTION ( 'NONE',  ( -3.986037398843765983E-20, -1.000000000000000000, -1.160734090543304660E-16 ) ) ;
#43007 = ORIENTED_EDGE ( 'NONE', *, *, #40933, .T. ) ;
#43008 = LINE ( 'NONE', #7909, #13463 ) ;
#43009 = CARTESIAN_POINT ( 'NONE',  ( 0.000000000000000000, 3.267716535433071279, 0.1574803149606286423 ) ) ;
#43010 = DIRECTION ( 'NONE',  ( 0.000000000000000000, -1.000000000000000000, -0.000000000000000000 ) ) ;
#43011 = VECTOR ( 'NONE', #40797, 39.37007874015748143 ) ;
#43012 = ORIENTED_EDGE ( 'NONE', *, *, #46557, .F. ) ;
#43013 = VECTOR ( 'NONE', #25357, 39.37007874015748143 ) ;
#43014 = CARTESIAN_POINT ( 'NONE',  ( 2.154397719472966433, 0.9909074813825916594, -1.481072863788291949 ) ) ;
#43015 = CARTESIAN_POINT ( 'NONE',  ( 0.000000000000000000, 2.755905511811024056, 0.000000000000000000 ) ) ;
#43016 = EDGE_LOOP ( 'NONE', ( #34568, #7897, #50896, #10412 ) ) ;
#43017 = CARTESIAN_POINT ( 'NONE',  ( -0.8942052331142552601, 3.346456692913386100, -1.889763779527552146 ) ) ;
#43018 = DIRECTION ( 'NONE',  ( -0.000000000000000000, 0.000000000000000000, 1.000000000000000000 ) ) ;
#43019 = VECTOR ( 'NONE', #11435, 39.37007874015748143 ) ;
#43020 = VECTOR ( 'NONE', #46095, 39.37007874015748854 ) ;
#43021 = LINE ( 'NONE', #7671, #5968 ) ;
#43022 = ORIENTED_EDGE ( 'NONE', *, *, #3617, .T. ) ;
#43023 = CARTESIAN_POINT ( 'NONE',  ( -1.247273217833388514, 0.007942302252338809612, -1.260601835943744087 ) ) ;
#43024 = EDGE_CURVE ( 'NONE', #5216, #16605, #38664, .T. ) ;
#43025 = CARTESIAN_POINT ( 'NONE',  ( 1.325491792074624087, 1.739919523179865202, -2.638988599164732385 ) ) ;
#43026 = VECTOR ( 'NONE', #4307, 39.37007874015748143 ) ;
#43027 = CARTESIAN_POINT ( 'NONE',  ( 0.5455278134075212115, 3.346456692913386100, -1.259842519685035134 ) ) ;
#43029 = EDGE_CURVE ( 'NONE', #32071, #45936, #35802, .T. ) ;
#43028 = DIRECTION ( 'NONE',  ( -3.469446951953613696E-16, 0.000000000000000000, -1.000000000000000000 ) ) ;
#43030 = ORIENTED_EDGE ( 'NONE', *, *, #21537, .F. ) ;
#43031 = EDGE_CURVE ( 'NONE', #6021, #11147, #47373, .T. ) ;
#43032 = ORIENTED_EDGE ( 'NONE', *, *, #5161, .T. ) ;
#43033 = EDGE_LOOP ( 'NONE', ( #48569, #19226, #33247, #8170 ) ) ;
#43034 = CARTESIAN_POINT ( 'NONE',  ( -0.2727639067037607723, 3.346456692913386100, 0.4724409448818869817 ) ) ;
#43035 = ORIENTED_EDGE ( 'NONE', *, *, #50514, .T. ) ;
#43036 = DIRECTION ( 'NONE',  ( 1.734723475976806848E-16, -0.000000000000000000, 1.000000000000000000 ) ) ;
#43037 = FACE_OUTER_BOUND ( 'NONE', #3100, .T. ) ;
#43038 = EDGE_LOOP ( 'NONE', ( #19351, #14042, #15007, #10104 ) ) ;
#43039 = DIRECTION ( 'NONE',  ( -3.469446951953613696E-16, 0.000000000000000000, -1.000000000000000000 ) ) ;
#43040 = ORIENTED_EDGE ( 'NONE', *, *, #40201, .F. ) ;
#43041 = CARTESIAN_POINT ( 'NONE',  ( 2.093903048064389427, 0.000000000000000000, -0.4274415146361335571 ) ) ;
#43042 = ORIENTED_EDGE ( 'NONE', *, *, #48742, .T. ) ;
#43043 = ORIENTED_EDGE ( 'NONE', *, *, #44895, .T. ) ;
#43044 = CARTESIAN_POINT ( 'NONE',  ( 0.8182917201112824834, 3.346456692913386100, 1.850393700787392293 ) ) ;
#43045 = VERTEX_POINT ( 'NONE', #34786 ) ;
#43046 = CIRCLE ( 'NONE', #7615, 1.850107469027523432 ) ;
#43047 = LINE ( 'NONE', #7449, #41062 ) ;
#43048 = EDGE_CURVE ( 'NONE', #22523, #36726, #15666, .T. ) ;
#43049 = ORIENTED_EDGE ( 'NONE', *, *, #49522, .T. ) ;
#43050 = ORIENTED_EDGE ( 'NONE', *, *, #25132, .F. ) ;
#43051 = DIRECTION ( 'NONE',  ( 0.000000000000000000, 1.000000000000000000, 0.000000000000000000 ) ) ;
#43052 = VECTOR ( 'NONE', #7194, 39.37007874015748143 ) ;
#43053 = CARTESIAN_POINT ( 'NONE',  ( -1.843409664576977303, 1.612759574255218986, -1.157856685511029715 ) ) ;
#43054 = ORIENTED_EDGE ( 'NONE', *, *, #36448, .T. ) ;
#43055 = VECTOR ( 'NONE', #47283, 39.37007874015748143 ) ;
#43056 = DIRECTION ( 'NONE',  ( 0.000000000000000000, -1.000000000000000000, 0.000000000000000000 ) ) ;
#43057 = EDGE_CURVE ( 'NONE', #30156, #50385, #31164, .T. ) ;
#43058 = VERTEX_POINT ( 'NONE', #50469 ) ;
#43059 = DIRECTION ( 'NONE',  ( 8.741157232058135226E-17, -1.000000000000000000, 7.636919086868543885E-17 ) ) ;
#43060 = VECTOR ( 'NONE', #49834, 39.37007874015748143 ) ;
#43061 = AXIS2_PLACEMENT_3D ( 'NONE', #9568, #34085, #30463 ) ;
#43062 = CARTESIAN_POINT ( 'NONE',  ( -1.363819533518803473, 3.267716535433071279, 1.535433070866133232 ) ) ;
#43063 = CARTESIAN_POINT ( 'NONE',  ( -1.195183497228115035E-16, 3.346456692913386100, 0.3149606299212576177 ) ) ;
#43064 = EDGE_LOOP ( 'NONE', ( #44057, #43249, #41919, #10991 ) ) ;
#43065 = ORIENTED_EDGE ( 'NONE', *, *, #10492, .T. ) ;
#43066 = DIRECTION ( 'NONE',  ( -1.000000000000000000, 0.000000000000000000, -0.000000000000000000 ) ) ;
#43067 = CARTESIAN_POINT ( 'NONE',  ( -0.3486774197067339376, 3.346456692913386100, -0.6299212598425175669 ) ) ;
#43068 = CARTESIAN_POINT ( 'NONE',  ( -0.6313959120844663264, 0.5236499866080164267, -2.102827561452275784 ) ) ;
#43069 = EDGE_CURVE ( 'NONE', #27482, #39685, #50488, .T. ) ;
#43070 = CARTESIAN_POINT ( 'NONE',  ( 2.309000164489917406, 1.744884814208895296, 0.2631132722234555410 ) ) ;
#43071 = ADVANCED_FACE ( 'NONE', ( #7419 ), #49312, .F. ) ;
#43072 = CARTESIAN_POINT ( 'NONE',  ( -0.4350747367504783636, 0.000000000000000000, -2.121846421795421378 ) ) ;
#43073 = FACE_OUTER_BOUND ( 'NONE', #28024, .T. ) ;
#43074 = ORIENTED_EDGE ( 'NONE', *, *, #37663, .F. ) ;
#43075 = DIRECTION ( 'NONE',  ( -3.986037398843765983E-20, -1.000000000000000000, -1.160734090543304660E-16 ) ) ;
#43076 = ORIENTED_EDGE ( 'NONE', *, *, #4490, .T. ) ;
#43077 = LINE ( 'NONE', #27848, #50575 ) ;
#43078 = ORIENTED_EDGE ( 'NONE', *, *, #38648, .T. ) ;
#43080 = EDGE_CURVE ( 'NONE', #18489, #46097, #30913, .T. ) ;
#43079 = EDGE_LOOP ( 'NONE', ( #15742, #48276, #38142, #35186 ) ) ;
#43081 = DIRECTION ( 'NONE',  ( 0.000000000000000000, 0.000000000000000000, -1.000000000000000000 ) ) ;
#43082 = CARTESIAN_POINT ( 'NONE',  ( -0.2727639067037607723, 0.000000000000000000, -1.417322834645664331 ) ) ;
#43083 = ORIENTED_EDGE ( 'NONE', *, *, #37836, .T. ) ;
#43084 = ADVANCED_FACE ( 'NONE', ( #19277 ), #23664, .F. ) ;
#43085 = EDGE_CURVE ( 'NONE', #49411, #22546, #11540, .T. ) ;
#43086 = VECTOR ( 'NONE', #48293, 39.37007874015748143 ) ;
#43087 = DIRECTION ( 'NONE',  ( 1.000000000000000000, -0.000000000000000000, 0.000000000000000000 ) ) ;
#43088 = ORIENTED_EDGE ( 'NONE', *, *, #42170, .T. ) ;
#43089 = FACE_OUTER_BOUND ( 'NONE', #18250, .T. ) ;
#43090 = ORIENTED_EDGE ( 'NONE', *, *, #40517, .F. ) ;
#43091 = CIRCLE ( 'NONE', #15110, 2.164630168518208109 ) ;
#43092 = VECTOR ( 'NONE', #49777, 39.37007874015748143 ) ;
#43093 = PLANE ( 'NONE',  #16140 ) ;
#43094 = CARTESIAN_POINT ( 'NONE',  ( 0.2727639067037604947, 0.000000000000000000, 0.1574803149606283648 ) ) ;
#43095 = EDGE_CURVE ( 'NONE', #7950, #45913, #27276, .T. ) ;
#43096 = ORIENTED_EDGE ( 'NONE', *, *, #14852, .F. ) ;
#43097 = VECTOR ( 'NONE', #49212, 39.37007874015748143 ) ;
#43098 = LINE ( 'NONE', #7744, #4919 ) ;
#43099 = VERTEX_POINT ( 'NONE', #27530 ) ;
#43100 = ORIENTED_EDGE ( 'NONE', *, *, #31140, .T. ) ;
#43101 = CARTESIAN_POINT ( 'NONE',  ( -0.4414517166633473710, 0.5234905560015207238, 2.156986477457879747 ) ) ;
#43102 = DIRECTION ( 'NONE',  ( -0.000000000000000000, 0.000000000000000000, 1.000000000000000000 ) ) ;
#43103 = CARTESIAN_POINT ( 'NONE',  ( 2.951990591674675368, 1.765258879000601855, -0.08331184815398361143 ) ) ;
#43104 = ORIENTED_EDGE ( 'NONE', *, *, #42014, .T. ) ;
#43105 = LINE ( 'NONE', #11378, #18788 ) ;
#43106 = DIRECTION ( 'NONE',  ( -0.01601477604151182663, 0.9998717552508123996, -0.000000000000000000 ) ) ;
#43107 = EDGE_CURVE ( 'NONE', #33385, #30631, #11788, .T. ) ;
#43108 = ORIENTED_EDGE ( 'NONE', *, *, #45976, .F. ) ;
#43109 = DIRECTION ( 'NONE',  ( -3.469446951953613696E-16, 0.000000000000000000, -1.000000000000000000 ) ) ;
#43110 = VERTEX_POINT ( 'NONE', #19529 ) ;
#43111 = ORIENTED_EDGE ( 'NONE', *, *, #17693, .T. ) ;
#43112 = CARTESIAN_POINT ( 'NONE',  ( 1.865899819297162532, 29.40509435798275106, 74.47845804085073951 ) ) ;
#43113 = EDGE_CURVE ( 'NONE', #23957, #4956, #43272, .T. ) ;
#43114 = EDGE_LOOP ( 'NONE', ( #18729, #30836, #32589, #11602 ) ) ;
#43115 = DIRECTION ( 'NONE',  ( 0.000000000000000000, 1.160734090543304660E-16, -1.000000000000000000 ) ) ;
#43116 = CARTESIAN_POINT ( 'NONE',  ( -2.032045338671488288, 3.346456692913386100, 0.7480314960629874665 ) ) ;
#43117 = EDGE_CURVE ( 'NONE', #45764, #30593, #35546, .T. ) ;
#43118 = EDGE_CURVE ( 'NONE', #46760, #38185, #25201, .T. ) ;
#43119 = PLANE ( 'NONE',  #27545 ) ;
#43120 = CARTESIAN_POINT ( 'NONE',  ( -0.3486774197067334380, 3.346456692913386100, 0.9448818897637749625 ) ) ;
#43121 = VERTEX_POINT ( 'NONE', #36062 ) ;
#43122 = EDGE_LOOP ( 'NONE', ( #1632, #25466, #23731, #7030 ) ) ;
#43123 = VECTOR ( 'NONE', #25860, 39.37007874015748143 ) ;
#43124 = CARTESIAN_POINT ( 'NONE',  ( -2.427212287055287909, 1.673239622219053535, -0.05974402731829655394 ) ) ;
#43125 = VECTOR ( 'NONE', #12244, 39.37007874015748143 ) ;
#43126 = ORIENTED_EDGE ( 'NONE', *, *, #39545, .T. ) ;
#43127 = CARTESIAN_POINT ( 'NONE',  ( -1.636583440222563635, 0.000000000000000000, 0.4330708661417290162 ) ) ;
#43128 = DIRECTION ( 'NONE',  ( 0.000000000000000000, -1.000000000000000000, 0.000000000000000000 ) ) ;
#43129 = AXIS2_PLACEMENT_3D ( 'NONE', #12868, #474, #16226 ) ;
#43130 = LINE ( 'NONE', #27639, #50279 ) ;
#43131 = VECTOR ( 'NONE', #45988, 39.37007874015748143 ) ;
#43132 = CARTESIAN_POINT ( 'NONE',  ( -0.5455278134075208785, 0.000000000000000000, 1.259842519685033357 ) ) ;
#43133 = DIRECTION ( 'NONE',  ( -0.4338837391175656699, 0.000000000000000000, 0.9009688679024154823 ) ) ;
#43134 = DIRECTION ( 'NONE',  ( -1.000000000000000000, 0.000000000000000000, -0.000000000000000000 ) ) ;
#43135 = CIRCLE ( 'NONE', #38238, 2.106299212598425008 ) ;
#43136 = VERTEX_POINT ( 'NONE', #1198 ) ;
#43137 = DIRECTION ( 'NONE',  ( -0.9998717552508121775, -0.01601477604151182316, 0.000000000000000000 ) ) ;
#43138 = SURFACE_STYLE_FILL_AREA ( #19896 ) ;
#43139 = EDGE_CURVE ( 'NONE', #16462, #44897, #44552, .T. ) ;
#43140 = ORIENTED_EDGE ( 'NONE', *, *, #17304, .F. ) ;
#43141 = ORIENTED_EDGE ( 'NONE', *, *, #15016, .F. ) ;
#43142 = FACE_OUTER_BOUND ( 'NONE', #19403, .T. ) ;
#43143 = DIRECTION ( 'NONE',  ( 1.000000000000000000, 0.000000000000000000, 0.000000000000000000 ) ) ;
#43144 = FACE_OUTER_BOUND ( 'NONE', #9394, .T. ) ;
#43145 = ORIENTED_EDGE ( 'NONE', *, *, #18170, .T. ) ;
#43146 = EDGE_CURVE ( 'NONE', #23992, #22341, #5650, .T. ) ;
#43147 = ADVANCED_FACE ( 'NONE', ( #17205 ), #941, .F. ) ;
#43148 = EDGE_CURVE ( 'NONE', #13391, #23287, #28300, .T. ) ;
#43149 = ORIENTED_EDGE ( 'NONE', *, *, #33657, .F. ) ;
#43150 = DIRECTION ( 'NONE',  ( 0.000000000000000000, 1.160734090543304660E-16, -1.000000000000000000 ) ) ;
#43151 = ORIENTED_EDGE ( 'NONE', *, *, #4039, .T. ) ;
#43152 = DIRECTION ( 'NONE',  ( -0.7530714660036196273, -1.160734090543304907E-16, 0.6579387259397027066 ) ) ;
#43153 = ORIENTED_EDGE ( 'NONE', *, *, #14498, .T. ) ;
#43154 = CARTESIAN_POINT ( 'NONE',  ( -1.236813753895213086, 1.601547340627394567, -2.681693691597581974 ) ) ;
#43155 = CARTESIAN_POINT ( 'NONE',  ( 0.5455278134075217666, 0.000000000000000000, 2.204724409448808764 ) ) ;
#43156 = DIRECTION ( 'NONE',  ( 1.734723475976806848E-16, -0.000000000000000000, 1.000000000000000000 ) ) ;
#43157 = VERTEX_POINT ( 'NONE', #24185 ) ;
#43158 = VECTOR ( 'NONE', #32543, 39.37007874015748143 ) ;
#43159 = VERTEX_POINT ( 'NONE', #8686 ) ;
#43160 = ORIENTED_EDGE ( 'NONE', *, *, #26070, .T. ) ;
#43161 = CARTESIAN_POINT ( 'NONE',  ( 0.5455278134075211005, 0.000000000000000000, 0.7480314960629872445 ) ) ;
#43162 = FACE_OUTER_BOUND ( 'NONE', #40892, .T. ) ;
#43163 = VERTEX_POINT ( 'NONE', #40958 ) ;
#43164 = ORIENTED_EDGE ( 'NONE', *, *, #33508, .F. ) ;
#43165 = CARTESIAN_POINT ( 'NONE',  ( 1.091055626815042645, 3.346456692913386100, 0.3149606299212578953 ) ) ;
#43166 = DIRECTION ( 'NONE',  ( 1.734723475976806848E-16, -0.000000000000000000, 1.000000000000000000 ) ) ;
#43167 = CARTESIAN_POINT ( 'NONE',  ( -2.145839806594207033, 0.5252136644077377570, -0.04710757465011475298 ) ) ;
#43168 = VECTOR ( 'NONE', #31364, 39.37007874015748143 ) ;
#43169 = VECTOR ( 'NONE', #14465, 39.37007874015748143 ) ;
#43170 = VERTEX_POINT ( 'NONE', #5582 ) ;
#43171 = EDGE_LOOP ( 'NONE', ( #39653, #50755, #3306, #6300 ) ) ;
#43172 = PLANE ( 'NONE',  #3204 ) ;
#43173 = CARTESIAN_POINT ( 'NONE',  ( -2.071704270381554913, 3.267716535433071279, -0.6299212598425177889 ) ) ;
#43174 = PLANE ( 'NONE',  #13819 ) ;
#43175 = VERTEX_POINT ( 'NONE', #28555 ) ;
#43176 = DIRECTION ( 'NONE',  ( -0.000000000000000000, 0.000000000000000000, 1.000000000000000000 ) ) ;
#43177 = CARTESIAN_POINT ( 'NONE',  ( -2.182111253630085290, 3.267716535433071279, 0.4330708661417290162 ) ) ;
#43178 = AXIS2_PLACEMENT_3D ( 'NONE', #41082, #1315, #29190 ) ;
#43179 = ORIENTED_EDGE ( 'NONE', *, *, #47002, .F. ) ;
#43180 = CARTESIAN_POINT ( 'NONE',  ( 0.8182917201112817063, 3.346456692913386100, -1.929133858267711110 ) ) ;
#43181 = ORIENTED_EDGE ( 'NONE', *, *, #12033, .F. ) ;
#43182 = ORIENTED_EDGE ( 'NONE', *, *, #38815, .T. ) ;
#43183 = CARTESIAN_POINT ( 'NONE',  ( -1.636583440222564301, 0.000000000000000000, 1.574803149606291530 ) ) ;
#43184 = CARTESIAN_POINT ( 'NONE',  ( 2.949782676795221992, 0.000000000000000000, -0.1324748927672375898 ) ) ;
#43185 = CARTESIAN_POINT ( 'NONE',  ( 1.536664496436161003E-16, 3.267716535433071279, -2.665687976667886873E-32 ) ) ;
#43186 = EDGE_CURVE ( 'NONE', #48785, #11136, #36831, .T. ) ;
#43187 = DIRECTION ( 'NONE',  ( -0.000000000000000000, 1.000000000000000000, -0.000000000000000000 ) ) ;
#43188 = LINE ( 'NONE', #43446, #14776 ) ;
#43189 = ORIENTED_EDGE ( 'NONE', *, *, #146, .T. ) ;
#43191 = EDGE_CURVE ( 'NONE', #20798, #3180, #21334, .T. ) ;
#43190 = ORIENTED_EDGE ( 'NONE', *, *, #48119, .T. ) ;
#43192 = EDGE_LOOP ( 'NONE', ( #44084, #913, #44557, #43601 ) ) ;
#43193 = DIRECTION ( 'NONE',  ( -1.000000000000000000, 0.000000000000000000, -0.000000000000000000 ) ) ;
#43194 = CARTESIAN_POINT ( 'NONE',  ( 1.087963734054938625, 1.205361022782829114E-17, 1.724994741719410918 ) ) ;
#43195 =( GEOMETRIC_REPRESENTATION_CONTEXT ( 3 ) GLOBAL_UNCERTAINTY_ASSIGNED_CONTEXT ( ( #24678 ) ) GLOBAL_UNIT_ASSIGNED_CONTEXT ( ( #5490, #48563, #48808 ) ) REPRESENTATION_CONTEXT ( 'NONE', 'WORKASPACE' ) );
#43196 = CARTESIAN_POINT ( 'NONE',  ( -1.712496953225537188, 3.346456692913386100, -0.1574803149606297248 ) ) ;
#43197 = CARTESIAN_POINT ( 'NONE',  ( 1.956192433058983493, 0.05925166736471587647, -0.03859050128386512513 ) ) ;
#43198 = ORIENTED_EDGE ( 'NONE', *, *, #48842, .T. ) ;
#43199 = DIRECTION ( 'NONE',  ( 0.000000000000000000, 1.000000000000000000, 0.000000000000000000 ) ) ;
#43200 = B_SPLINE_CURVE_WITH_KNOTS ( 'NONE', 3,
 ( #11275, #27511, #37709, #42757 ),
 .UNSPECIFIED., .F., .F.,
 ( 4, 4 ),
 ( 0.01311645403109486761, 0.03074129349619527524 ),
 .UNSPECIFIED. ) ;
#43201 = AXIS2_PLACEMENT_3D ( 'NONE', #44311, #17216, #40708 ) ;
#43202 = EDGE_CURVE ( 'NONE', #8694, #18289, #35351, .T. ) ;
#43203 = DIRECTION ( 'NONE',  ( -3.469446951953613696E-16, 0.000000000000000000, -1.000000000000000000 ) ) ;
#43204 = AXIS2_PLACEMENT_3D ( 'NONE', #41906, #30027, #10411 ) ;
#43205 = VECTOR ( 'NONE', #21904, 39.37007874015748143 ) ;
#43206 = ORIENTED_EDGE ( 'NONE', *, *, #26540, .T. ) ;
#43207 = CARTESIAN_POINT ( 'NONE',  ( 1.499921196763806419, 3.267716535433071279, -1.929133858267710666 ) ) ;
#43208 = ADVANCED_FACE ( 'NONE', ( #40192 ), #29064, .F. ) ;
#43209 = CARTESIAN_POINT ( 'NONE',  ( 2.323794147221719175, 1.745121766917047790, -0.05509951330290247667 ) ) ;
#43210 = CARTESIAN_POINT ( 'NONE',  ( -0.3595914698493425377, 0.000000000000000000, 1.705899337635481405 ) ) ;
#43211 = ORIENTED_EDGE ( 'NONE', *, *, #21994, .T. ) ;
#43212 = DIRECTION ( 'NONE',  ( 0.000000000000000000, 1.000000000000000000, 0.000000000000000000 ) ) ;
#43213 = CARTESIAN_POINT ( 'NONE',  ( -0.3486774197067334935, 3.346456692913386100, 1.377952755905504256 ) ) ;
#43214 = CARTESIAN_POINT ( 'NONE',  ( -2.182111253630085734, 3.346456692913386100, -1.141732283464563791 ) ) ;
#43215 = VECTOR ( 'NONE', #46564, 39.37007874015748143 ) ;
#43216 = B_SPLINE_CURVE_WITH_KNOTS ( 'NONE', 3,
 ( #529, #35902, #24794, #44145 ),
 .UNSPECIFIED., .F., .F.,
 ( 4, 4 ),
 ( 0.01457548150641458512, 0.03074977565575078009 ),
 .UNSPECIFIED. ) ;
#43217 = ADVANCED_FACE ( 'NONE', ( #20564 ), #44304, .F. ) ;
#43218 = ORIENTED_EDGE ( 'NONE', *, *, #17846, .T. ) ;
#43219 = LINE ( 'NONE', #40396, #37899 ) ;
#43220 = ORIENTED_EDGE ( 'NONE', *, *, #16532, .F. ) ;
#43221 = PLANE ( 'NONE',  #22907 ) ;
#43222 = FACE_OUTER_BOUND ( 'NONE', #41171, .T. ) ;
#43223 = LINE ( 'NONE', #15113, #6237 ) ;
#43224 = EDGE_LOOP ( 'NONE', ( #33223, #4655, #7348, #15822 ) ) ;
#43225 = EDGE_LOOP ( 'NONE', ( #40859, #38427, #4639, #49595 ) ) ;
#43226 = DIRECTION ( 'NONE',  ( 0.000000000000000000, 1.000000000000000000, 0.000000000000000000 ) ) ;
#43227 = CARTESIAN_POINT ( 'NONE',  ( -1.091055626815042645, 3.267716535433071279, -0.9448818897637760728 ) ) ;
#43228 = ORIENTED_EDGE ( 'NONE', *, *, #44940, .T. ) ;
#43229 = CARTESIAN_POINT ( 'NONE',  ( 0.8182917201112824834, 0.000000000000000000, 1.417322834645662777 ) ) ;
#43230 = DIRECTION ( 'NONE',  ( 1.734723475976806848E-16, 0.000000000000000000, 1.000000000000000000 ) ) ;
#43231 = PLANE ( 'NONE',  #39238 ) ;
#43232 = DIRECTION ( 'NONE',  ( 0.4738686624729965269, 1.288287287306305283E-16, 0.8805955318567391110 ) ) ;
#43233 = ORIENTED_EDGE ( 'NONE', *, *, #36454, .T. ) ;
#43234 = ORIENTED_EDGE ( 'NONE', *, *, #15068, .T. ) ;
#43235 = DIRECTION ( 'NONE',  ( 1.000000000000000000, -0.000000000000000000, 0.000000000000000000 ) ) ;
#43236 = PLANE ( 'NONE',  #128 ) ;
#43237 = CONICAL_SURFACE ( 'NONE', #48964, 3.483074324928249421, 1.244861948955335196 ) ;
#43238 = EDGE_LOOP ( 'NONE', ( #11784, #9602, #14491, #249 ) ) ;
#43239 = CARTESIAN_POINT ( 'NONE',  ( 2.150824344285287459, 1.742351338968239238, -0.8657870173518766865 ) ) ;
#43240 = VECTOR ( 'NONE', #33845, 39.37007874015748143 ) ;
#43241 = ORIENTED_EDGE ( 'NONE', *, *, #17627, .T. ) ;
#43242 = EDGE_LOOP ( 'NONE', ( #5026, #6445, #43806, #38316 ) ) ;
#43243 = DIRECTION ( 'NONE',  ( -3.469446951953613696E-16, 0.000000000000000000, -1.000000000000000000 ) ) ;
#43244 = VECTOR ( 'NONE', #21596, 39.37007874015748143 ) ;
#43245 = VECTOR ( 'NONE', #15851, 39.37007874015748143 ) ;
#43246 = ORIENTED_EDGE ( 'NONE', *, *, #31370, .F. ) ;
#43247 = ORIENTED_EDGE ( 'NONE', *, *, #22577, .T. ) ;
#43248 = CARTESIAN_POINT ( 'NONE',  ( 2.106197740627112402, 3.267716535433071279, 0.02067487291359298637 ) ) ;
#43249 = ORIENTED_EDGE ( 'NONE', *, *, #37184, .T. ) ;
#43250 = EDGE_CURVE ( 'NONE', #3960, #28934, #16698, .T. ) ;
#43251 = VECTOR ( 'NONE', #5336, 39.37007874015748143 ) ;
#43252 = EDGE_CURVE ( 'NONE', #43798, #50288, #20122, .T. ) ;
#43253 = CARTESIAN_POINT ( 'NONE',  ( 1.915720322920900331, 0.05860343245220329955, -0.3867724703730804348 ) ) ;
#43254 = CARTESIAN_POINT ( 'NONE',  ( 0.2431224069212723493, 0.000000000000000000, 2.152304290637673034 ) ) ;
#43255 = ADVANCED_FACE ( 'NONE', ( #16182 ), #48393, .F. ) ;
#43256 = CARTESIAN_POINT ( 'NONE',  ( 2.276001286114500477, 1.711547877995502231, -0.4690042491690135096 ) ) ;
#43257 = ADVANCED_FACE ( 'NONE', ( #12309 ), #24947, .F. ) ;
#43258 = DIRECTION ( 'NONE',  ( -0.8584487936018655452, 0.000000000000000000, -0.5128992774059071280 ) ) ;
#43259 = DIRECTION ( 'NONE',  ( 0.000000000000000000, 0.000000000000000000, -1.000000000000000000 ) ) ;
#43260 = CARTESIAN_POINT ( 'NONE',  ( -0.2727639067037608278, 3.346456692913386100, 0.2755905511810995412 ) ) ;
#43261 = ORIENTED_EDGE ( 'NONE', *, *, #18900, .T. ) ;
#43262 = DIRECTION ( 'NONE',  ( 0.000000000000000000, -1.000000000000000000, 0.000000000000000000 ) ) ;
#43263 = LINE ( 'NONE', #23148, #34274 ) ;
#43264 = CARTESIAN_POINT ( 'NONE',  ( 0.2727639067037606613, 3.267716535433071279, -4.731699523581610974E-17 ) ) ;
#43265 = VERTEX_POINT ( 'NONE', #8435 ) ;
#43266 = LINE ( 'NONE', #23661, #23178 ) ;
#43267 = EDGE_CURVE ( 'NONE', #17956, #2104, #23800, .T. ) ;
#43268 = B_SPLINE_CURVE_WITH_KNOTS ( 'NONE', 3,
 ( #46215, #11627, #10872, #26614 ),
 .UNSPECIFIED., .F., .F.,
 ( 4, 4 ),
 ( 0.1211775127643062444, 0.1625894504277921315 ),
 .UNSPECIFIED. ) ;
#43269 = ADVANCED_FACE ( 'NONE', ( #6851 ), #2721, .T. ) ;
#43270 = DIRECTION ( 'NONE',  ( -0.8660254037844362651, 0.000000000000000000, 0.5000000000000039968 ) ) ;
#43271 = ORIENTED_EDGE ( 'NONE', *, *, #50118, .T. ) ;
#43272 = LINE ( 'NONE', #7919, #27078 ) ;
#43273 = PLANE ( 'NONE',  #32554 ) ;
#43274 = CARTESIAN_POINT ( 'NONE',  ( 1.909347346926324684, 3.267716535433071279, -3.312189666507128175E-16 ) ) ;
#43275 = VECTOR ( 'NONE', #38220, 39.37007874015748854 ) ;
#43276 = VECTOR ( 'NONE', #13415, 39.37007874015748143 ) ;
#43277 = EDGE_CURVE ( 'NONE', #47459, #17713, #30350, .T. ) ;
#43278 = VECTOR ( 'NONE', #5950, 39.37007874015748143 ) ;
#43279 = DIRECTION ( 'NONE',  ( 1.734723475976806848E-16, -0.000000000000000000, 1.000000000000000000 ) ) ;
#43280 = ORIENTED_EDGE ( 'NONE', *, *, #35788, .F. ) ;
#43281 = LINE ( 'NONE', #3550, #26452 ) ;
#43282 = AXIS2_PLACEMENT_3D ( 'NONE', #16124, #31889, #47578 ) ;
#43283 = CARTESIAN_POINT ( 'NONE',  ( 0.4696143004045484903, 3.267716535433071279, 1.732283464566921172 ) ) ;
#43284 = DIRECTION ( 'NONE',  ( 1.000000000000000000, 0.000000000000000000, 0.000000000000000000 ) ) ;
#43285 = CARTESIAN_POINT ( 'NONE',  ( 0.000000000000000000, 3.267716535433071279, 0.000000000000000000 ) ) ;
#43286 = ORIENTED_EDGE ( 'NONE', *, *, #26829, .T. ) ;
#43287 = AXIS2_PLACEMENT_3D ( 'NONE', #43730, #24897, #40644 ) ;
#43288 = ORIENTED_EDGE ( 'NONE', *, *, #22621, .T. ) ;
#43289 = ORIENTED_EDGE ( 'NONE', *, *, #854, .F. ) ;
#43290 = CARTESIAN_POINT ( 'NONE',  ( 0.8182917201112819283, 3.346456692913386100, 0.9055118110236164419 ) ) ;
#43291 = ORIENTED_EDGE ( 'NONE', *, *, #2010, .F. ) ;
#43292 = CARTESIAN_POINT ( 'NONE',  ( -0.7328193673159020260, 1.696164507524817511, 2.092647490920610309 ) ) ;
#43293 = FACE_OUTER_BOUND ( 'NONE', #33936, .T. ) ;
#43294 = EDGE_CURVE ( 'NONE', #1152, #19232, #33731, .T. ) ;
#43295 = ORIENTED_EDGE ( 'NONE', *, *, #37187, .F. ) ;
#43296 = DIRECTION ( 'NONE',  ( 0.000000000000000000, 0.000000000000000000, -1.000000000000000000 ) ) ;
#43297 = ORIENTED_EDGE ( 'NONE', *, *, #27520, .F. ) ;
#43298 = CARTESIAN_POINT ( 'NONE',  ( -1.909347346926324906, 3.267716535433071279, 1.417322834645662333 ) ) ;
#43299 = CARTESIAN_POINT ( 'NONE',  ( 1.499921196763806419, 3.267716535433071279, -1.929133858267710666 ) ) ;
#43300 = ORIENTED_EDGE ( 'NONE', *, *, #32860, .F. ) ;
#43301 = VERTEX_POINT ( 'NONE', #29588 ) ;
#43302 = CARTESIAN_POINT ( 'NONE',  ( 0.4435105686220199295, 5.905511811023623991, 2.168331686854577889 ) ) ;
#43303 = ORIENTED_EDGE ( 'NONE', *, *, #15940, .T. ) ;
#43304 = DIRECTION ( 'NONE',  ( 1.734723475976806848E-16, -0.000000000000000000, 1.000000000000000000 ) ) ;
#43305 = VERTEX_POINT ( 'NONE', #42209 ) ;
#43306 = VERTEX_POINT ( 'NONE', #1964 ) ;
#43307 = LINE ( 'NONE', #23701, #21557 ) ;
#43308 = VECTOR ( 'NONE', #45231, 39.37007874015748143 ) ;
#43309 = EDGE_CURVE ( 'NONE', #49899, #2298, #29840, .T. ) ;
#43310 = CARTESIAN_POINT ( 'NONE',  ( 4.268512490100411402E-16, 0.000000000000000000, 0.9448818897637749625 ) ) ;
#43311 = VECTOR ( 'NONE', #25456, 39.37007874015748143 ) ;
#43312 = VERTEX_POINT ( 'NONE', #33478 ) ;
#43313 = CARTESIAN_POINT ( 'NONE',  ( 0.1067246931122726866, 0.02962905676920215767, 0.000000000000000000 ) ) ;
#43314 = AXIS2_PLACEMENT_3D ( 'NONE', #5722, #41097, #21725 ) ;
#43315 = EDGE_LOOP ( 'NONE', ( #22813, #30509, #12322, #48774, #28418, #27747, #17675, #24827, #45712, #19651, #41459 ) ) ;
#43316 = DIRECTION ( 'NONE',  ( -0.7818314824680309139, 0.000000000000000000, 0.6234898018587318180 ) ) ;
#43317 = EDGE_CURVE ( 'NONE', #28387, #47614, #45554, .T. ) ;
#43318 = DIRECTION ( 'NONE',  ( 0.000000000000000000, -1.000000000000000000, 0.000000000000000000 ) ) ;
#43319 = EDGE_CURVE ( 'NONE', #41767, #18572, #25965, .T. ) ;
#43320 = VECTOR ( 'NONE', #32802, 39.37007874015748143 ) ;
#43321 = EDGE_CURVE ( 'NONE', #9931, #33373, #33218, .T. ) ;
#43322 = DIRECTION ( 'NONE',  ( -0.000000000000000000, 1.000000000000000000, -0.000000000000000000 ) ) ;
#43323 = ORIENTED_EDGE ( 'NONE', *, *, #31920, .F. ) ;
#43324 = EDGE_LOOP ( 'NONE', ( #18969, #7634, #8703, #30091 ) ) ;
#43325 = VECTOR ( 'NONE', #9661, 39.37007874015748143 ) ;
#43326 = CARTESIAN_POINT ( 'NONE',  ( 0.8182917201112819283, 3.267716535433071279, -1.419509857074483292E-16 ) ) ;
#43327 = CARTESIAN_POINT ( 'NONE',  ( 1.363819533518803029, 3.346456692913386100, -1.102362204724405714 ) ) ;
#43328 = CARTESIAN_POINT ( 'NONE',  ( 4.268512490100411402E-16, 3.346456692913386100, 1.574803149606291974 ) ) ;
#43329 = DIRECTION ( 'NONE',  ( 0.3513748240813434620, 1.086579671787963332E-16, -0.9362348706397368714 ) ) ;
#43330 = LINE ( 'NONE', #23720, #26451 ) ;
#43331 = DIRECTION ( 'NONE',  ( -0.000000000000000000, -1.000000000000000000, -0.000000000000000000 ) ) ;
#43332 = ADVANCED_FACE ( 'NONE', ( #13840 ), #49662, .F. ) ;
#43333 = ORIENTED_EDGE ( 'NONE', *, *, #33540, .F. ) ;
#43334 = DIRECTION ( 'NONE',  ( -0.000000000000000000, 1.000000000000000000, -0.000000000000000000 ) ) ;
#43335 = ORIENTED_EDGE ( 'NONE', *, *, #35650, .T. ) ;
#43336 = LINE ( 'NONE', #50779, #16860 ) ;
#43337 = EDGE_CURVE ( 'NONE', #31565, #24019, #41714, .T. ) ;
#43338 = ORIENTED_EDGE ( 'NONE', *, *, #7278, .F. ) ;
#43339 = PLANE ( 'NONE',  #31654 ) ;
#43340 = B_SPLINE_CURVE_WITH_KNOTS ( 'NONE', 3,
 ( #27788, #11789, #7420, #18786 ),
 .UNSPECIFIED., .F., .F.,
 ( 4, 4 ),
 ( 0.001850897396926462404, 0.04526678932488142210 ),
 .UNSPECIFIED. ) ;
#43341 = DIRECTION ( 'NONE',  ( 1.734723475976806848E-16, -0.000000000000000000, 1.000000000000000000 ) ) ;
#43342 = ORIENTED_EDGE ( 'NONE', *, *, #26096, .T. ) ;
#43343 = EDGE_CURVE ( 'NONE', #12429, #18859, #42888, .T. ) ;
#43344 = CARTESIAN_POINT ( 'NONE',  ( 1.091055626815042423, 3.346456692913386100, -1.456692913385822630 ) ) ;
#43345 = VECTOR ( 'NONE', #36046, 39.37007874015748143 ) ;
#43346 = ORIENTED_EDGE ( 'NONE', *, *, #21707, .F. ) ;
#43347 = CARTESIAN_POINT ( 'NONE',  ( 0.2727639067037604392, 0.000000000000000000, 0.5905511811023579360 ) ) ;
#43348 = EDGE_CURVE ( 'NONE', #1059, #4594, #41460, .T. ) ;
#43349 = AXIS2_PLACEMENT_3D ( 'NONE', #17534, #6871, #46829 ) ;
#43350 = EDGE_LOOP ( 'NONE', ( #9653, #10679, #37914, #35269 ) ) ;
#43351 = CARTESIAN_POINT ( 'NONE',  ( -0.07591351300297277671, 3.346456692913386100, 2.047244094488179567 ) ) ;
#43352 = DIRECTION ( 'NONE',  ( 1.000000000000000000, -0.000000000000000000, 0.000000000000000000 ) ) ;
#43353 = VECTOR ( 'NONE', #32525, 39.37007874015748143 ) ;
#43354 = B_SPLINE_CURVE_WITH_KNOTS ( 'NONE', 3,
 ( #21639, #17765, #33532, #45359 ),
 .UNSPECIFIED., .F., .F.,
 ( 4, 4 ),
 ( 6.352633626275700509E-07, 0.003169472943232748419 ),
 .UNSPECIFIED. ) ;
#43355 = EDGE_LOOP ( 'NONE', ( #37991, #13760, #18308, #45846, #40595, #35467, #4053, #40718, #39903, #36808, #17042, #5211, #28849, #16586, #27940, #21210, #10166, #35676, #32301, #43247, #18196, #10368, #43974, #13141, #3738, #37792, #31399, #3146, #8773, #9856, #39844, #43303, #7016, #39114, #5498, #20654, #20125, #46730, #19108, #21397, #4985, #32217, #23549, #3971, #31818, #22576, #30862, #2279, #18852, #17743, #13271, #3346, #41628, #27253, #34262, #22664, #21609, #11370, #24419, #8831, #10754, #7925, #20768, #3374, #4368, #43521, #8476, #22674, #29356, #19542, #2916 ) ) ;
#43356 = VECTOR ( 'NONE', #9219, 39.37007874015748143 ) ;
#43357 = DIRECTION ( 'NONE',  ( 0.04486483035050446017, -1.159583191840067383E-16, 0.9989930665413151445 ) ) ;
#43358 = ORIENTED_EDGE ( 'NONE', *, *, #38723, .T. ) ;
#43359 = ORIENTED_EDGE ( 'NONE', *, *, #38667, .F. ) ;
#43360 = EDGE_CURVE ( 'NONE', #18949, #5207, #48902, .T. ) ;
#43361 = DIRECTION ( 'NONE',  ( -1.000000000000000000, -0.000000000000000000, -1.734839586111147395E-16 ) ) ;
#43362 = LINE ( 'NONE', #8001, #26493 ) ;
#43363 = DIRECTION ( 'NONE',  ( 1.734723475976806848E-16, -0.000000000000000000, 1.000000000000000000 ) ) ;
#43364 = EDGE_CURVE ( 'NONE', #16143, #370, #13591, .T. ) ;
#43365 = ORIENTED_EDGE ( 'NONE', *, *, #17184, .T. ) ;
#43366 = DIRECTION ( 'NONE',  ( -0.000000000000000000, 1.000000000000000000, -0.000000000000000000 ) ) ;
#43367 = CARTESIAN_POINT ( 'NONE',  ( -1.500384104887378278, 1.695869373643325906, 2.543203506785173040 ) ) ;
#43368 = VERTEX_POINT ( 'NONE', #45807 ) ;
#43369 = CARTESIAN_POINT ( 'NONE',  ( 0.2727639067037608278, 3.267716535433071279, -4.731699523581614055E-17 ) ) ;
#43370 = ORIENTED_EDGE ( 'NONE', *, *, #7443, .T. ) ;
#43371 = EDGE_LOOP ( 'NONE', ( #45092, #7871, #31688, #16382 ) ) ;
#43372 = ORIENTED_EDGE ( 'NONE', *, *, #6730, .F. ) ;
#43373 = CARTESIAN_POINT ( 'NONE',  ( 4.268512490100411402E-16, 3.346456692913386100, 1.574803149606291974 ) ) ;
#43374 = EDGE_CURVE ( 'NONE', #25574, #39964, #17714, .T. ) ;
#43375 = DIRECTION ( 'NONE',  ( -1.000000000000000000, 0.000000000000000000, -0.000000000000000000 ) ) ;
#43377 = CARTESIAN_POINT ( 'NONE',  ( -1.636583440222564301, 0.000000000000000000, -0.9448818897637762948 ) ) ;
#43376 = AXIS2_PLACEMENT_3D ( 'NONE', #36753, #29246, #41140 ) ;
#43378 = EDGE_CURVE ( 'NONE', #18328, #29362, #10904, .T. ) ;
#43379 = CARTESIAN_POINT ( 'NONE',  ( 0.000000000000000000, 3.267716535433071279, 1.692913385826762873 ) ) ;
#43380 = ORIENTED_EDGE ( 'NONE', *, *, #50402, .F. ) ;
#43381 = ORIENTED_EDGE ( 'NONE', *, *, #27706, .F. ) ;
#43382 = AXIS2_PLACEMENT_3D ( 'NONE', #49533, #22225, #22722 ) ;
#43383 =( CONVERSION_BASED_UNIT ( 'INCH', #16029 ) LENGTH_UNIT ( ) NAMED_UNIT ( #11934 ) );
#43384 = VECTOR ( 'NONE', #46794, 39.37007874015748143 ) ;
#43385 = PLANE ( 'NONE',  #35853 ) ;
#43386 = VERTEX_POINT ( 'NONE', #26219 ) ;
#43387 = DIRECTION ( 'NONE',  ( 1.000000000000000000, 0.000000000000000000, 0.000000000000000000 ) ) ;
#43388 = VECTOR ( 'NONE', #39817, 39.37007874015748143 ) ;
#43389 = DIRECTION ( 'NONE',  ( -0.000000000000000000, 1.000000000000000000, -0.000000000000000000 ) ) ;
#43390 = VECTOR ( 'NONE', #2795, 39.37007874015748143 ) ;
#43391 = DIRECTION ( 'NONE',  ( 1.734723475976806848E-16, 0.000000000000000000, 1.000000000000000000 ) ) ;
#43392 = CARTESIAN_POINT ( 'NONE',  ( 1.472219874544873131, 1.742205712729733014, 2.560030851058970214 ) ) ;
#43393 = DIRECTION ( 'NONE',  ( 1.734723475976806848E-16, -0.000000000000000000, 1.000000000000000000 ) ) ;
#43394 = AXIS2_PLACEMENT_3D ( 'NONE', #24656, #9158, #13293 ) ;
#43395 = ORIENTED_EDGE ( 'NONE', *, *, #14707, .F. ) ;
#43396 = CARTESIAN_POINT ( 'NONE',  ( 1.909347346926324684, 0.000000000000000000, 0.4724409448818868706 ) ) ;
#43397 =( NAMED_UNIT ( * ) PLANE_ANGLE_UNIT ( ) SI_UNIT ( $, .RADIAN. ) );
#43398 = VERTEX_POINT ( 'NONE', #22350 ) ;
#43399 = VERTEX_POINT ( 'NONE', #29325 ) ;
#43400 = CARTESIAN_POINT ( 'NONE',  ( -1.628069513120385503, 0.001843152681973240061, -0.6423508795876955446 ) ) ;
#43401 = CARTESIAN_POINT ( 'NONE',  ( 0.000000000000000000, 3.267716535433071279, -0.3149606299212593941 ) ) ;
#43402 = DIRECTION ( 'NONE',  ( 1.000000000000000000, 0.000000000000000000, 0.000000000000000000 ) ) ;
#43403 = ORIENTED_EDGE ( 'NONE', *, *, #44934, .F. ) ;
#43404 = EDGE_CURVE ( 'NONE', #32825, #24862, #38106, .T. ) ;
#43405 = ORIENTED_EDGE ( 'NONE', *, *, #47556, .T. ) ;
#43406 = DIRECTION ( 'NONE',  ( -1.000000000000000000, -0.000000000000000000, -0.000000000000000000 ) ) ;
#43407 = ORIENTED_EDGE ( 'NONE', *, *, #7596, .F. ) ;
#43408 = CARTESIAN_POINT ( 'NONE',  ( 2.164658444855302122, 5.905511811023623991, -0.04795272066889885720 ) ) ;
#43409 = ADVANCED_FACE ( 'NONE', ( #39352 ), #103, .F. ) ;
#43410 = ORIENTED_EDGE ( 'NONE', *, *, #45397, .F. ) ;
#43411 = CARTESIAN_POINT ( 'NONE',  ( 2.576863348864710801, 1.456480680773285741, 1.442554885838449596 ) ) ;
#43412 = FACE_OUTER_BOUND ( 'NONE', #29031, .T. ) ;
#43413 = CARTESIAN_POINT ( 'NONE',  ( 0.000000000000000000, 0.000000000000000000, 2.952755905511811108 ) ) ;
#43414 = ADVANCED_FACE ( 'NONE', ( #7360 ), #46563, .T. ) ;
#43415 = EDGE_CURVE ( 'NONE', #44588, #23253, #7607, .T. ) ;
#43416 = CIRCLE ( 'NONE', #5481, 2.086614173228346303 ) ;
#43417 = VERTEX_POINT ( 'NONE', #26963 ) ;
#43418 = ORIENTED_EDGE ( 'NONE', *, *, #29880, .F. ) ;
#43419 = ORIENTED_EDGE ( 'NONE', *, *, #45465, .F. ) ;
#43420 = DIRECTION ( 'NONE',  ( -0.000000000000000000, 1.000000000000000000, -0.000000000000000000 ) ) ;
#43421 = AXIS2_PLACEMENT_3D ( 'NONE', #31218, #34588, #11588 ) ;
#43422 = DIRECTION ( 'NONE',  ( -0.9998717552508122886, -0.01601477604151180928, 0.000000000000000000 ) ) ;
#43423 = ORIENTED_EDGE ( 'NONE', *, *, #45422, .F. ) ;
#43424 = VERTEX_POINT ( 'NONE', #38355 ) ;
#43425 = EDGE_CURVE ( 'NONE', #47197, #35113, #11985, .T. ) ;
#43426 = CARTESIAN_POINT ( 'NONE',  ( -1.266385247993056185, 1.541563538762524166, -2.667452810599844071 ) ) ;
#43427 = CARTESIAN_POINT ( 'NONE',  ( 1.287906020515830141, 3.267716535433071279, -0.3149606299212596716 ) ) ;
#43428 = LINE ( 'NONE', #7817, #25286 ) ;
#43429 = VERTEX_POINT ( 'NONE', #27721 ) ;
#43430 = DIRECTION ( 'NONE',  ( -0.6234898018587431423, -1.160734090543304660E-16, 0.7818314824680221431 ) ) ;
#43431 = LINE ( 'NONE', #48039, #38974 ) ;
#43432 = AXIS2_PLACEMENT_3D ( 'NONE', #40033, #24023, #39260 ) ;
#43433 = DIRECTION ( 'NONE',  ( 0.000000000000000000, 0.000000000000000000, -1.000000000000000000 ) ) ;
#43434 = ORIENTED_EDGE ( 'NONE', *, *, #2252, .T. ) ;
#43435 = FACE_OUTER_BOUND ( 'NONE', #29623, .T. ) ;
#43436 = DIRECTION ( 'NONE',  ( -0.01601477604151182663, 0.9998717552508123996, -0.000000000000000000 ) ) ;
#43437 = ORIENTED_EDGE ( 'NONE', *, *, #32796, .T. ) ;
#43438 = CYLINDRICAL_SURFACE ( 'NONE', #20823, 2.165354330708661568 ) ;
#43439 = ORIENTED_EDGE ( 'NONE', *, *, #47070, .T. ) ;
#43440 = EDGE_LOOP ( 'NONE', ( #20039, #26251, #23104, #32885 ) ) ;
#43441 = DIRECTION ( 'NONE',  ( -0.01601477604151182663, 0.9998717552508123996, -0.000000000000000000 ) ) ;
#43442 = EDGE_CURVE ( 'NONE', #7243, #39002, #50412, .T. ) ;
#43443 = LINE ( 'NONE', #3456, #46149 ) ;
#43444 = CARTESIAN_POINT ( 'NONE',  ( -0.4788131938641533303, 1.525670379232220375, 2.914091152102185944 ) ) ;
#43445 = EDGE_CURVE ( 'NONE', #35577, #11067, #15101, .T. ) ;
#43446 = CARTESIAN_POINT ( 'NONE',  ( -0.8182917201112814842, 3.346456692913386100, 1.102362204724404160 ) ) ;
#43447 = EDGE_LOOP ( 'NONE', ( #3734, #16587, #12970, #15018 ) ) ;
#43448 = VERTEX_POINT ( 'NONE', #34980 ) ;
#43449 = ORIENTED_EDGE ( 'NONE', *, *, #28654, .F. ) ;
#43450 = DIRECTION ( 'NONE',  ( -3.469446951953613696E-16, 0.000000000000000000, -1.000000000000000000 ) ) ;
#43451 = FACE_OUTER_BOUND ( 'NONE', #39754, .T. ) ;
#43452 = CIRCLE ( 'NONE', #39338, 2.165354330708661568 ) ;
#43453 = VECTOR ( 'NONE', #16633, 39.37007874015748143 ) ;
#43454 = CARTESIAN_POINT ( 'NONE',  ( 0.5455278134075212115, 0.000000000000000000, 0.6299212598425161236 ) ) ;
#43455 = CARTESIAN_POINT ( 'NONE',  ( 0.2727639067037609943, 3.346456692913386100, 2.165354330708650910 ) ) ;
#43456 = VECTOR ( 'NONE', #37587, 39.37007874015748143 ) ;
#43457 = ORIENTED_EDGE ( 'NONE', *, *, #42057, .T. ) ;
#43458 = LINE ( 'NONE', #43967, #46442 ) ;
#43459 = LINE ( 'NONE', #44233, #38902 ) ;
#43460 = ORIENTED_EDGE ( 'NONE', *, *, #49947, .T. ) ;
#43461 = FACE_OUTER_BOUND ( 'NONE', #33766, .T. ) ;
#43462 = FACE_OUTER_BOUND ( 'NONE', #6689, .T. ) ;
#43463 = DIRECTION ( 'NONE',  ( 0.000000000000000000, 0.000000000000000000, -1.000000000000000000 ) ) ;
#43464 = ORIENTED_EDGE ( 'NONE', *, *, #36826, .T. ) ;
#43465 = CARTESIAN_POINT ( 'NONE',  ( -1.723188456408593527, 1.574803149606302854, 1.311251662046200694 ) ) ;
#43466 = DIRECTION ( 'NONE',  ( -0.000000000000000000, 1.000000000000000000, -0.000000000000000000 ) ) ;
#43467 = LINE ( 'NONE', #7863, #4456 ) ;
#43468 = ORIENTED_EDGE ( 'NONE', *, *, #31440, .F. ) ;
#43469 = FACE_OUTER_BOUND ( 'NONE', #3824, .T. ) ;
#43470 = CARTESIAN_POINT ( 'NONE',  ( -1.882988517681398966, 1.574803149606302854, 1.069164917025789530 ) ) ;
#43471 = EDGE_LOOP ( 'NONE', ( #22444, #8537, #5651, #26486, #10002, #2389 ) ) ;
#43472 = VECTOR ( 'NONE', #4228, 39.37007874015748143 ) ;
#43473 = B_SPLINE_CURVE_WITH_KNOTS ( 'NONE', 3,
 ( #44354, #40497, #4615, #20359 ),
 .UNSPECIFIED., .F., .F.,
 ( 4, 4 ),
 ( 0.001065024714398824521, 0.003565326717754890851 ),
 .UNSPECIFIED. ) ;
#43474 = DIRECTION ( 'NONE',  ( -1.000000000000000000, -0.000000000000000000, -0.000000000000000000 ) ) ;
#43475 = LINE ( 'NONE', #5017, #21865 ) ;
#43476 = LINE ( 'NONE', #47834, #19743 ) ;
#43477 = EDGE_CURVE ( 'NONE', #7931, #21785, #4717, .T. ) ;
#43478 = ADVANCED_FACE ( 'NONE', ( #2979 ), #3222, .F. ) ;
#43479 = EDGE_CURVE ( 'NONE', #1977, #30098, #34479, .T. ) ;
#43480 = ORIENTED_EDGE ( 'NONE', *, *, #37594, .F. ) ;
#43481 = ORIENTED_EDGE ( 'NONE', *, *, #34854, .F. ) ;
#43482 = CARTESIAN_POINT ( 'NONE',  ( -0.07591351300297277671, 0.000000000000000000, 1.417322834645662777 ) ) ;
#43483 = DIRECTION ( 'NONE',  ( 1.734723475976806848E-16, -0.000000000000000000, 1.000000000000000000 ) ) ;
#43484 = ORIENTED_EDGE ( 'NONE', *, *, #48714, .F. ) ;
#43485 = PLANE ( 'NONE',  #8544 ) ;
#43486 = DIRECTION ( 'NONE',  ( -0.5877852522924802425, 0.000000000000000000, 0.8090169943749422332 ) ) ;
#43487 = DIRECTION ( 'NONE',  ( -1.000000000000000000, 0.000000000000000000, 0.000000000000000000 ) ) ;
#43488 = DIRECTION ( 'NONE',  ( -6.104789737168038204E-17, 1.000000000000000000, -1.134460028949771622E-16 ) ) ;
#43489 = ORIENTED_EDGE ( 'NONE', *, *, #25927, .F. ) ;
#43490 = ORIENTED_EDGE ( 'NONE', *, *, #23509, .T. ) ;
#43491 = ORIENTED_EDGE ( 'NONE', *, *, #45620, .T. ) ;
#43492 = CARTESIAN_POINT ( 'NONE',  ( 1.687984952120845428, 3.346456692913386100, 1.259842519685033135 ) ) ;
#43493 = AXIS2_PLACEMENT_3D ( 'NONE', #42156, #45755, #26166 ) ;
#43494 = VECTOR ( 'NONE', #22230, 39.37007874015748143 ) ;
#43495 = DIRECTION ( 'NONE',  ( 1.734723475976806848E-16, 0.000000000000000000, 1.000000000000000000 ) ) ;
#43496 = DIRECTION ( 'NONE',  ( -3.469446951953613696E-16, 0.000000000000000000, -1.000000000000000000 ) ) ;
#43497 = FACE_BOUND ( 'NONE', #46779, .T. ) ;
#43498 = ORIENTED_EDGE ( 'NONE', *, *, #142, .T. ) ;
#43499 = CARTESIAN_POINT ( 'NONE',  ( 4.268512490100411402E-16, 3.346456692913386100, 1.889763779527550369 ) ) ;
#43500 = VERTEX_POINT ( 'NONE', #35484 ) ;
#43502 = ORIENTED_EDGE ( 'NONE', *, *, #36759, .F. ) ;
#43501 = AXIS2_PLACEMENT_3D ( 'NONE', #30501, #34381, #50071 ) ;
#43503 = ADVANCED_FACE ( 'NONE', ( #42714 ), #3210, .T. ) ;
#43504 = CARTESIAN_POINT ( 'NONE',  ( 2.138597145901430352, 2.755905511811027164, 0.3393547186367261159 ) ) ;
#43505 = EDGE_CURVE ( 'NONE', #18547, #37057, #22507, .T. ) ;
#43506 = ORIENTED_EDGE ( 'NONE', *, *, #8430, .T. ) ;
#43507 = VERTEX_POINT ( 'NONE', #3733 ) ;
#43508 = DIRECTION ( 'NONE',  ( 1.000000000000000000, 0.000000000000000000, -3.469446951953613696E-16 ) ) ;
#43509 = EDGE_CURVE ( 'NONE', #9779, #23437, #31107, .T. ) ;
#43510 = VECTOR ( 'NONE', #30193, 39.37007874015748143 ) ;
#43511 = VERTEX_POINT ( 'NONE', #11483 ) ;
#43512 = B_SPLINE_CURVE_WITH_KNOTS ( 'NONE', 3,
 ( #23813, #39561, #42911, #19921 ),
 .UNSPECIFIED., .F., .F.,
 ( 4, 4 ),
 ( 0.04164592054790196285, 0.04281073085324779703 ),
 .UNSPECIFIED. ) ;
#43513 = EDGE_CURVE ( 'NONE', #21641, #37337, #42955, .T. ) ;
#43515 = DIRECTION ( 'NONE',  ( 1.734723475976806848E-16, -0.000000000000000000, 1.000000000000000000 ) ) ;
#43514 = AXIS2_PLACEMENT_3D ( 'NONE', #18657, #11653, #50096 ) ;
#43516 = CARTESIAN_POINT ( 'NONE',  ( 0.2841802383804452603, 0.03247133209088205741, 1.841575167587790718 ) ) ;
#43517 = DIRECTION ( 'NONE',  ( -1.000000000000000000, 0.000000000000000000, 0.000000000000000000 ) ) ;
#43518 = CARTESIAN_POINT ( 'NONE',  ( -0.3486774197067339376, 3.346456692913386100, 2.077238655036873549 ) ) ;
#43519 = CARTESIAN_POINT ( 'NONE',  ( -0.5272349255865266260, 5.905511811023623991, 2.905303903342410621 ) ) ;
#43520 = CARTESIAN_POINT ( 'NONE',  ( 0.04921259842519669359, 1.643073385594818525, 2.245762300990225224 ) ) ;
#43521 = ORIENTED_EDGE ( 'NONE', *, *, #18967, .T. ) ;
#43522 = CARTESIAN_POINT ( 'NONE',  ( 1.295918523765950958, 1.485688605496056969, -2.653230334577374450 ) ) ;
#43523 = LINE ( 'NONE', #23919, #41682 ) ;
#43524 = CARTESIAN_POINT ( 'NONE',  ( 0.2727639067037604392, 0.000000000000000000, -0.6692913385826760875 ) ) ;
#43525 = VERTEX_POINT ( 'NONE', #35232 ) ;
#43526 = CARTESIAN_POINT ( 'NONE',  ( 0.8182917201112824834, 3.267716535433071279, 1.850393700787392293 ) ) ;
#43527 = CARTESIAN_POINT ( 'NONE',  ( 1.091055626815042645, 0.000000000000000000, 0.6299212598425161236 ) ) ;
#43528 = VERTEX_POINT ( 'NONE', #19466 ) ;
#43529 = CARTESIAN_POINT ( 'NONE',  ( -1.732283464566932052, 3.346456692913386100, -1.299212598425193210 ) ) ;
#43530 = AXIS2_PLACEMENT_3D ( 'NONE', #28175, #48981, #41532 ) ;
#43531 = CYLINDRICAL_SURFACE ( 'NONE', #18511, 0.8858267716535433989 ) ;
#43532 = DIRECTION ( 'NONE',  ( 0.000000000000000000, -0.000000000000000000, -1.000000000000000000 ) ) ;
#43533 = CIRCLE ( 'NONE', #693, 0.3740157480314960647 ) ;
#43534 = CARTESIAN_POINT ( 'NONE',  ( 2.141071258218635531, 0.000000000000000000, -0.04689341889560144638 ) ) ;
#43535 = ORIENTED_EDGE ( 'NONE', *, *, #6618, .T. ) ;
#43536 = PLANE ( 'NONE',  #27251 ) ;
#43537 = DIRECTION ( 'NONE',  ( -0.01601477604151182663, 0.9998717552508123996, -0.000000000000000000 ) ) ;
#43538 = VECTOR ( 'NONE', #39891, 39.37007874015748143 ) ;
#43539 = CIRCLE ( 'NONE', #21311, 2.165354330708661568 ) ;
#43540 = DIRECTION ( 'NONE',  ( -0.000000000000000000, 1.000000000000000000, -0.000000000000000000 ) ) ;
#43541 = DIRECTION ( 'NONE',  ( -0.000000000000000000, 1.000000000000000000, -0.000000000000000000 ) ) ;
#43542 = EDGE_LOOP ( 'NONE', ( #27764, #23536, #20813, #34084 ) ) ;
#43543 = AXIS2_PLACEMENT_3D ( 'NONE', #23962, #727, #47926 ) ;
#43544 = EDGE_CURVE ( 'NONE', #39002, #1584, #23598, .T. ) ;
#43545 = EDGE_LOOP ( 'NONE', ( #20696, #18312, #37167, #40409 ) ) ;
#43546 = ORIENTED_EDGE ( 'NONE', *, *, #20358, .F. ) ;
#43547 = EDGE_CURVE ( 'NONE', #17742, #3538, #29381, .T. ) ;
#43548 = DIRECTION ( 'NONE',  ( 0.000000000000000000, 0.000000000000000000, 1.000000000000000000 ) ) ;
#43549 = VERTEX_POINT ( 'NONE', #27466 ) ;
#43550 = CARTESIAN_POINT ( 'NONE',  ( 0.000000000000000000, 3.267716535433071279, -0.7874015748031473194 ) ) ;
#43551 = AXIS2_PLACEMENT_3D ( 'NONE', #21901, #37658, #26521 ) ;
#43552 = DIRECTION ( 'NONE',  ( -0.9998717552508121775, -0.01601477604151182663, 0.000000000000000000 ) ) ;
#43553 = ORIENTED_EDGE ( 'NONE', *, *, #44602, .F. ) ;
#43554 = EDGE_CURVE ( 'NONE', #13419, #34660, #16634, .T. ) ;
#43555 = CARTESIAN_POINT ( 'NONE',  ( -0.3937007874015748254, 0.3937007874015748254, -0.7480314960629921295 ) ) ;
#43556 = EDGE_LOOP ( 'NONE', ( #24205, #49864, #4511, #50534 ) ) ;
#43557 = CARTESIAN_POINT ( 'NONE',  ( 1.621795816027391979, 0.000000000000000000, -0.6396693727619211511 ) ) ;
#43558 = DIRECTION ( 'NONE',  ( 0.000000000000000000, 0.000000000000000000, 1.000000000000000000 ) ) ;
#43559 = ORIENTED_EDGE ( 'NONE', *, *, #48401, .F. ) ;
#43560 = CARTESIAN_POINT ( 'NONE',  ( -1.636583440222563635, 3.346456692913386100, 0.6299212598425164567 ) ) ;
#43561 = ORIENTED_EDGE ( 'NONE', *, *, #42333, .T. ) ;
#43562 = DIRECTION ( 'NONE',  ( -0.7071067811865466846, 0.000000000000000000, 0.7071067811865483499 ) ) ;
#43563 = EDGE_CURVE ( 'NONE', #5670, #39828, #40387, .T. ) ;
#43564 = VECTOR ( 'NONE', #41667, 39.37007874015748854 ) ;
#43565 = EDGE_LOOP ( 'NONE', ( #6580, #4400, #36142, #37691 ) ) ;
#43566 = VERTEX_POINT ( 'NONE', #4497 ) ;
#43567 = CARTESIAN_POINT ( 'NONE',  ( 0.000000000000000000, 2.755905511811023612, 0.000000000000000000 ) ) ;
#43568 = LINE ( 'NONE', #8472, #38593 ) ;
#43569 = EDGE_CURVE ( 'NONE', #48864, #31004, #24373, .T. ) ;
#43570 = ORIENTED_EDGE ( 'NONE', *, *, #38387, .T. ) ;
#43571 = AXIS2_PLACEMENT_3D ( 'NONE', #47445, #12374, #23733 ) ;
#43572 = FACE_OUTER_BOUND ( 'NONE', #50845, .T. ) ;
#43573 = VERTEX_POINT ( 'NONE', #31873 ) ;
#43574 = FACE_OUTER_BOUND ( 'NONE', #40866, .T. ) ;
#43575 = CARTESIAN_POINT ( 'NONE',  ( 0.000000000000000000, 3.267716535433071279, 0.000000000000000000 ) ) ;
#43576 = AXIS2_PLACEMENT_3D ( 'NONE', #8329, #31834, #27942 ) ;
#43577 = VECTOR ( 'NONE', #9408, 39.37007874015748143 ) ;
#43578 = LINE ( 'NONE', #5113, #8245 ) ;
#43579 = ORIENTED_EDGE ( 'NONE', *, *, #13771, .F. ) ;
#43580 = ORIENTED_EDGE ( 'NONE', *, *, #13076, .T. ) ;
#43581 = DIRECTION ( 'NONE',  ( 0.000000000000000000, 0.000000000000000000, 1.000000000000000000 ) ) ;
#43582 = CARTESIAN_POINT ( 'NONE',  ( 1.636583440222563857, 3.346456692913386100, 1.377952755905504256 ) ) ;
#43583 = LINE ( 'NONE', #38960, #48862 ) ;
#43584 = AXIS2_PLACEMENT_3D ( 'NONE', #36320, #40699, #37086 ) ;
#43585 = PLANE ( 'NONE',  #11154 ) ;
#43586 = LINE ( 'NONE', #24240, #42943 ) ;
#43587 = CYLINDRICAL_SURFACE ( 'NONE', #31762, 2.165354330708661568 ) ;
#43588 = ORIENTED_EDGE ( 'NONE', *, *, #48765, .F. ) ;
#43589 = DIRECTION ( 'NONE',  ( 1.734723475976806848E-16, -0.000000000000000000, 1.000000000000000000 ) ) ;
#43590 = EDGE_LOOP ( 'NONE', ( #28040, #47770, #47391, #49249 ) ) ;
#43591 = CARTESIAN_POINT ( 'NONE',  ( -0.3486774197067334380, 3.267716535433071279, 1.574803149606291974 ) ) ;
#43592 = ORIENTED_EDGE ( 'NONE', *, *, #25775, .T. ) ;
#43593 = CARTESIAN_POINT ( 'NONE',  ( -2.009899395340762229, 3.267716535433071279, -0.6299212598425177889 ) ) ;
#43594 = DIRECTION ( 'NONE',  ( -0.000000000000000000, 1.000000000000000000, -0.000000000000000000 ) ) ;
#43595 = CARTESIAN_POINT ( 'NONE',  ( 0.2239970000120027616, 0.000000000000000000, -1.939803615689571048 ) ) ;
#43596 = VECTOR ( 'NONE', #31564, 39.37007874015748143 ) ;
#43597 = ORIENTED_EDGE ( 'NONE', *, *, #3198, .F. ) ;
#43598 = EDGE_CURVE ( 'NONE', #2778, #40451, #32385, .T. ) ;
#43599 = CARTESIAN_POINT ( 'NONE',  ( -1.751183565233300543, 0.5249316475426857309, -0.6949723508179344034 ) ) ;
#43600 = EDGE_CURVE ( 'NONE', #46032, #14806, #10231, .T. ) ;
#43601 = ORIENTED_EDGE ( 'NONE', *, *, #14329, .F. ) ;
#43602 = DIRECTION ( 'NONE',  ( 1.000000000000000000, 0.000000000000000000, 0.000000000000000000 ) ) ;
#43603 = ORIENTED_EDGE ( 'NONE', *, *, #37705, .T. ) ;
#43604 = EDGE_CURVE ( 'NONE', #7678, #28374, #43973, .T. ) ;
#43605 = VECTOR ( 'NONE', #13538, 39.37007874015748143 ) ;
#43606 = PLANE ( 'NONE',  #15330 ) ;
#43607 = DIRECTION ( 'NONE',  ( -0.000000000000000000, 1.000000000000000000, -0.000000000000000000 ) ) ;
#43608 = EDGE_CURVE ( 'NONE', #8198, #33931, #12758, .T. ) ;
#43609 = ADVANCED_FACE ( 'NONE', ( #21012 ), #1385, .T. ) ;
#43610 = AXIS2_PLACEMENT_3D ( 'NONE', #8120, #11734, #39615 ) ;
#43611 = DIRECTION ( 'NONE',  ( 0.7227948638273978821, 0.000000000000000000, -0.6910626489868580968 ) ) ;
#43612 = ORIENTED_EDGE ( 'NONE', *, *, #38123, .T. ) ;
#43613 = EDGE_LOOP ( 'NONE', ( #43043, #21330, #22096, #24226 ) ) ;
#43614 = DIRECTION ( 'NONE',  ( -0.5877852522924684742, 9.392878985996986848E-17, -0.8090169943749506709 ) ) ;
#43615 = DIRECTION ( 'NONE',  ( 1.734723475976806848E-16, -0.000000000000000000, 1.000000000000000000 ) ) ;
#43616 = DIRECTION ( 'NONE',  ( -0.000000000000000000, -0.000000000000000000, 1.000000000000000000 ) ) ;
#43617 = CIRCLE ( 'NONE', #8187, 2.874015748031496731 ) ;
#43618 = EDGE_LOOP ( 'NONE', ( #45897, #9745, #26801, #3809 ) ) ;
#43619 = CARTESIAN_POINT ( 'NONE',  ( 1.558105373646058167, 3.267716535433071279, -1.417322834645665219 ) ) ;
#43620 = EDGE_CURVE ( 'NONE', #23414, #44911, #36763, .T. ) ;
#43621 = CARTESIAN_POINT ( 'NONE',  ( -2.009899395340762673, 3.346456692913386100, 0.6299212598425164567 ) ) ;
#43622 = ORIENTED_EDGE ( 'NONE', *, *, #28169, .F. ) ;
#43623 = CARTESIAN_POINT ( 'NONE',  ( -2.592410190554199634, 1.580416535242628928, 1.413664012880529119 ) ) ;
#43624 = EDGE_CURVE ( 'NONE', #40993, #16212, #16114, .T. ) ;
#43625 = EDGE_LOOP ( 'NONE', ( #16228, #5641, #7389, #28572 ) ) ;
#43626 = ORIENTED_EDGE ( 'NONE', *, *, #32954, .F. ) ;
#43627 = APPLICATION_PROTOCOL_DEFINITION ( 'draft international standard', 'automotive_design', 1998, #18712 ) ;
#43628 = ORIENTED_EDGE ( 'NONE', *, *, #23112, .F. ) ;
#43629 = LINE ( 'NONE', #25048, #4543 ) ;
#43630 = CARTESIAN_POINT ( 'NONE',  ( 0.000000000000000000, 3.267716535433071279, -1.889763779527552146 ) ) ;
#43631 = AXIS2_PLACEMENT_3D ( 'NONE', #20384, #36141, #12645 ) ;
#43632 = EDGE_CURVE ( 'NONE', #24862, #4018, #12493, .T. ) ;
#43633 = CARTESIAN_POINT ( 'NONE',  ( 0.2052282226254518727, 0.000000000000000000, -1.731265419273307682 ) ) ;
#43634 = DIRECTION ( 'NONE',  ( 0.000000000000000000, 1.000000000000000000, 0.000000000000000000 ) ) ;
#43635 = VERTEX_POINT ( 'NONE', #40632 ) ;
#43636 = ORIENTED_EDGE ( 'NONE', *, *, #17782, .T. ) ;
#43637 = CARTESIAN_POINT ( 'NONE',  ( -1.790827367621149024, 1.613601776126088128, -1.241082175747989735 ) ) ;
#43638 = CARTESIAN_POINT ( 'NONE',  ( -1.088998432874330735, 6.692913385826772199, 1.918626195649137500 ) ) ;
#43639 = VERTEX_POINT ( 'NONE', #17141 ) ;
#43640 = EDGE_CURVE ( 'NONE', #39372, #50839, #35996, .T. ) ;
#43641 = PLANE ( 'NONE',  #44899 ) ;
#43642 = CARTESIAN_POINT ( 'NONE',  ( 1.091055626815042423, 0.000000000000000000, -1.259842519685035134 ) ) ;
#43643 = VECTOR ( 'NONE', #18891, 39.37007874015748143 ) ;
#43644 = FACE_OUTER_BOUND ( 'NONE', #10305, .T. ) ;
#43645 = B_SPLINE_CURVE_WITH_KNOTS ( 'NONE', 3,
 ( #22043, #24895, #41161, #5270 ),
 .UNSPECIFIED., .F., .F.,
 ( 4, 4 ),
 ( 0.0001113516447889145337, 0.002611425118082581591 ),
 .UNSPECIFIED. ) ;
#43646 = CARTESIAN_POINT ( 'NONE',  ( -0.8942052331142552601, 3.346456692913386100, -1.972094414217999914 ) ) ;
#43647 = DIRECTION ( 'NONE',  ( 0.000000000000000000, -1.000000000000000000, 0.000000000000000000 ) ) ;
#43648 = ORIENTED_EDGE ( 'NONE', *, *, #1210, .T. ) ;
#43649 = LINE ( 'NONE', #31538, #15991 ) ;
#43650 = SURFACE_STYLE_USAGE ( .BOTH. , #27649 ) ;
#43651 = AXIS2_PLACEMENT_3D ( 'NONE', #10911, #23036, #3162 ) ;
#43652 = VERTEX_POINT ( 'NONE', #36508 ) ;
#43653 = VERTEX_POINT ( 'NONE', #12241 ) ;
#43654 = LINE ( 'NONE', #32063, #34829 ) ;
#43655 = FACE_OUTER_BOUND ( 'NONE', #34543, .T. ) ;
#43656 = DIRECTION ( 'NONE',  ( 1.000000000000000000, 0.000000000000000000, -3.469446951953613696E-16 ) ) ;
#43657 = ORIENTED_EDGE ( 'NONE', *, *, #23102, .T. ) ;
#43658 = ORIENTED_EDGE ( 'NONE', *, *, #27408, .F. ) ;
#43659 = CARTESIAN_POINT ( 'NONE',  ( 2.755905511811024056, 4.960629921259846142, -1.023622047244094224 ) ) ;
#43660 = VERTEX_POINT ( 'NONE', #43716 ) ;
#43661 = FACE_OUTER_BOUND ( 'NONE', #35211, .T. ) ;
#43662 = ORIENTED_EDGE ( 'NONE', *, *, #43710, .F. ) ;
#43663 = EDGE_CURVE ( 'NONE', #38821, #20664, #28488, .T. ) ;
#43664 = CARTESIAN_POINT ( 'NONE',  ( 2.280039352122881002, 0.9892193096974960520, 1.282827082053922485 ) ) ;
#43665 = DIRECTION ( 'NONE',  ( 1.734723475976806848E-16, -0.000000000000000000, 1.000000000000000000 ) ) ;
#43666 = DIRECTION ( 'NONE',  ( -1.000000000000000000, 0.000000000000000000, 0.000000000000000000 ) ) ;
#43667 = VECTOR ( 'NONE', #17678, 39.37007874015748143 ) ;
#43668 = EDGE_CURVE ( 'NONE', #2919, #23674, #4237, .T. ) ;
#43669 = EDGE_LOOP ( 'NONE', ( #46695, #24283, #34892 ) ) ;
#43670 = ORIENTED_EDGE ( 'NONE', *, *, #8449, .T. ) ;
#43671 = ORIENTED_EDGE ( 'NONE', *, *, #47232, .T. ) ;
#43672 = CARTESIAN_POINT ( 'NONE',  ( -1.117755760306016644, 0.3937007874015748254, -0.7480314960629922405 ) ) ;
#43673 = DIRECTION ( 'NONE',  ( -3.469446951953613696E-16, 0.000000000000000000, -1.000000000000000000 ) ) ;
#43674 = ORIENTED_EDGE ( 'NONE', *, *, #19758, .T. ) ;
#43675 = EDGE_LOOP ( 'NONE', ( #9775, #4706, #35101, #1235 ) ) ;
#43676 = LINE ( 'NONE', #44193, #43714 ) ;
#43677 = DIRECTION ( 'NONE',  ( -0.000000000000000000, 1.000000000000000000, -0.000000000000000000 ) ) ;
#43678 = DIRECTION ( 'NONE',  ( -3.469446951953613696E-16, 0.000000000000000000, -1.000000000000000000 ) ) ;
#43679 = ORIENTED_EDGE ( 'NONE', *, *, #45682, .T. ) ;
#43680 = LINE ( 'NONE', #49315, #9805 ) ;
#43681 = DIRECTION ( 'NONE',  ( -0.000000000000000000, 1.000000000000000000, -0.000000000000000000 ) ) ;
#43682 = CARTESIAN_POINT ( 'NONE',  ( -0.6214413264104945434, 0.000000000000000000, -0.7874015748031467643 ) ) ;
#43683 = EDGE_LOOP ( 'NONE', ( #22733, #44885, #47089, #20378 ) ) ;
#43684 = CARTESIAN_POINT ( 'NONE',  ( -1.636583440222564301, 0.000000000000000000, -0.6299212598425177889 ) ) ;
#43685 = CARTESIAN_POINT ( 'NONE',  ( 2.100190309385009169, 5.905511811023623991, 0.5298329251847516685 ) ) ;
#43686 = ORIENTED_EDGE ( 'NONE', *, *, #6585, .T. ) ;
#43687 = ORIENTED_EDGE ( 'NONE', *, *, #50874, .F. ) ;
#43688 = ORIENTED_EDGE ( 'NONE', *, *, #33141, .T. ) ;
#43689 = VECTOR ( 'NONE', #33925, 39.37007874015748143 ) ;
#43690 = CARTESIAN_POINT ( 'NONE',  ( -0.5455278134075214336, 3.346456692913386100, 0.1181102362204703021 ) ) ;
#43691 = CARTESIAN_POINT ( 'NONE',  ( -1.181102362204724310, 0.5905511811023621549, -1.181102362204724754 ) ) ;
#43692 = CARTESIAN_POINT ( 'NONE',  ( -1.198202975868765119, 3.346456692913386100, -1.732283464566922726 ) ) ;
#43693 = EDGE_CURVE ( 'NONE', #15979, #30087, #24632, .T. ) ;
#43694 = LINE ( 'NONE', #39588, #45090 ) ;
#43695 = LINE ( 'NONE', #5235, #34569 ) ;
#43696 = ORIENTED_EDGE ( 'NONE', *, *, #47296, .F. ) ;
#43697 = ORIENTED_EDGE ( 'NONE', *, *, #24280, .T. ) ;
#43698 = ORIENTED_EDGE ( 'NONE', *, *, #48831, .T. ) ;
#43699 = DIRECTION ( 'NONE',  ( 1.142080616180678453E-16, -1.000000000000000000, 2.072570748943325363E-17 ) ) ;
#43700 = EDGE_CURVE ( 'NONE', #25220, #21117, #24168, .T. ) ;
#43701 = DIRECTION ( 'NONE',  ( -0.000000000000000000, 1.000000000000000000, -0.000000000000000000 ) ) ;
#43702 = EDGE_CURVE ( 'NONE', #13031, #1905, #23859, .T. ) ;
#43703 = CARTESIAN_POINT ( 'NONE',  ( 1.091055626815043311, 0.000000000000000000, 1.574803149606291974 ) ) ;
#43704 = CARTESIAN_POINT ( 'NONE',  ( 0.002207914879453961535, -5.712274067634378313E-18, 0.04916304461325374242 ) ) ;
#43705 = CARTESIAN_POINT ( 'NONE',  ( -0.2042174104418111591, -0.6299212598425202314, -0.3133417129078099328 ) ) ;
#43706 = EDGE_LOOP ( 'NONE', ( #22235, #44043, #8141, #11659 ) ) ;
#43707 = DIRECTION ( 'NONE',  ( 0.01601477604151182663, -0.9998717552508123996, 0.000000000000000000 ) ) ;
#43708 = EDGE_CURVE ( 'NONE', #27397, #31869, #48837, .T. ) ;
#43709 = DIRECTION ( 'NONE',  ( -0.000000000000000000, 1.000000000000000000, -0.000000000000000000 ) ) ;
#43710 = EDGE_CURVE ( 'NONE', #22725, #24393, #30025, .T. ) ;
#43711 = AXIS2_PLACEMENT_3D ( 'NONE', #23518, #4164, #49651 ) ;
#43712 = ORIENTED_EDGE ( 'NONE', *, *, #27817, .T. ) ;
#43713 = CARTESIAN_POINT ( 'NONE',  ( -1.546800823997126262, 1.683127104815683728, -1.546979550173933182 ) ) ;
#43714 = VECTOR ( 'NONE', #13228, 39.37007874015748143 ) ;
#43715 = CARTESIAN_POINT ( 'NONE',  ( -0.8942052331142547050, 0.000000000000000000, 0.3149606299212580063 ) ) ;
#43716 = CARTESIAN_POINT ( 'NONE',  ( 2.378961647330872786, 3.267716535433071279, -0.1968503937007886062 ) ) ;
#43717 = ORIENTED_EDGE ( 'NONE', *, *, #11622, .T. ) ;
#43718 = CARTESIAN_POINT ( 'NONE',  ( 1.645338673473796254, 0.05427277550655955352, -1.027111169014480296 ) ) ;
#43719 = CARTESIAN_POINT ( 'NONE',  ( -1.350373579275921276, 0.006290961278228680842, 1.139832270491418553 ) ) ;
#43720 = DIRECTION ( 'NONE',  ( -1.000000000000000000, -0.000000000000000000, -0.000000000000000000 ) ) ;
#43721 = VERTEX_POINT ( 'NONE', #6544 ) ;
#43722 = FACE_BOUND ( 'NONE', #14996, .T. ) ;
#43723 = AXIS2_PLACEMENT_3D ( 'NONE', #22681, #6432, #49494 ) ;
#43724 = DIRECTION ( 'NONE',  ( -3.469446951953613696E-16, 0.000000000000000000, -1.000000000000000000 ) ) ;
#43725 = EDGE_LOOP ( 'NONE', ( #45940, #32415, #24800, #47585 ) ) ;
#43726 = PLANE ( 'NONE',  #8045 ) ;
#43727 = ADVANCED_FACE ( 'NONE', ( #29522 ), #37787, .F. ) ;
#43728 = PLANE ( 'NONE',  #13609 ) ;
#43729 = CARTESIAN_POINT ( 'NONE',  ( -1.876322193478733524, 1.681962395836037016, 1.559262294237737434 ) ) ;
#43730 = CARTESIAN_POINT ( 'NONE',  ( 0.000000000000000000, 0.000000000000000000, 0.000000000000000000 ) ) ;
#43731 = EDGE_CURVE ( 'NONE', #30180, #10179, #49093, .T. ) ;
#43732 = ADVANCED_FACE ( 'NONE', ( #37023 ), #27964, .F. ) ;
#43733 = ORIENTED_EDGE ( 'NONE', *, *, #11853, .T. ) ;
#43734 = ORIENTED_EDGE ( 'NONE', *, *, #44416, .F. ) ;
#43735 = LINE ( 'NONE', #43482, #33143 ) ;
#43736 = EDGE_CURVE ( 'NONE', #17239, #29386, #41151, .T. ) ;
#43737 = DIRECTION ( 'NONE',  ( -1.000000000000000000, 0.000000000000000000, -0.000000000000000000 ) ) ;
#43738 = ORIENTED_EDGE ( 'NONE', *, *, #548, .T. ) ;
#43739 = CARTESIAN_POINT ( 'NONE',  ( 0.1968503937007877735, 3.267716535433071279, 1.377952755905504256 ) ) ;
#43740 = DIRECTION ( 'NONE',  ( -3.469446951953613696E-16, 0.000000000000000000, -1.000000000000000000 ) ) ;
#43741 = DIRECTION ( 'NONE',  ( -0.1342332658176522420, -1.160734090543305153E-16, -0.9909497617679352555 ) ) ;
#43742 = DIRECTION ( 'NONE',  ( -0.3090169943749582204, -1.160734090543304660E-16, 0.9510565162951500895 ) ) ;
#43743 = ORIENTED_EDGE ( 'NONE', *, *, #39968, .T. ) ;
#43744 = ORIENTED_EDGE ( 'NONE', *, *, #46447, .F. ) ;
#43745 = FACE_OUTER_BOUND ( 'NONE', #50456, .T. ) ;
#43746 = DIRECTION ( 'NONE',  ( 0.000000000000000000, 0.000000000000000000, -1.000000000000000000 ) ) ;
#43747 = CARTESIAN_POINT ( 'NONE',  ( 0.5455278134075212115, 0.000000000000000000, -0.9448818897637765168 ) ) ;
#43748 = CARTESIAN_POINT ( 'NONE',  ( 2.043634885149959057, 6.692913385826772199, 0.7157624142946238388 ) ) ;
#43749 = FACE_BOUND ( 'NONE', #21709, .T. ) ;
#43750 = EDGE_LOOP ( 'NONE', ( #10983, #3566, #43984, #42339 ) ) ;
#43751 = CARTESIAN_POINT ( 'NONE',  ( 1.909347346926324684, 3.346456692913386100, -0.1574803149606304187 ) ) ;
#43752 = ORIENTED_EDGE ( 'NONE', *, *, #13774, .F. ) ;
#43753 = ORIENTED_EDGE ( 'NONE', *, *, #14673, .T. ) ;
#43754 = CARTESIAN_POINT ( 'NONE',  ( -1.971834065208965203, 0.000000000000000000, 0.8963217522329899323 ) ) ;
#43755 = AXIS2_PLACEMENT_3D ( 'NONE', #45105, #1507, #5883 ) ;
#43756 = VECTOR ( 'NONE', #6746, 39.37007874015748854 ) ;
#43757 = ORIENTED_EDGE ( 'NONE', *, *, #41255, .T. ) ;
#43759 = ORIENTED_EDGE ( 'NONE', *, *, #15867, .F. ) ;
#43758 = ADVANCED_FACE ( 'NONE', ( #45492 ), #26154, .F. ) ;
#43760 = CARTESIAN_POINT ( 'NONE',  ( 0.1155636338427008941, -0.5222242541845523167, 0.000000000000000000 ) ) ;
#43761 = ORIENTED_EDGE ( 'NONE', *, *, #41479, .F. ) ;
#43762 = AXIS2_PLACEMENT_3D ( 'NONE', #40720, #1725, #5347 ) ;
#43763 = DIRECTION ( 'NONE',  ( -0.6427876096865403621, -0.7660444431189770143, 0.000000000000000000 ) ) ;
#43764 = FACE_OUTER_BOUND ( 'NONE', #27801, .T. ) ;
#43765 = EDGE_CURVE ( 'NONE', #38732, #3406, #13776, .T. ) ;
#43766 = LINE ( 'NONE', #39402, #18502 ) ;
#43767 = ADVANCED_FACE ( 'NONE', ( #1638 ), #33663, .F. ) ;
#43768 = EDGE_CURVE ( 'NONE', #42606, #27951, #43617, .T. ) ;
#43769 = FACE_OUTER_BOUND ( 'NONE', #6834, .T. ) ;
#43770 = EDGE_CURVE ( 'NONE', #20204, #12025, #21388, .T. ) ;
#43771 = LINE ( 'NONE', #4550, #10502 ) ;
#43772 = CARTESIAN_POINT ( 'NONE',  ( -1.152568299495734250, 1.574803149606302854, 1.833124570921536467 ) ) ;
#43773 = ORIENTED_EDGE ( 'NONE', *, *, #45532, .F. ) ;
#43774 = CARTESIAN_POINT ( 'NONE',  ( 0.002207914879453961535, -5.712274067634378313E-18, 0.04916304461325374242 ) ) ;
#43775 = CARTESIAN_POINT ( 'NONE',  ( 1.695772546416037363, 1.745688802946234297, -2.417756147381349141 ) ) ;
#43776 = CARTESIAN_POINT ( 'NONE',  ( 0.4696143004045479352, 3.346456692913386100, -0.4724409448818886470 ) ) ;
#43777 = ORIENTED_EDGE ( 'NONE', *, *, #761, .T. ) ;
#43778 = LINE ( 'NONE', #938, #17443 ) ;
#43779 = CARTESIAN_POINT ( 'NONE',  ( -0.8182917201112819283, 3.267716535433071279, -1.929133858267710000 ) ) ;
#43780 = VERTEX_POINT ( 'NONE', #21775 ) ;
#43781 = CARTESIAN_POINT ( 'NONE',  ( 0.000000000000000000, 0.000000000000000000, -1.968503937007874072 ) ) ;
#43782 = CARTESIAN_POINT ( 'NONE',  ( 1.973323729629757217, 0.000000000000000000, -0.7899196136953162695 ) ) ;
#43783 = CARTESIAN_POINT ( 'NONE',  ( 0.4696143004045484348, 0.000000000000000000, 1.220472440944875281 ) ) ;
#43784 = PRODUCT ( 'Stator', 'Stator', '', ( #39513 ) ) ;
#43785 = CYLINDRICAL_SURFACE ( 'NONE', #32330, 2.086614173228346303 ) ;
#43786 = ADVANCED_FACE ( 'NONE', ( #34164 ), #17900, .F. ) ;
#43787 = VECTOR ( 'NONE', #11577, 39.37007874015748143 ) ;
#43788 = EDGE_LOOP ( 'NONE', ( #47174, #48678, #9463, #25387 ) ) ;
#43789 = CARTESIAN_POINT ( 'NONE',  ( -0.2922638600240530793, 1.612444929547712125, -2.698310553500231634 ) ) ;
#43790 = DIRECTION ( 'NONE',  ( 0.8805955318567321166, 0.000000000000000000, 0.4738686624730094055 ) ) ;
#43791 = VECTOR ( 'NONE', #42950, 39.37007874015748854 ) ;
#43792 = ADVANCED_FACE ( 'NONE', ( #14277 ), #34542, .T. ) ;
#43793 = VECTOR ( 'NONE', #30315, 39.37007874015748143 ) ;
#43794 = CARTESIAN_POINT ( 'NONE',  ( -1.979793062125317693, 1.688404340953838068, 2.191257344206539504 ) ) ;
#43795 = CARTESIAN_POINT ( 'NONE',  ( -2.182111253630085734, 3.346456692913386100, -0.8267716535433052849 ) ) ;
#43796 = ADVANCED_FACE ( 'NONE', ( #29774 ), #10151, .F. ) ;
#43797 = VECTOR ( 'NONE', #29279, 39.37007874015748143 ) ;
#43798 = VERTEX_POINT ( 'NONE', #14537 ) ;
#43799 = VERTEX_POINT ( 'NONE', #18156 ) ;
#43800 = EDGE_CURVE ( 'NONE', #50716, #17666, #37278, .T. ) ;
#43801 = DIRECTION ( 'NONE',  ( 1.000000000000000000, 0.000000000000000000, 0.000000000000000000 ) ) ;
#43802 = EDGE_CURVE ( 'NONE', #47200, #32548, #17645, .T. ) ;
#43803 = ORIENTED_EDGE ( 'NONE', *, *, #20548, .F. ) ;
#43804 = VECTOR ( 'NONE', #8775, 39.37007874015748143 ) ;
#43805 = DIRECTION ( 'NONE',  ( 0.04486483035051863633, -1.160734090543304660E-16, -0.9989930665413144784 ) ) ;
#43806 = ORIENTED_EDGE ( 'NONE', *, *, #44435, .F. ) ;
#43807 = CARTESIAN_POINT ( 'NONE',  ( 1.015142113812069313, 0.000000000000000000, 1.102362204724403938 ) ) ;
#43808 = AXIS2_PLACEMENT_3D ( 'NONE', #10217, #33215, #20815 ) ;
#43809 = B_SPLINE_CURVE_WITH_KNOTS ( 'NONE', 3,
 ( #25648, #17147, #5264, #24891 ),
 .UNSPECIFIED., .F., .F.,
 ( 4, 4 ),
 ( 2.137550060313775870E-07, 0.002500695496946613028 ),
 .UNSPECIFIED. ) ;
#43810 = ORIENTED_EDGE ( 'NONE', *, *, #44695, .T. ) ;
#43811 = CARTESIAN_POINT ( 'NONE',  ( -1.091055626815042645, 3.346456692913386100, -1.259842519685034690 ) ) ;
#43812 = ORIENTED_EDGE ( 'NONE', *, *, #8355, .F. ) ;
#43813 = FACE_OUTER_BOUND ( 'NONE', #773, .T. ) ;
#43814 = ORIENTED_EDGE ( 'NONE', *, *, #19262, .T. ) ;
#43815 = CARTESIAN_POINT ( 'NONE',  ( 1.636583440222563857, 3.346456692913386100, -0.3149606299212596716 ) ) ;
#43816 = VERTEX_POINT ( 'NONE', #19153 ) ;
#43817 = ORIENTED_EDGE ( 'NONE', *, *, #14540, .T. ) ;
#43818 = LINE ( 'NONE', #8469, #30618 ) ;
#43819 = CARTESIAN_POINT ( 'NONE',  ( -0.04921259842519707522, 1.574803149606302854, 2.164795024401847456 ) ) ;
#43820 = EDGE_LOOP ( 'NONE', ( #50766, #17657, #47990, #27827 ) ) ;
#43821 = DIRECTION ( 'NONE',  ( -1.000000000000000000, -0.000000000000000000, -0.000000000000000000 ) ) ;
#43822 = ORIENTED_EDGE ( 'NONE', *, *, #33761, .T. ) ;
#43823 = CARTESIAN_POINT ( 'NONE',  ( 2.576863348864710801, 1.660943078747768364, 1.442554885838449819 ) ) ;
#43824 = AXIS2_PLACEMENT_3D ( 'NONE', #35991, #16109, #28484 ) ;
#43825 = CARTESIAN_POINT ( 'NONE',  ( 0.002207914879453961535, -5.712274067634378313E-18, 0.04916304461325374242 ) ) ;
#43826 = VECTOR ( 'NONE', #7264, 39.37007874015748143 ) ;
#43827 = EDGE_CURVE ( 'NONE', #34736, #30054, #46497, .T. ) ;
#43828 = LINE ( 'NONE', #48188, #30512 ) ;
#43829 = ORIENTED_EDGE ( 'NONE', *, *, #34783, .F. ) ;
#43830 = ORIENTED_EDGE ( 'NONE', *, *, #7438, .F. ) ;
#43831 = EDGE_CURVE ( 'NONE', #35502, #5108, #42394, .T. ) ;
#43832 = AXIS2_PLACEMENT_3D ( 'NONE', #47518, #3942, #19415 ) ;
#43833 = CARTESIAN_POINT ( 'NONE',  ( -2.258024766633058622, 3.346456692913386100, 0.1574803149606286423 ) ) ;
#43834 = CARTESIAN_POINT ( 'NONE',  ( -1.909347346926324462, 3.267716535433071279, -0.1574803149606297248 ) ) ;
#43835 = EDGE_CURVE ( 'NONE', #17350, #41720, #30786, .T. ) ;
#43836 = CARTESIAN_POINT ( 'NONE',  ( 1.692294915983738157, 1.738507761360482018, 1.862189238238326050 ) ) ;
#43837 = VECTOR ( 'NONE', #971, 39.37007874015748143 ) ;
#43838 = CARTESIAN_POINT ( 'NONE',  ( 1.041962601392105725, 0.02949362477880272670, 1.648001814300100065 ) ) ;
#43839 = LINE ( 'NONE', #8490, #46212 ) ;
#43840 = AXIS2_PLACEMENT_3D ( 'NONE', #34476, #10971, #11228 ) ;
#43841 = CARTESIAN_POINT ( 'NONE',  ( 2.277873973731426194, 0.000000000000000000, 1.879489153247667854 ) ) ;
#43842 = VERTEX_POINT ( 'NONE', #19398 ) ;
#43843 = FACE_OUTER_BOUND ( 'NONE', #3940, .T. ) ;
#43844 = ORIENTED_EDGE ( 'NONE', *, *, #29760, .F. ) ;
#43845 = CARTESIAN_POINT ( 'NONE',  ( -1.985260859929297572, 3.346456692913386100, 0.9448818897637749625 ) ) ;
#43846 = EDGE_CURVE ( 'NONE', #34884, #47219, #46250, .T. ) ;
#43847 = EDGE_LOOP ( 'NONE', ( #11312, #48857, #47024, #49505 ) ) ;
#43848 = PLANE ( 'NONE',  #1131 ) ;
#43849 = CARTESIAN_POINT ( 'NONE',  ( -1.636583440222564301, 0.000000000000000000, -0.3149606299212592275 ) ) ;
#43850 = EDGE_CURVE ( 'NONE', #30308, #20408, #34413, .T. ) ;
#43851 = CARTESIAN_POINT ( 'NONE',  ( -1.712496953225537188, 3.267716535433071279, -0.03937007874015881204 ) ) ;
#43852 = ORIENTED_EDGE ( 'NONE', *, *, #49452, .T. ) ;
#43853 = LINE ( 'NONE', #40001, #46364 ) ;
#43854 = FACE_OUTER_BOUND ( 'NONE', #30953, .T. ) ;
#43855 = EDGE_CURVE ( 'NONE', #16487, #2592, #11468, .T. ) ;
#43856 = ORIENTED_EDGE ( 'NONE', *, *, #14323, .T. ) ;
#43857 = CARTESIAN_POINT ( 'NONE',  ( -1.091055626815042201, 0.000000000000000000, 0.9448818897637749625 ) ) ;
#43858 = EDGE_CURVE ( 'NONE', #47575, #34814, #15290, .T. ) ;
#43859 = ORIENTED_EDGE ( 'NONE', *, *, #19270, .T. ) ;
#43860 = CARTESIAN_POINT ( 'NONE',  ( 1.588513588560381828, 0.05336261777518135074, -1.107536019441389019 ) ) ;
#43861 = LINE ( 'NONE', #15239, #32188 ) ;
#43862 = AXIS2_PLACEMENT_3D ( 'NONE', #42118, #41116, #17867 ) ;
#43863 = AXIS2_PLACEMENT_3D ( 'NONE', #49615, #7561, #33929 ) ;
#43864 = LINE ( 'NONE', #48730, #22251 ) ;
#43865 = ORIENTED_EDGE ( 'NONE', *, *, #15737, .F. ) ;
#43866 = ORIENTED_EDGE ( 'NONE', *, *, #21705, .T. ) ;
#43867 = CARTESIAN_POINT ( 'NONE',  ( -2.100227814008681637, 1.686526752338742385, -2.076109931251943763 ) ) ;
#43869 = LINE ( 'NONE', #8519, #29780 ) ;
#43868 = VECTOR ( 'NONE', #48625, 39.37007874015748143 ) ;
#43870 = DIRECTION ( 'NONE',  ( 1.734723475976806848E-16, 0.000000000000000000, 1.000000000000000000 ) ) ;
#43871 = VECTOR ( 'NONE', #19653, 39.37007874015748143 ) ;
#43872 = LINE ( 'NONE', #39507, #3122 ) ;
#43873 = DIRECTION ( 'NONE',  ( 0.9959742939952384022, 0.000000000000000000, 0.08963930890344089242 ) ) ;
#43874 = ORIENTED_EDGE ( 'NONE', *, *, #12847, .F. ) ;
#43875 = DIRECTION ( 'NONE',  ( -0.000000000000000000, 1.000000000000000000, -0.000000000000000000 ) ) ;
#43876 = VERTEX_POINT ( 'NONE', #50104 ) ;
#43877 = ORIENTED_EDGE ( 'NONE', *, *, #7097, .F. ) ;
#43878 = CONTEXT_DEPENDENT_SHAPE_REPRESENTATION ( #13428, #23585 ) ;
#43879 = ORIENTED_EDGE ( 'NONE', *, *, #28489, .F. ) ;
#43880 = CARTESIAN_POINT ( 'NONE',  ( 0.000000000000000000, 7.874015748031496287, 0.000000000000000000 ) ) ;
#43881 = CARTESIAN_POINT ( 'NONE',  ( 2.182111253630085290, 0.000000000000000000, -0.3149606299212596716 ) ) ;
#43882 = DIRECTION ( 'NONE',  ( 1.734723475976806848E-16, 0.000000000000000000, 1.000000000000000000 ) ) ;
#43883 = CARTESIAN_POINT ( 'NONE',  ( -1.439733046521776583, 3.267716535433071279, -0.9448818897637762948 ) ) ;
#43884 = EDGE_LOOP ( 'NONE', ( #8189, #40505, #23900, #13014 ) ) ;
#43885 = ORIENTED_EDGE ( 'NONE', *, *, #437, .T. ) ;
#43886 = EDGE_CURVE ( 'NONE', #49800, #46986, #4097, .T. ) ;
#43887 = CARTESIAN_POINT ( 'NONE',  ( 1.091055626815043311, 0.000000000000000000, 1.889763779527550369 ) ) ;
#43888 = DIRECTION ( 'NONE',  ( -0.000000000000000000, 1.000000000000000000, -0.000000000000000000 ) ) ;
#43889 = EDGE_CURVE ( 'NONE', #20960, #39237, #29640, .T. ) ;
#43890 = LINE ( 'NONE', #40556, #12641 ) ;
#43891 = ORIENTED_EDGE ( 'NONE', *, *, #12475, .F. ) ;
#43892 = EDGE_CURVE ( 'NONE', #15727, #2869, #14791, .T. ) ;
#43893 = DIRECTION ( 'NONE',  ( -1.000000000000000000, -0.000000000000000000, -0.000000000000000000 ) ) ;
#43894 = EDGE_CURVE ( 'NONE', #49655, #34486, #47716, .T. ) ;
#43895 = CARTESIAN_POINT ( 'NONE',  ( -1.363819533518803473, 0.000000000000000000, 2.047244094488179567 ) ) ;
#43896 = VECTOR ( 'NONE', #43875, 39.37007874015748143 ) ;
#43897 = LINE ( 'NONE', #8548, #33408 ) ;
#43898 = ADVANCED_FACE ( 'NONE', ( #43144 ), #46003, .F. ) ;
#43899 = CARTESIAN_POINT ( 'NONE',  ( -0.6214413264104945434, 0.000000000000000000, -1.417322834645664331 ) ) ;
#43900 = FACE_OUTER_BOUND ( 'NONE', #49350, .T. ) ;
#43901 = VECTOR ( 'NONE', #19242, 39.37007874015748143 ) ;
#43902 = ORIENTED_EDGE ( 'NONE', *, *, #29358, .F. ) ;
#43903 = LINE ( 'NONE', #31289, #50539 ) ;
#43904 = DIRECTION ( 'NONE',  ( -0.000000000000000000, 1.000000000000000000, -0.000000000000000000 ) ) ;
#43905 = VECTOR ( 'NONE', #21405, 39.37007874015748143 ) ;
#43906 = ORIENTED_EDGE ( 'NONE', *, *, #34094, .T. ) ;
#43907 = VECTOR ( 'NONE', #36748, 39.37007874015748854 ) ;
#43908 = ORIENTED_EDGE ( 'NONE', *, *, #41641, .F. ) ;
#43909 = FACE_OUTER_BOUND ( 'NONE', #21180, .T. ) ;
#43910 = DIRECTION ( 'NONE',  ( -0.000000000000000000, 1.000000000000000000, -0.000000000000000000 ) ) ;
#43911 = EDGE_CURVE ( 'NONE', #35300, #49387, #28686, .T. ) ;
#43912 = LINE ( 'NONE', #8560, #33780 ) ;
#43913 = ORIENTED_EDGE ( 'NONE', *, *, #34296, .T. ) ;
#43914 = VECTOR ( 'NONE', #49155, 39.37007874015748143 ) ;
#43915 = EDGE_CURVE ( 'NONE', #37948, #44472, #20850, .T. ) ;
#43916 = ORIENTED_EDGE ( 'NONE', *, *, #14637, .F. ) ;
#43917 = PLANE ( 'NONE',  #45999 ) ;
#43918 = ORIENTED_EDGE ( 'NONE', *, *, #45306, .F. ) ;
#43919 = B_SPLINE_CURVE_WITH_KNOTS ( 'NONE', 3,
 ( #48832, #9643, #41146, #17640 ),
 .UNSPECIFIED., .F., .F.,
 ( 4, 4 ),
 ( 2.008334167098713497E-07, 0.002500501959281965520 ),
 .UNSPECIFIED. ) ;
#43920 = PLANE ( 'NONE',  #43530 ) ;
#43921 = ORIENTED_EDGE ( 'NONE', *, *, #1766, .F. ) ;
#43922 = CARTESIAN_POINT ( 'NONE',  ( 0.6502734851936936566, 1.718317270777941941, -2.171228911417812046 ) ) ;
#43923 = CARTESIAN_POINT ( 'NONE',  ( 0.5762653268100312864, 0.000000000000000000, -1.903066372058335620 ) ) ;
#43924 = LINE ( 'NONE', #48025, #5423 ) ;
#43925 = VERTEX_POINT ( 'NONE', #15039 ) ;
#43926 = ORIENTED_EDGE ( 'NONE', *, *, #15299, .T. ) ;
#43927 = ORIENTED_EDGE ( 'NONE', *, *, #978, .T. ) ;
#43928 = CARTESIAN_POINT ( 'NONE',  ( -0.3486774197067339376, 3.346456692913386100, -1.259842519685035134 ) ) ;
#43929 = VERTEX_POINT ( 'NONE', #26401 ) ;
#43930 = VERTEX_POINT ( 'NONE', #7295 ) ;
#43931 = PLANE ( 'NONE',  #25641 ) ;
#43932 = CARTESIAN_POINT ( 'NONE',  ( 0.000000000000000000, 3.267716535433071279, 1.102362204724404160 ) ) ;
#43933 = LINE ( 'NONE', #8580, #5420 ) ;
#43934 = ADVANCED_FACE ( 'NONE', ( #3416 ), #50592, .T. ) ;
#43935 = VERTEX_POINT ( 'NONE', #31297 ) ;
#43936 = CARTESIAN_POINT ( 'NONE',  ( 0.5455278134075217666, 3.346456692913386100, 1.574803149606291974 ) ) ;
#43937 = LINE ( 'NONE', #843, #6001 ) ;
#43938 = DIRECTION ( 'NONE',  ( -0.000000000000000000, 1.000000000000000000, -0.000000000000000000 ) ) ;
#43939 = ORIENTED_EDGE ( 'NONE', *, *, #40002, .F. ) ;
#43940 = CARTESIAN_POINT ( 'NONE',  ( 0.5662636741187413447, 0.000000000000000000, 1.648861433446464186 ) ) ;
#43941 = VECTOR ( 'NONE', #26680, 39.37007874015748143 ) ;
#43942 = CARTESIAN_POINT ( 'NONE',  ( -0.3486774197067339376, 3.346456692913386100, -0.6299212598425175669 ) ) ;
#43943 = ORIENTED_EDGE ( 'NONE', *, *, #38493, .F. ) ;
#43944 = CARTESIAN_POINT ( 'NONE',  ( -1.363819533518803473, 3.346456692913386100, 1.681890501046756192 ) ) ;
#43945 = ORIENTED_EDGE ( 'NONE', *, *, #29953, .T. ) ;
#43946 = VERTEX_POINT ( 'NONE', #35423 ) ;
#43947 = CARTESIAN_POINT ( 'NONE',  ( -2.099568260077699033, 6.692913385826772199, -0.5296909464896106812 ) ) ;
#43948 = VECTOR ( 'NONE', #19375, 39.37007874015748143 ) ;
#43949 = VECTOR ( 'NONE', #21959, 39.37007874015748143 ) ;
#43950 = DIRECTION ( 'NONE',  ( -1.000000000000000000, 0.000000000000000000, 0.000000000000000000 ) ) ;
#43951 = CARTESIAN_POINT ( 'NONE',  ( -0.6214413264104945434, 0.000000000000000000, -0.3543307086614175816 ) ) ;
#43952 = CARTESIAN_POINT ( 'NONE',  ( -1.642191404871911731, 0.000000000000000000, 0.5853255206279681655 ) ) ;
#43953 = VERTEX_POINT ( 'NONE', #6788 ) ;
#43954 = VERTEX_POINT ( 'NONE', #38295 ) ;
#43955 = VECTOR ( 'NONE', #27972, 39.37007874015748143 ) ;
#43956 = EDGE_CURVE ( 'NONE', #24752, #28976, #35674, .T. ) ;
#43957 = ORIENTED_EDGE ( 'NONE', *, *, #38179, .F. ) ;
#43958 = CARTESIAN_POINT ( 'NONE',  ( 2.308557526972506047, 5.905511811023623991, 1.841013194464793390 ) ) ;
#43959 = CARTESIAN_POINT ( 'NONE',  ( 0.000000000000000000, 3.267716535433071279, 2.007874015748021268 ) ) ;
#43960 = EDGE_CURVE ( 'NONE', #11828, #5323, #47503, .T. ) ;
#43961 = ADVANCED_FACE ( 'NONE', ( #8814 ), #24050, .F. ) ;
#43962 = ADVANCED_FACE ( 'NONE', ( #31806 ), #32320, .F. ) ;
#43963 = DIRECTION ( 'NONE',  ( -1.000000000000000000, 0.000000000000000000, 0.000000000000000000 ) ) ;
#43964 = LINE ( 'NONE', #20487, #27686 ) ;
#43965 = LINE ( 'NONE', #43455, #42709 ) ;
#43966 = ORIENTED_EDGE ( 'NONE', *, *, #12757, .F. ) ;
#43967 = CARTESIAN_POINT ( 'NONE',  ( 3.937007874015748143, 5.118110236220475784, 1.181102362204724310 ) ) ;
#43968 = PLANE ( 'NONE',  #28161 ) ;
#43969 = ORIENTED_EDGE ( 'NONE', *, *, #6845, .F. ) ;
#43970 = DIRECTION ( 'NONE',  ( -0.000000000000000000, 0.000000000000000000, 1.000000000000000000 ) ) ;
#43971 = CARTESIAN_POINT ( 'NONE',  ( 2.662626360126375769, 1.757290156728792185, -0.6582052835281975156 ) ) ;
#43972 = EDGE_CURVE ( 'NONE', #21553, #10178, #32116, .T. ) ;
#43973 = LINE ( 'NONE', #16377, #1588 ) ;
#43974 = ORIENTED_EDGE ( 'NONE', *, *, #1597, .T. ) ;
#43975 = DIRECTION ( 'NONE',  ( -1.000000000000000000, 0.000000000000000000, 0.000000000000000000 ) ) ;
#43976 = CARTESIAN_POINT ( 'NONE',  ( -0.3129956986278690789, 1.049866565067837820, 2.000361441164483445 ) ) ;
#43977 = CARTESIAN_POINT ( 'NONE',  ( -1.602125192864240821, 3.346456692913386100, -1.456692913385822186 ) ) ;
#43978 = AXIS2_PLACEMENT_3D ( 'NONE', #44699, #18119, #48800 ) ;
#43979 = EDGE_CURVE ( 'NONE', #30012, #41869, #12691, .T. ) ;
#43980 = VERTEX_POINT ( 'NONE', #48013 ) ;
#43981 = AXIS2_PLACEMENT_3D ( 'NONE', #28105, #27596, #4120 ) ;
#43982 = DIRECTION ( 'NONE',  ( -0.000000000000000000, 1.000000000000000000, -0.000000000000000000 ) ) ;
#43983 = DIRECTION ( 'NONE',  ( -0.000000000000000000, 1.000000000000000000, -0.000000000000000000 ) ) ;
#43984 = ORIENTED_EDGE ( 'NONE', *, *, #7425, .T. ) ;
#43985 = CARTESIAN_POINT ( 'NONE',  ( 4.821444091131312140E-17, 0.07874015748031502893, 0.3937007874015748254 ) ) ;
#43986 = ADVANCED_BREP_SHAPE_REPRESENTATION ( '', ( #23876, #26741 ), #4483 ) ;
#43987 = AXIS2_PLACEMENT_3D ( 'NONE', #25886, #18144, #49836 ) ;
#43988 = B_SPLINE_CURVE_WITH_KNOTS ( 'NONE', 3,
 ( #7669, #7921, #23926, #39672 ),
 .UNSPECIFIED., .F., .F.,
 ( 4, 4 ),
 ( 2.051202603109093890E-07, 0.002500241469102131974 ),
 .UNSPECIFIED. ) ;
#43989 = CARTESIAN_POINT ( 'NONE',  ( -0.5455278134075214336, 3.267716535433071279, -1.889763779527552146 ) ) ;
#43990 = LINE ( 'NONE', #38678, #11504 ) ;
#43991 = CARTESIAN_POINT ( 'NONE',  ( 0.2431224069212730987, 5.905511811023623991, 2.152304290637673478 ) ) ;
#43992 = EDGE_CURVE ( 'NONE', #42860, #7477, #25503, .T. ) ;
#43993 = ORIENTED_EDGE ( 'NONE', *, *, #5690, .F. ) ;
#43994 = ORIENTED_EDGE ( 'NONE', *, *, #22760, .F. ) ;
#43995 = LINE ( 'NONE', #36527, #14963 ) ;
#43996 = AXIS2_PLACEMENT_3D ( 'NONE', #7032, #45992, #22524 ) ;
#43997 = CARTESIAN_POINT ( 'NONE',  ( 0.000000000000000000, 3.313179664429866556, 0.000000000000000000 ) ) ;
#43998 = EDGE_LOOP ( 'NONE', ( #12662, #8656, #4839, #42222 ) ) ;
#43999 = CARTESIAN_POINT ( 'NONE',  ( -0.3486774197067339376, 0.000000000000000000, -1.889763779527552146 ) ) ;
#44000 = DIRECTION ( 'NONE',  ( 1.000000000000000000, 0.000000000000000000, -3.469446951953613696E-16 ) ) ;
#44001 = CARTESIAN_POINT ( 'NONE',  ( 2.139229417893225627, 0.000000000000000000, -0.3394403656973398742 ) ) ;
#44002 = ADVANCED_FACE ( 'NONE', ( #4429 ), #48273, .F. ) ;
#44003 = CARTESIAN_POINT ( 'NONE',  ( 1.287906020515829919, 3.346456692913386100, -1.259842519685035134 ) ) ;
#44004 = ORIENTED_EDGE ( 'NONE', *, *, #12047, .T. ) ;
#44005 = ORIENTED_EDGE ( 'NONE', *, *, #43608, .F. ) ;
#44006 = PLANE ( 'NONE',  #12229 ) ;
#44007 = LINE ( 'NONE', #8651, #41463 ) ;
#44008 = CARTESIAN_POINT ( 'NONE',  ( -0.6233543567505162031, 1.574803149606302854, -2.073689640095379705 ) ) ;
#44009 = DIRECTION ( 'NONE',  ( 1.734723475976806848E-16, -0.000000000000000000, 1.000000000000000000 ) ) ;
#44010 = FACE_BOUND ( 'NONE', #41129, .T. ) ;
#44011 = ORIENTED_EDGE ( 'NONE', *, *, #10466, .F. ) ;
#44012 = EDGE_CURVE ( 'NONE', #30696, #46419, #8300, .T. ) ;
#44013 = CARTESIAN_POINT ( 'NONE',  ( 0.2156685157584260770, 1.510622172706404864, -2.945280361644574185 ) ) ;
#44014 = ORIENTED_EDGE ( 'NONE', *, *, #45459, .T. ) ;
#44015 = ORIENTED_EDGE ( 'NONE', *, *, #33378, .T. ) ;
#44016 = DIRECTION ( 'NONE',  ( 0.5508969814520945363, 0.000000000000000000, 0.8345732537213079727 ) ) ;
#44017 = EDGE_CURVE ( 'NONE', #39335, #26738, #3464, .T. ) ;
#44018 = ORIENTED_EDGE ( 'NONE', *, *, #36639, .F. ) ;
#44019 = ORIENTED_EDGE ( 'NONE', *, *, #18684, .T. ) ;
#44020 = CARTESIAN_POINT ( 'NONE',  ( 0.2727639067037604947, 3.346456692913386100, -0.1574803149606298636 ) ) ;
#44021 = ORIENTED_EDGE ( 'NONE', *, *, #42060, .T. ) ;
#44022 = AXIS2_PLACEMENT_3D ( 'NONE', #8920, #16676, #5045 ) ;
#44023 = AXIS2_PLACEMENT_3D ( 'NONE', #35648, #15518, #16281 ) ;
#44024 = AXIS2_PLACEMENT_3D ( 'NONE', #5844, #29847, #33986 ) ;
#44025 = CARTESIAN_POINT ( 'NONE',  ( -1.636583440222563635, 3.267716535433071279, 0.1181102362204704270 ) ) ;
#44026 = CARTESIAN_POINT ( 'NONE',  ( -2.277873973731453727, 1.585326468414270495, 1.879489153247635214 ) ) ;
#44027 = CARTESIAN_POINT ( 'NONE',  ( 0.5284761224300889015, 5.905511811023623991, -2.099874368989729234 ) ) ;
#44028 = VECTOR ( 'NONE', #17145, 39.37007874015748143 ) ;
#44029 = ADVANCED_FACE ( 'NONE', ( #35930 ), #12428, .T. ) ;
#44030 = AXIS2_PLACEMENT_3D ( 'NONE', #26581, #26084, #37468 ) ;
#44031 = DIRECTION ( 'NONE',  ( 0.000000000000000000, -1.000000000000000000, 0.000000000000000000 ) ) ;
#44032 = EDGE_CURVE ( 'NONE', #34431, #7984, #43912, .T. ) ;
#44033 = LINE ( 'NONE', #8676, #8013 ) ;
#44034 = DIRECTION ( 'NONE',  ( -0.000000000000000000, 1.000000000000000000, -0.000000000000000000 ) ) ;
#44035 = VECTOR ( 'NONE', #47569, 39.37007874015748143 ) ;
#44036 = ORIENTED_EDGE ( 'NONE', *, *, #35242, .T. ) ;
#44037 = CARTESIAN_POINT ( 'NONE',  ( 1.583112249919723213, 0.000000000000000000, -0.7301740747847023094 ) ) ;
#44038 = PLANE ( 'NONE',  #466 ) ;
#44039 = PLANE ( 'NONE',  #10019 ) ;
#44040 = ORIENTED_EDGE ( 'NONE', *, *, #4406, .F. ) ;
#44041 = DIRECTION ( 'NONE',  ( -3.469446951953613696E-16, 0.000000000000000000, -1.000000000000000000 ) ) ;
#44042 = CARTESIAN_POINT ( 'NONE',  ( -1.152895553066196177, 0.000000000000000000, -1.833672301139088745 ) ) ;
#44043 = ORIENTED_EDGE ( 'NONE', *, *, #26926, .T. ) ;
#44044 = DIRECTION ( 'NONE',  ( 5.063291518728965670E-17, 1.000000000000000000, 1.184615939703122503E-16 ) ) ;
#44045 = CARTESIAN_POINT ( 'NONE',  ( 0.000000000000000000, 3.267716535433071279, -2.086614173228339641 ) ) ;
#44046 = DIRECTION ( 'NONE',  ( -1.000000000000000000, -0.000000000000000000, -0.000000000000000000 ) ) ;
#44047 = EDGE_LOOP ( 'NONE', ( #30679, #18413, #37697, #46479 ) ) ;
#44048 = CARTESIAN_POINT ( 'NONE',  ( 0.08139965876239094178, 1.610780518492231694, 0.000000000000000000 ) ) ;
#44049 = ORIENTED_EDGE ( 'NONE', *, *, #37952, .T. ) ;
#44050 = DIRECTION ( 'NONE',  ( -0.9998717552508122886, -0.01601477604151181275, 0.000000000000000000 ) ) ;
#44051 = CARTESIAN_POINT ( 'NONE',  ( 1.015142113812069313, 3.346456692913386100, -0.3543307086614175816 ) ) ;
#44052 = LINE ( 'NONE', #28310, #7801 ) ;
#44053 = CARTESIAN_POINT ( 'NONE',  ( 2.322368699764507216, 1.646673738916892837, -0.1535599007534338978 ) ) ;
#44054 = EDGE_CURVE ( 'NONE', #37003, #14034, #40323, .T. ) ;
#44055 = PLANE ( 'NONE',  #25524 ) ;
#44056 = EDGE_LOOP ( 'NONE', ( #32323, #31832, #20474 ) ) ;
#44057 = ORIENTED_EDGE ( 'NONE', *, *, #20502, .T. ) ;
#44058 = DIRECTION ( 'NONE',  ( 0.000000000000000000, -1.000000000000000000, 0.000000000000000000 ) ) ;
#44059 = ORIENTED_EDGE ( 'NONE', *, *, #49769, .T. ) ;
#44060 = AXIS2_PLACEMENT_3D ( 'NONE', #25213, #24452, #32202 ) ;
#44061 = LINE ( 'NONE', #1721, #14528 ) ;
#44062 = ORIENTED_EDGE ( 'NONE', *, *, #13364, .F. ) ;
#44063 = EDGE_CURVE ( 'NONE', #31184, #49197, #16825, .T. ) ;
#44064 = VECTOR ( 'NONE', #43540, 39.37007874015748143 ) ;
#44065 = VECTOR ( 'NONE', #31479, 39.37007874015748143 ) ;
#44066 = DIRECTION ( 'NONE',  ( -3.469446951953613696E-16, 0.000000000000000000, -1.000000000000000000 ) ) ;
#44067 = EDGE_CURVE ( 'NONE', #42204, #24086, #4904, .T. ) ;
#44068 = B_SPLINE_CURVE_WITH_KNOTS ( 'NONE', 3,
 ( #49404, #36817, #1187, #13828 ),
 .UNSPECIFIED., .F., .F.,
 ( 4, 4 ),
 ( 6.437188407750467112E-07, 0.003699879688711244820 ),
 .UNSPECIFIED. ) ;
#44069 = ORIENTED_EDGE ( 'NONE', *, *, #11265, .T. ) ;
#44070 = CARTESIAN_POINT ( 'NONE',  ( -0.3486774197067340486, 3.346456692913386100, -0.1968503937007883287 ) ) ;
#44071 = ADVANCED_FACE ( 'NONE', ( #31623 ), #36268, .F. ) ;
#44072 = PLANE ( 'NONE',  #3375 ) ;
#44073 = VECTOR ( 'NONE', #42716, 39.37007874015748143 ) ;
#44074 = ORIENTED_EDGE ( 'NONE', *, *, #11278, .T. ) ;
#44075 = DIRECTION ( 'NONE',  ( 0.000000000000000000, 1.000000000000000000, 0.000000000000000000 ) ) ;
#44076 = ORIENTED_EDGE ( 'NONE', *, *, #27237, .T. ) ;
#44077 = DIRECTION ( 'NONE',  ( -1.000000000000000000, -0.000000000000000000, -0.000000000000000000 ) ) ;
#44078 = ORIENTED_EDGE ( 'NONE', *, *, #17879, .T. ) ;
#44079 = VERTEX_POINT ( 'NONE', #20245 ) ;
#44080 = EDGE_CURVE ( 'NONE', #33373, #13332, #637, .T. ) ;
#44081 = CARTESIAN_POINT ( 'NONE',  ( -4.268512490100411402E-16, 3.346456692913386100, -2.401574803149598480 ) ) ;
#44082 = VERTEX_POINT ( 'NONE', #32142 ) ;
#44083 = LINE ( 'NONE', #24225, #5645 ) ;
#44084 = ORIENTED_EDGE ( 'NONE', *, *, #26912, .F. ) ;
#44085 = LINE ( 'NONE', #982, #36782 ) ;
#44086 = ADVANCED_FACE ( 'NONE', ( #12505 ), #12771, .F. ) ;
#44087 = CARTESIAN_POINT ( 'NONE',  ( 0.000000000000000000, 3.267716535433071279, 1.692913385826762873 ) ) ;
#44089 = ADVANCED_FACE ( 'NONE', ( #19982 ), #26350, .T. ) ;
#44088 = CARTESIAN_POINT ( 'NONE',  ( -0.3486774197067334380, 0.000000000000000000, 0.9448818897637749625 ) ) ;
#44090 = ADVANCED_FACE ( 'NONE', ( #35746 ), #39621, .F. ) ;
#44091 = ORIENTED_EDGE ( 'NONE', *, *, #20243, .F. ) ;
#44092 = VERTEX_POINT ( 'NONE', #8891 ) ;
#44093 = LINE ( 'NONE', #16746, #16243 ) ;
#44094 = CARTESIAN_POINT ( 'NONE',  ( -0.07591351300297340121, 0.000000000000000000, -1.299212598425193210 ) ) ;
#44095 = VECTOR ( 'NONE', #3656, 39.37007874015748143 ) ;
#44096 = PLANE ( 'NONE',  #50463 ) ;
#44097 = DIRECTION ( 'NONE',  ( -1.000000000000000000, 0.000000000000000000, 0.000000000000000000 ) ) ;
#44098 = VECTOR ( 'NONE', #2589, 39.37007874015748143 ) ;
#44099 = LINE ( 'NONE', #9765, #21886 ) ;
#44100 = VECTOR ( 'NONE', #33989, 39.37007874015748143 ) ;
#44101 = CARTESIAN_POINT ( 'NONE',  ( 2.157073429634569717, 0.5219348593605198650, 0.7526208317096673150 ) ) ;
#44102 = DIRECTION ( 'NONE',  ( 1.000000000000000000, 0.000000000000000000, 0.000000000000000000 ) ) ;
#44103 = ORIENTED_EDGE ( 'NONE', *, *, #17480, .F. ) ;
#44104 = B_SPLINE_CURVE_WITH_KNOTS ( 'NONE', 3,
 ( #27868, #31501, #12648, #23750 ),
 .UNSPECIFIED., .F., .F.,
 ( 4, 4 ),
 ( 0.001530659381711838756, 0.04616820643450836315 ),
 .UNSPECIFIED. ) ;
#44105 = LINE ( 'NONE', #39988, #45706 ) ;
#44106 = CIRCLE ( 'NONE', #22673, 2.244934639244525076 ) ;
#44107 = ORIENTED_EDGE ( 'NONE', *, *, #21542, .T. ) ;
#44108 = CARTESIAN_POINT ( 'NONE',  ( -1.712496953225537188, 3.346456692913386100, -0.03937007874015881204 ) ) ;
#44109 = ORIENTED_EDGE ( 'NONE', *, *, #18170, .F. ) ;
#44110 = LINE ( 'NONE', #9781, #4451 ) ;
#44111 = LINE ( 'NONE', #7987, #21253 ) ;
#44112 = DIRECTION ( 'NONE',  ( 1.734723475976806848E-16, -0.000000000000000000, 1.000000000000000000 ) ) ;
#44113 = CARTESIAN_POINT ( 'NONE',  ( 1.560669927219590747, 0.000000000000000000, 1.102362204724403938 ) ) ;
#44114 = ORIENTED_EDGE ( 'NONE', *, *, #33098, .F. ) ;
#44115 = CARTESIAN_POINT ( 'NONE',  ( -0.9914495361339012991, 1.703811331058339373, 2.781765111341808705 ) ) ;
#44116 = FACE_BOUND ( 'NONE', #30573, .T. ) ;
#44117 = ORIENTED_EDGE ( 'NONE', *, *, #44287, .F. ) ;
#44118 = CARTESIAN_POINT ( 'NONE',  ( 0.000000000000000000, 5.905511811023623991, 0.000000000000000000 ) ) ;
#44119 = ORIENTED_EDGE ( 'NONE', *, *, #40583, .F. ) ;
#44120 = DIRECTION ( 'NONE',  ( 0.000000000000000000, 0.000000000000000000, 1.000000000000000000 ) ) ;
#44121 = CARTESIAN_POINT ( 'NONE',  ( 2.813306935136158149, 1.763089614240364256, 0.8968503919106445288 ) ) ;
#44122 = EDGE_CURVE ( 'NONE', #11359, #12085, #43476, .T. ) ;
#44123 = ADVANCED_FACE ( 'NONE', ( #27735 ), #8125, .T. ) ;
#44124 = EDGE_CURVE ( 'NONE', #49030, #2108, #15860, .T. ) ;
#44125 = CARTESIAN_POINT ( 'NONE',  ( 0.08139965876239094178, 1.610780518492231694, 0.000000000000000000 ) ) ;
#44126 = AXIS2_PLACEMENT_3D ( 'NONE', #17263, #13381, #17761 ) ;
#44127 = ORIENTED_EDGE ( 'NONE', *, *, #24686, .T. ) ;
#44128 = EDGE_LOOP ( 'NONE', ( #44319, #48662, #23250, #22758, #16298, #4914, #22239, #41230, #12564, #26105, #39090 ) ) ;
#44129 = AXIS2_PLACEMENT_3D ( 'NONE', #42608, #26361, #34375 ) ;
#44130 = PLANE ( 'NONE',  #3752 ) ;
#44131 = CARTESIAN_POINT ( 'NONE',  ( -2.952069331832154919, 5.118110236220475784, -1.181102362204724310 ) ) ;
#44132 = LINE ( 'NONE', #17046, #32633 ) ;
#44133 = VECTOR ( 'NONE', #30797, 39.37007874015748143 ) ;
#44134 = EDGE_CURVE ( 'NONE', #11433, #44433, #43990, .T. ) ;
#44135 = FACE_OUTER_BOUND ( 'NONE', #15383, .T. ) ;
#44136 = FACE_OUTER_BOUND ( 'NONE', #13078, .T. ) ;
#44137 = VECTOR ( 'NONE', #43363, 39.37007874015748143 ) ;
#44138 = ORIENTED_EDGE ( 'NONE', *, *, #30752, .T. ) ;
#44139 = CARTESIAN_POINT ( 'NONE',  ( -1.166969139818015755, 3.267716535433071279, -0.03937007874015868020 ) ) ;
#44140 = VECTOR ( 'NONE', #21855, 39.37007874015748143 ) ;
#44141 = ORIENTED_EDGE ( 'NONE', *, *, #40583, .T. ) ;
#44142 = ORIENTED_EDGE ( 'NONE', *, *, #6758, .T. ) ;
#44143 = ADVANCED_FACE ( 'NONE', ( #44251 ), #8637, .F. ) ;
#44144 = ORIENTED_EDGE ( 'NONE', *, *, #30788, .T. ) ;
#44145 = CARTESIAN_POINT ( 'NONE',  ( 2.576863348864710801, 1.660943078747768364, 1.442554885838449819 ) ) ;
#44146 = CARTESIAN_POINT ( 'NONE',  ( 0.000000000000000000, 2.755905511811024056, 0.000000000000000000 ) ) ;
#44147 = EDGE_CURVE ( 'NONE', #22729, #50486, #20512, .T. ) ;
#44148 = LINE ( 'NONE', #45156, #30029 ) ;
#44149 = CARTESIAN_POINT ( 'NONE',  ( 2.919426793319799707, 1.666276233232717896, 0.4451252810446822417 ) ) ;
#44150 = EDGE_CURVE ( 'NONE', #6703, #26688, #889, .T. ) ;
#44151 = EDGE_LOOP ( 'NONE', ( #46082, #24370, #40208, #13370, #3009, #7073, #25994, #43300, #30456, #42041, #19693, #50105, #17679 ) ) ;
#44152 = VERTEX_POINT ( 'NONE', #40140 ) ;
#44153 = CARTESIAN_POINT ( 'NONE',  ( -1.080768593899272823, 0.000000000000000000, -1.459517500771556620 ) ) ;
#44154 = DIRECTION ( 'NONE',  ( 1.000000000000000000, 0.000000000000000000, -3.469446951953613696E-16 ) ) ;
#44155 = EDGE_CURVE ( 'NONE', #6809, #5773, #13885, .T. ) ;
#44156 = LINE ( 'NONE', #40813, #212 ) ;
#44157 = ADVANCED_FACE ( 'NONE', ( #30672 ), #46116, .T. ) ;
#44158 = CARTESIAN_POINT ( 'NONE',  ( 2.378961647330872786, 0.000000000000000000, 0.3149606299212573401 ) ) ;
#44159 = FACE_OUTER_BOUND ( 'NONE', #50134, .T. ) ;
#44160 = DIRECTION ( 'NONE',  ( -3.469446951953613696E-16, 0.000000000000000000, -1.000000000000000000 ) ) ;
#44161 = FACE_OUTER_BOUND ( 'NONE', #16098, .T. ) ;
#44162 = CARTESIAN_POINT ( 'NONE',  ( 0.000000000000000000, 6.692913385826772199, 0.000000000000000000 ) ) ;
#44163 = ORIENTED_EDGE ( 'NONE', *, *, #34725, .T. ) ;
#44164 =( GEOMETRIC_REPRESENTATION_CONTEXT ( 3 ) GLOBAL_UNCERTAINTY_ASSIGNED_CONTEXT ( ( #29306 ) ) GLOBAL_UNIT_ASSIGNED_CONTEXT ( ( #10660, #3408, #30277 ) ) REPRESENTATION_CONTEXT ( 'NONE', 'WORKASPACE' ) );
#44165 = CARTESIAN_POINT ( 'NONE',  ( -0.06966273521059175577, -0.6299212598425202314, 0.3674709282358789575 ) ) ;
#44166 = DIRECTION ( 'NONE',  ( 1.734723475976806848E-16, -0.000000000000000000, 1.000000000000000000 ) ) ;
#44167 = CONICAL_SURFACE ( 'NONE', #40868, 1.850107469027523210, 0.6386652850508578450 ) ;
#44168 = ORIENTED_EDGE ( 'NONE', *, *, #2840, .F. ) ;
#44169 = VECTOR ( 'NONE', #48101, 39.37007874015748143 ) ;
#44170 = EDGE_LOOP ( 'NONE', ( #23668, #21518, #32126, #24954 ) ) ;
#44171 = CARTESIAN_POINT ( 'NONE',  ( 1.833433833923351353, 0.000000000000000000, 0.9448818897637746295 ) ) ;
#44172 = DIRECTION ( 'NONE',  ( 0.1938878870612535388, -0.000000000000000000, 0.9810236935216818388 ) ) ;
#44173 = DIRECTION ( 'NONE',  ( -3.469446951953613696E-16, 0.000000000000000000, -1.000000000000000000 ) ) ;
#44174 = VECTOR ( 'NONE', #6250, 39.37007874015748143 ) ;
#44175 = ORIENTED_EDGE ( 'NONE', *, *, #33812, .F. ) ;
#44176 = VECTOR ( 'NONE', #14932, 39.37007874015748143 ) ;
#44177 = ORIENTED_EDGE ( 'NONE', *, *, #47659, .T. ) ;
#44178 = FACE_OUTER_BOUND ( 'NONE', #47921, .T. ) ;
#44179 = ORIENTED_EDGE ( 'NONE', *, *, #45189, .T. ) ;
#44180 = LINE ( 'NONE', #29665, #41089 ) ;
#44181 = EDGE_LOOP ( 'NONE', ( #11848, #15314, #19348, #47652 ) ) ;
#44182 = CARTESIAN_POINT ( 'NONE',  ( -1.363819533518803029, 3.267716535433071279, 0.9055118110236167750 ) ) ;
#44183 = DIRECTION ( 'NONE',  ( 1.000000000000000000, 0.000000000000000000, -3.469446951953613696E-16 ) ) ;
#44184 = LINE ( 'NONE', #24577, #2145 ) ;
#44185 = EDGE_LOOP ( 'NONE', ( #36323, #27166, #30473, #33065, #36867, #23417, #38161 ) ) ;
#44186 = EDGE_CURVE ( 'NONE', #3260, #11420, #46383, .T. ) ;
#44187 = ORIENTED_EDGE ( 'NONE', *, *, #9777, .F. ) ;
#44188 = ORIENTED_EDGE ( 'NONE', *, *, #564, .F. ) ;
#44189 = DIRECTION ( 'NONE',  ( -0.9998717552508122886, -0.01601477604151185785, 0.000000000000000000 ) ) ;
#44190 = EDGE_CURVE ( 'NONE', #10246, #19504, #9403, .T. ) ;
#44191 = ORIENTED_EDGE ( 'NONE', *, *, #14666, .T. ) ;
#44192 = ORIENTED_EDGE ( 'NONE', *, *, #33913, .F. ) ;
#44193 = CARTESIAN_POINT ( 'NONE',  ( -0.2727639067037607723, 3.346456692913386100, -0.4724409448818883694 ) ) ;
#44194 = CARTESIAN_POINT ( 'NONE',  ( -1.363819533518803029, 3.267716535433071279, 2.365849761790804994E-16 ) ) ;
#44195 = CARTESIAN_POINT ( 'NONE',  ( 2.518955203866161785, 1.653166854136447483, 0.2915536147086987273 ) ) ;
#44196 = EDGE_CURVE ( 'NONE', #35414, #23952, #37291, .T. ) ;
#44197 = ORIENTED_EDGE ( 'NONE', *, *, #9558, .T. ) ;
#44198 = CARTESIAN_POINT ( 'NONE',  ( -2.001301579076982584, 3.346456692913386100, -0.8267716535433052849 ) ) ;
#44199 = CARTESIAN_POINT ( 'NONE',  ( -1.712496953225537633, 3.267716535433071279, -1.102362204724405492 ) ) ;
#44200 = CARTESIAN_POINT ( 'NONE',  ( 1.015142113812069313, 3.346456692913386100, -0.03937007874015881204 ) ) ;
#44201 = AXIS2_PLACEMENT_3D ( 'NONE', #34653, #46238, #45732 ) ;
#44202 = ORIENTED_EDGE ( 'NONE', *, *, #27515, .T. ) ;
#44203 = LINE ( 'NONE', #47535, #44674 ) ;
#44204 = CARTESIAN_POINT ( 'NONE',  ( 0.7423782071083085965, 3.346456692913386100, -1.141732283464564013 ) ) ;
#44205 = VECTOR ( 'NONE', #6640, 39.37007874015748143 ) ;
#44206 = ORIENTED_EDGE ( 'NONE', *, *, #5220, .T. ) ;
#44207 = VECTOR ( 'NONE', #24681, 39.37007874015748143 ) ;
#44208 = CARTESIAN_POINT ( 'NONE',  ( -2.889674983507169337, 1.575792602931942232, -0.6090712660038034576 ) ) ;
#44209 = ORIENTED_EDGE ( 'NONE', *, *, #31812, .T. ) ;
#44210 = ORIENTED_EDGE ( 'NONE', *, *, #24264, .F. ) ;
#44211 = CARTESIAN_POINT ( 'NONE',  ( -0.9838852166859196613, 5.905511811023623991, 1.929635236160304190 ) ) ;
#44212 = FACE_OUTER_BOUND ( 'NONE', #29810, .T. ) ;
#44213 = VECTOR ( 'NONE', #12200, 39.37007874015748143 ) ;
#44214 = CARTESIAN_POINT ( 'NONE',  ( 0.08139965876239094178, 1.610780518492231694, 0.000000000000000000 ) ) ;
#44215 = ADVANCED_FACE ( 'NONE', ( #33678 ), #1398, .F. ) ;
#44216 = VECTOR ( 'NONE', #24677, 39.37007874015748143 ) ;
#44217 = DIRECTION ( 'NONE',  ( 5.779879058770898378E-18, 1.000000000000000000, 1.286990067732318227E-16 ) ) ;
#44218 = DIRECTION ( 'NONE',  ( -0.000000000000000000, 1.000000000000000000, -0.000000000000000000 ) ) ;
#44219 = EDGE_LOOP ( 'NONE', ( #19306, #22511, #15590, #38728 ) ) ;
#44220 = ORIENTED_EDGE ( 'NONE', *, *, #10749, .T. ) ;
#44221 = VECTOR ( 'NONE', #33996, 39.37007874015748143 ) ;
#44222 = EDGE_CURVE ( 'NONE', #42166, #337, #28759, .T. ) ;
#44223 = ADVANCED_FACE ( 'NONE', ( #32658 ), #17913, .T. ) ;
#44224 = DIRECTION ( 'NONE',  ( -0.000000000000000000, 1.000000000000000000, -0.000000000000000000 ) ) ;
#44225 = ORIENTED_EDGE ( 'NONE', *, *, #9348, .F. ) ;
#44226 = CARTESIAN_POINT ( 'NONE',  ( 0.000000000000000000, 3.346456692913386100, -2.106299212598425008 ) ) ;
#44227 = DIRECTION ( 'NONE',  ( -0.2660368455666687892, 0.000000000000000000, -0.9639628606958549062 ) ) ;
#44228 = CARTESIAN_POINT ( 'NONE',  ( 1.636583440222563857, 3.267716535433071279, -0.6299212598425181220 ) ) ;
#44229 = DIRECTION ( 'NONE',  ( 1.734723475976806848E-16, 0.000000000000000000, 1.000000000000000000 ) ) ;
#44230 = CARTESIAN_POINT ( 'NONE',  ( 2.249085127468613443, 1.747331752236621183, 1.154398728974792565 ) ) ;
#44231 = ORIENTED_EDGE ( 'NONE', *, *, #23210, .F. ) ;
#44232 = CARTESIAN_POINT ( 'NONE',  ( 0.1155636338427008941, -0.5222242541845523167, 0.000000000000000000 ) ) ;
#44233 = CARTESIAN_POINT ( 'NONE',  ( 2.623503965249849301, 1.205361022782829114E-17, 1.355882097269873965 ) ) ;
#44234 = VERTEX_POINT ( 'NONE', #5018 ) ;
#44235 = CARTESIAN_POINT ( 'NONE',  ( 1.833433833923351353, 3.267716535433071279, 1.259842519685033135 ) ) ;
#44236 = DIRECTION ( 'NONE',  ( -0.000000000000000000, 0.000000000000000000, 1.000000000000000000 ) ) ;
#44237 = DIRECTION ( 'NONE',  ( -2.582876339026174526E-17, -1.000000000000000000, -1.131632063491654496E-16 ) ) ;
#44238 = ORIENTED_EDGE ( 'NONE', *, *, #35117, .T. ) ;
#44239 = VECTOR ( 'NONE', #4935, 39.37007874015748143 ) ;
#44240 = DIRECTION ( 'NONE',  ( -1.000000000000000000, 0.000000000000000000, 0.000000000000000000 ) ) ;
#44241 = PLANE ( 'NONE',  #32444 ) ;
#44242 = CARTESIAN_POINT ( 'NONE',  ( 1.836342932631641167, 0.000000000000000000, 1.044063857347276469 ) ) ;
#44243 = VECTOR ( 'NONE', #5371, 39.37007874015748143 ) ;
#44244 = AXIS2_PLACEMENT_3D ( 'NONE', #44976, #1370, #2135 ) ;
#44245 = ORIENTED_EDGE ( 'NONE', *, *, #42683, .F. ) ;
#44246 = CARTESIAN_POINT ( 'NONE',  ( -1.929629134066536134, 6.692913385826772199, 0.9824921284572121216 ) ) ;
#44247 = CARTESIAN_POINT ( 'NONE',  ( -1.166969139818015977, 3.346456692913386100, -0.1574803149606300023 ) ) ;
#44248 = ORIENTED_EDGE ( 'NONE', *, *, #33978, .T. ) ;
#44249 = LINE ( 'NONE', #4763, #11366 ) ;
#44250 = CARTESIAN_POINT ( 'NONE',  ( -0.8182917201112819283, 3.346456692913386100, -0.1574803149606301411 ) ) ;
#44251 = FACE_OUTER_BOUND ( 'NONE', #27085, .T. ) ;
#44252 = CARTESIAN_POINT ( 'NONE',  ( -1.166969139818015977, 0.000000000000000000, -0.1574803149606300023 ) ) ;
#44253 = AXIS2_PLACEMENT_3D ( 'NONE', #47545, #856, #48312 ) ;
#44254 = ORIENTED_EDGE ( 'NONE', *, *, #15303, .T. ) ;
#44255 = ORIENTED_EDGE ( 'NONE', *, *, #6068, .T. ) ;
#44256 = LINE ( 'NONE', #19987, #37267 ) ;
#44257 = DIRECTION ( 'NONE',  ( 0.000000000000000000, -1.000000000000000000, -0.000000000000000000 ) ) ;
#44258 = ADVANCED_FACE ( 'NONE', ( #17662 ), #25656, .F. ) ;
#44259 = VERTEX_POINT ( 'NONE', #48599 ) ;
#44260 = LINE ( 'NONE', #24654, #8581 ) ;
#44261 = CARTESIAN_POINT ( 'NONE',  ( 2.823445274216730638, 1.205361022782829114E-17, 0.8656477926280680135 ) ) ;
#44262 = CARTESIAN_POINT ( 'NONE',  ( -1.363819533518803473, 3.346456692913386100, 2.047244094488179567 ) ) ;
#44263 = EDGE_CURVE ( 'NONE', #17636, #4073, #41162, .T. ) ;
#44264 = CARTESIAN_POINT ( 'NONE',  ( 1.287906020515830141, 3.346456692913386100, -8.878505979408855953E-16 ) ) ;
#44265 = ORIENTED_EDGE ( 'NONE', *, *, #42619, .T. ) ;
#44266 = ORIENTED_EDGE ( 'NONE', *, *, #4382, .T. ) ;
#44267 = ADVANCED_FACE ( 'NONE', ( #40403 ), #37547, .F. ) ;
#44268 = CARTESIAN_POINT ( 'NONE',  ( 1.412396057062172305, -1.971265646866911096E-16, 1.691415513056038877 ) ) ;
#44269 = CARTESIAN_POINT ( 'NONE',  ( 0.5455278134075211005, 0.000000000000000000, -1.141732283464564013 ) ) ;
#44270 = DIRECTION ( 'NONE',  ( -3.469446951953613696E-16, 0.000000000000000000, -1.000000000000000000 ) ) ;
#44271 = EDGE_CURVE ( 'NONE', #17812, #30118, #5271, .T. ) ;
#44272 = ORIENTED_EDGE ( 'NONE', *, *, #17282, .F. ) ;
#44273 = LINE ( 'NONE', #8912, #9210 ) ;
#44274 = FACE_BOUND ( 'NONE', #19485, .T. ) ;
#44275 = ORIENTED_EDGE ( 'NONE', *, *, #31083, .F. ) ;
#44276 = CARTESIAN_POINT ( 'NONE',  ( -0.8182917201112819283, 3.346456692913386100, -1.417322834645664331 ) ) ;
#44277 = VERTEX_POINT ( 'NONE', #36520 ) ;
#44278 = ORIENTED_EDGE ( 'NONE', *, *, #17589, .T. ) ;
#44279 = CARTESIAN_POINT ( 'NONE',  ( -0.5455278134075208785, 0.000000000000000000, 1.062992125984246083 ) ) ;
#44280 = EDGE_CURVE ( 'NONE', #1365, #36460, #48346, .T. ) ;
#44281 = VECTOR ( 'NONE', #7359, 39.37007874015748143 ) ;
#44282 = VERTEX_POINT ( 'NONE', #9147 ) ;
#44283 = ORIENTED_EDGE ( 'NONE', *, *, #48985, .T. ) ;
#44284 = LINE ( 'NONE', #20012, #26931 ) ;
#44285 = ORIENTED_EDGE ( 'NONE', *, *, #23268, .F. ) ;
#44286 = VECTOR ( 'NONE', #35030, 39.37007874015748143 ) ;
#44287 = EDGE_CURVE ( 'NONE', #34275, #42801, #1140, .T. ) ;
#44288 = CARTESIAN_POINT ( 'NONE',  ( 0.000000000000000000, 3.267716535433071279, -0.3149606299212591165 ) ) ;
#44289 = CARTESIAN_POINT ( 'NONE',  ( -2.077187562400836907, 1.584429483328545274, 1.719447080701160591 ) ) ;
#44290 = PLANE ( 'NONE',  #42364 ) ;
#44291 = ADVANCED_FACE ( 'NONE', ( #36774, #1909 ), #9660, .T. ) ;
#44292 = PLANE ( 'NONE',  #22296 ) ;
#44293 = CARTESIAN_POINT ( 'NONE',  ( 0.000000000000000000, 3.267716535433071279, -0.1574803149606300023 ) ) ;
#44294 = LINE ( 'NONE', #13073, #9708 ) ;
#44295 = VERTEX_POINT ( 'NONE', #13791 ) ;
#44296 = DIRECTION ( 'NONE',  ( -0.9998717552508122886, -0.01601477604151181275, 0.000000000000000000 ) ) ;
#44297 = VECTOR ( 'NONE', #48191, 39.37007874015748143 ) ;
#44298 = ADVANCED_FACE ( 'NONE', ( #13282 ), #29013, .F. ) ;
#44299 = CARTESIAN_POINT ( 'NONE',  ( 1.806430656273612767, 0.5249316475426862860, 0.5351997119015522442 ) ) ;
#44300 = ORIENTED_EDGE ( 'NONE', *, *, #16986, .T. ) ;
#44301 = CARTESIAN_POINT ( 'NONE',  ( 0.5455278134075216556, 0.000000000000000000, 2.007874015748021268 ) ) ;
#44302 = CARTESIAN_POINT ( 'NONE',  ( -0.4788131938641533303, 1.525670379232220375, 2.914091152102185944 ) ) ;
#44303 = ORIENTED_EDGE ( 'NONE', *, *, #22026, .F. ) ;
#44304 = PLANE ( 'NONE',  #43584 ) ;
#44305 = DIRECTION ( 'NONE',  ( 0.000000000000000000, 0.000000000000000000, -1.000000000000000000 ) ) ;
#44306 = CARTESIAN_POINT ( 'NONE',  ( -0.8942052331142547050, 3.267716535433071279, 1.062992125984246083 ) ) ;
#44307 = ORIENTED_EDGE ( 'NONE', *, *, #9469, .F. ) ;
#44308 = DIRECTION ( 'NONE',  ( -1.000000000000000000, -0.000000000000000000, -0.000000000000000000 ) ) ;
#44309 = EDGE_LOOP ( 'NONE', ( #3124, #48479, #17625, #33871 ) ) ;
#44310 = FACE_BOUND ( 'NONE', #8850, .T. ) ;
#44311 = CARTESIAN_POINT ( 'NONE',  ( -0.2727639067037607723, 0.000000000000000000, -1.102362204724405714 ) ) ;
#44312 = LINE ( 'NONE', #24959, #2842 ) ;
#44313 = CARTESIAN_POINT ( 'NONE',  ( 0.002207914879453961969, 5.905511811023623991, 0.04916304461325442243 ) ) ;
#44314 = VECTOR ( 'NONE', #43938, 39.37007874015748143 ) ;
#44315 = VECTOR ( 'NONE', #46935, 39.37007874015748143 ) ;
#44316 = ORIENTED_EDGE ( 'NONE', *, *, #18299, .F. ) ;
#44317 = ORIENTED_EDGE ( 'NONE', *, *, #37145, .F. ) ;
#44318 = FACE_OUTER_BOUND ( 'NONE', #10606, .T. ) ;
#44319 = ORIENTED_EDGE ( 'NONE', *, *, #36697, .T. ) ;
#44320 = VECTOR ( 'NONE', #38449, 39.37007874015748143 ) ;
#44321 = FACE_OUTER_BOUND ( 'NONE', #46399, .T. ) ;
#44322 = VERTEX_POINT ( 'NONE', #1651 ) ;
#44323 = EDGE_CURVE ( 'NONE', #14478, #33096, #17404, .T. ) ;
#44324 = CARTESIAN_POINT ( 'NONE',  ( 0.000000000000000000, 3.267716535433071279, -0.03937007874015936021 ) ) ;
#44325 = ORIENTED_EDGE ( 'NONE', *, *, #41150, .T. ) ;
#44326 = CARTESIAN_POINT ( 'NONE',  ( -1.062992125984251413, 0.5905511811023621549, 1.062992125984251413 ) ) ;
#44327 = EDGE_CURVE ( 'NONE', #30813, #38209, #13536, .T. ) ;
#44328 = CARTESIAN_POINT ( 'NONE',  ( 1.466506618346834934, 1.205361022782829114E-17, -1.470210429041567401 ) ) ;
#44329 = ORIENTED_EDGE ( 'NONE', *, *, #18412, .T. ) ;
#44330 = CARTESIAN_POINT ( 'NONE',  ( -0.8182917201112819283, 0.000000000000000000, -2.244094488188968395 ) ) ;
#44331 = ORIENTED_EDGE ( 'NONE', *, *, #36343, .T. ) ;
#44332 = VECTOR ( 'NONE', #676, 39.37007874015748143 ) ;
#44333 = DIRECTION ( 'NONE',  ( 1.000000000000000000, 0.000000000000000000, -3.469446951953613696E-16 ) ) ;
#44334 = EDGE_LOOP ( 'NONE', ( #48751, #2550, #27304, #15632 ) ) ;
#44335 = ORIENTED_EDGE ( 'NONE', *, *, #41538, .T. ) ;
#44336 = DIRECTION ( 'NONE',  ( -0.9195277725514544587, 0.000000000000000000, 0.3930250316539147803 ) ) ;
#44337 = ORIENTED_EDGE ( 'NONE', *, *, #18777, .T. ) ;
#44338 = DIRECTION ( 'NONE',  ( -1.000000000000000000, 0.000000000000000000, 0.000000000000000000 ) ) ;
#44339 = ORIENTED_EDGE ( 'NONE', *, *, #2397, .T. ) ;
#44340 = DIRECTION ( 'NONE',  ( 0.000000000000000000, 1.000000000000000000, 0.000000000000000000 ) ) ;
#44341 = DIRECTION ( 'NONE',  ( 1.734723475976806848E-16, 0.000000000000000000, 1.000000000000000000 ) ) ;
#44342 = CONICAL_SURFACE ( 'NONE', #27020, 3.483074324928249421, 1.244861948955335196 ) ;
#44343 = VECTOR ( 'NONE', #2793, 39.37007874015748143 ) ;
#44344 = ADVANCED_FACE ( 'NONE', ( #10675 ), #10923, .T. ) ;
#44345 = CARTESIAN_POINT ( 'NONE',  ( -0.8942052331142547050, 3.346456692913386100, 1.574803149606291974 ) ) ;
#44346 = VERTEX_POINT ( 'NONE', #15050 ) ;
#44347 = CARTESIAN_POINT ( 'NONE',  ( -0.3486774197067340486, 0.000000000000000000, -1.141732283464563791 ) ) ;
#44348 = CARTESIAN_POINT ( 'NONE',  ( 2.516879689376027684, 1.751575581218955513, 0.2912724671682164201 ) ) ;
#44349 = LINE ( 'NONE', #4869, #11752 ) ;
#44350 = DIRECTION ( 'NONE',  ( -0.5128992774059071280, 0.000000000000000000, 0.8584487936018655452 ) ) ;
#44351 = VECTOR ( 'NONE', #40356, 39.37007874015748143 ) ;
#44352 = DIRECTION ( 'NONE',  ( -0.000000000000000000, 0.000000000000000000, 1.000000000000000000 ) ) ;
#44353 = ADVANCED_FACE ( 'NONE', ( #26412 ), #45758, .F. ) ;
#44354 = CARTESIAN_POINT ( 'NONE',  ( 0.4521076751547876138, 1.616718085813380945, 2.215705648545971407 ) ) ;
#44355 = VECTOR ( 'NONE', #30792, 39.37007874015748143 ) ;
#44356 = ADVANCED_FACE ( 'NONE', ( #26168 ), #31049, .F. ) ;
#44357 = LINE ( 'NONE', #43841, #25177 ) ;
#44358 = ORIENTED_EDGE ( 'NONE', *, *, #15924, .T. ) ;
#44359 = CARTESIAN_POINT ( 'NONE',  ( 0.8004649005966348874, 0.000000000000000000, -1.548759025234849762 ) ) ;
#44360 = EDGE_CURVE ( 'NONE', #30424, #11499, #38053, .T. ) ;
#44361 = LINE ( 'NONE', #40251, #34176 ) ;
#44362 = AXIS2_PLACEMENT_3D ( 'NONE', #11829, #23442, #38950 ) ;
#44363 = ORIENTED_EDGE ( 'NONE', *, *, #25620, .F. ) ;
#44364 = DIRECTION ( 'NONE',  ( 1.000000000000000000, -0.000000000000000000, 0.000000000000000000 ) ) ;
#44365 = EDGE_CURVE ( 'NONE', #42296, #10925, #3176, .T. ) ;
#44366 = VECTOR ( 'NONE', #49589, 39.37007874015748143 ) ;
#44367 = VERTEX_POINT ( 'NONE', #42160 ) ;
#44368 = CARTESIAN_POINT ( 'NONE',  ( 0.8182917201112817063, 0.000000000000000000, -2.047244094488181343 ) ) ;
#44369 = EDGE_CURVE ( 'NONE', #11744, #39972, #31737, .T. ) ;
#44370 = CARTESIAN_POINT ( 'NONE',  ( 0.000000000000000000, 3.267716535433071279, -1.732283464566922726 ) ) ;
#44371 = CARTESIAN_POINT ( 'NONE',  ( -0.3780516546848963766, 0.01461794527752662519, 1.807623340459256989 ) ) ;
#44372 = CARTESIAN_POINT ( 'NONE',  ( 2.947574761915768171, 1.205361022782829114E-17, -0.1816379373804913322 ) ) ;
#44373 = CARTESIAN_POINT ( 'NONE',  ( 0.000000000000000000, 3.267716535433071279, 1.889763779527550147 ) ) ;
#44374 = EDGE_LOOP ( 'NONE', ( #48490, #76, #45380, #44603, #31350 ) ) ;
#44375 = CARTESIAN_POINT ( 'NONE',  ( 1.236813753895252166, 1.640077341046696890, -2.681693691597563767 ) ) ;
#44376 = LINE ( 'NONE', #21406, #5604 ) ;
#44377 = ORIENTED_EDGE ( 'NONE', *, *, #32887, .F. ) ;
#44378 = CARTESIAN_POINT ( 'NONE',  ( 1.287906020515830141, 0.000000000000000000, 0.3149606299212578953 ) ) ;
#44379 = EDGE_LOOP ( 'NONE', ( #11824, #23558, #5240, #37042 ) ) ;
#44380 = EDGE_CURVE ( 'NONE', #22546, #10739, #49610, .T. ) ;
#44381 = DIRECTION ( 'NONE',  ( -1.000000000000000000, -0.000000000000000000, -0.000000000000000000 ) ) ;
#44382 = DIRECTION ( 'NONE',  ( -1.156061316345074457E-16, -1.000000000000000000, 1.040474016969491568E-17 ) ) ;
#44383 = CIRCLE ( 'NONE', #14694, 2.165354330708661568 ) ;
#44384 = ADVANCED_FACE ( 'NONE', ( #26910 ), #46756, .F. ) ;
#44385 = CARTESIAN_POINT ( 'NONE',  ( -2.150793259809249847, 1.575027863729615341, -0.2506944975021367372 ) ) ;
#44386 = EDGE_LOOP ( 'NONE', ( #23644, #7956, #39667, #40722 ) ) ;
#44387 = ORIENTED_EDGE ( 'NONE', *, *, #16818, .F. ) ;
#44388 = CARTESIAN_POINT ( 'NONE',  ( 1.152568299495707382, 6.692913385826772199, 1.833124570921553342 ) ) ;
#44389 = DIRECTION ( 'NONE',  ( 0.000000000000000000, 0.000000000000000000, -1.000000000000000000 ) ) ;
#44390 = LINE ( 'NONE', #40016, #35087 ) ;
#44391 = VECTOR ( 'NONE', #35971, 39.37007874015748143 ) ;
#44392 = VECTOR ( 'NONE', #8199, 39.37007874015748143 ) ;
#44393 = DIRECTION ( 'NONE',  ( -1.000000000000000000, 0.000000000000000000, -0.000000000000000000 ) ) ;
#44394 = CARTESIAN_POINT ( 'NONE',  ( 1.833433833923351353, 3.346456692913386100, 0.9448818897637746295 ) ) ;
#44395 = ORIENTED_EDGE ( 'NONE', *, *, #104, .F. ) ;
#44396 = B_SPLINE_CURVE_WITH_KNOTS ( 'NONE', 3,
 ( #44742, #48337, #1900, #13017 ),
 .UNSPECIFIED., .F., .F.,
 ( 4, 4 ),
 ( 2.395904123760600257E-07, 0.002500455472051103887 ),
 .UNSPECIFIED. ) ;
#44397 = CIRCLE ( 'NONE', #22959, 1.743387098533651480 ) ;
#44398 = DIRECTION ( 'NONE',  ( 1.734723475976806848E-16, -0.000000000000000000, 1.000000000000000000 ) ) ;
#44399 = ORIENTED_EDGE ( 'NONE', *, *, #5156, .T. ) ;
#44400 = ORIENTED_EDGE ( 'NONE', *, *, #25935, .T. ) ;
#44401 = VECTOR ( 'NONE', #14657, 39.37007874015748143 ) ;
#44402 = ORIENTED_EDGE ( 'NONE', *, *, #31943, .T. ) ;
#44403 = CARTESIAN_POINT ( 'NONE',  ( 0.07982360342473591996, 1.709180471932028711, 0.000000000000000000 ) ) ;
#44404 = DIRECTION ( 'NONE',  ( 1.734723475976806848E-16, 0.000000000000000000, 1.000000000000000000 ) ) ;
#44405 = AXIS2_PLACEMENT_3D ( 'NONE', #23394, #22896, #31153 ) ;
#44406 = FACE_OUTER_BOUND ( 'NONE', #15487, .T. ) ;
#44407 = CARTESIAN_POINT ( 'NONE',  ( -0.6214413264104939882, 0.000000000000000000, 1.732283464566921172 ) ) ;
#44408 = VERTEX_POINT ( 'NONE', #14287 ) ;
#44409 = ORIENTED_EDGE ( 'NONE', *, *, #35942, .F. ) ;
#44410 = DIRECTION ( 'NONE',  ( 1.734723475976806848E-16, 0.000000000000000000, 1.000000000000000000 ) ) ;
#44411 = LINE ( 'NONE', #9311, #45225 ) ;
#44412 = B_SPLINE_CURVE_WITH_KNOTS ( 'NONE', 3,
 ( #26413, #6297, #2671, #49106 ),
 .UNSPECIFIED., .F., .F.,
 ( 4, 4 ),
 ( 0.1211873102087489551, 0.1625992483279400380 ),
 .UNSPECIFIED. ) ;
#44413 = DIRECTION ( 'NONE',  ( -1.000000000000000000, 0.000000000000000000, -2.891205793294678326E-16 ) ) ;
#44414 = CARTESIAN_POINT ( 'NONE',  ( -2.715141060683412100, 0.000000000000000000, -1.160506983230102040 ) ) ;
#44415 = CARTESIAN_POINT ( 'NONE',  ( -0.07591351300297362326, 3.346456692913386100, -2.104930761696520491 ) ) ;
#44416 = EDGE_CURVE ( 'NONE', #28119, #50243, #30039, .T. ) ;
#44417 = DIRECTION ( 'NONE',  ( 1.000000000000000000, 0.000000000000000000, 0.000000000000000000 ) ) ;
#44418 = VECTOR ( 'NONE', #44257, 39.37007874015748143 ) ;
#44419 = ADVANCED_FACE ( 'NONE', ( #38799 ), #22298, .T. ) ;
#44420 = DIRECTION ( 'NONE',  ( 1.000000000000000000, 0.000000000000000000, -3.469446951953613696E-16 ) ) ;
#44421 = EDGE_CURVE ( 'NONE', #15323, #1336, #50606, .T. ) ;
#44422 = ORIENTED_EDGE ( 'NONE', *, *, #37893, .T. ) ;
#44423 = DIRECTION ( 'NONE',  ( -0.000000000000000000, 1.000000000000000000, -0.000000000000000000 ) ) ;
#44424 = LINE ( 'NONE', #33347, #40908 ) ;
#44425 = EDGE_LOOP ( 'NONE', ( #14661, #42244, #20296, #8860 ) ) ;
#44426 = ORIENTED_EDGE ( 'NONE', *, *, #3360, .F. ) ;
#44427 = CIRCLE ( 'NONE', #4051, 2.165354330708661568 ) ;
#44429 = PLANE ( 'NONE',  #38918 ) ;
#44428 = CIRCLE ( 'NONE', #13969, 2.244934639244525076 ) ;
#44430 = FACE_OUTER_BOUND ( 'NONE', #46772, .T. ) ;
#44431 = EDGE_LOOP ( 'NONE', ( #32844, #14820, #50882, #48982 ) ) ;
#44432 =( GEOMETRIC_REPRESENTATION_CONTEXT ( 3 ) GLOBAL_UNCERTAINTY_ASSIGNED_CONTEXT ( ( #922 ) ) GLOBAL_UNIT_ASSIGNED_CONTEXT ( ( #37201, #22460, #29699 ) ) REPRESENTATION_CONTEXT ( 'NONE', 'WORKASPACE' ) );
#44433 = VERTEX_POINT ( 'NONE', #50360 ) ;
#44434 = CARTESIAN_POINT ( 'NONE',  ( 1.636583440222563857, 3.346456692913386100, 1.417869535855831975 ) ) ;
#44436 = VERTEX_POINT ( 'NONE', #49859 ) ;
#44435 = EDGE_CURVE ( 'NONE', #39739, #44754, #41913, .T. ) ;
#44437 = VECTOR ( 'NONE', #41903, 39.37007874015748143 ) ;
#44438 = ORIENTED_EDGE ( 'NONE', *, *, #9136, .F. ) ;
#44439 = CARTESIAN_POINT ( 'NONE',  ( 0.5111248625547512026, 1.013073221274083169, 2.540917155971571528 ) ) ;
#44440 = ADVANCED_FACE ( 'NONE', ( #30798 ), #6797, .F. ) ;
#44441 = CARTESIAN_POINT ( 'NONE',  ( -1.091055626815042645, 0.000000000000000000, -1.456692913385822186 ) ) ;
#44442 = EDGE_CURVE ( 'NONE', #34963, #10110, #42410, .T. ) ;
#44443 = EDGE_LOOP ( 'NONE', ( #15479, #35288, #624, #32988 ) ) ;
#44444 = VERTEX_POINT ( 'NONE', #2926 ) ;
#44445 = ORIENTED_EDGE ( 'NONE', *, *, #19706, .F. ) ;
#44446 = LINE ( 'NONE', #21472, #50996 ) ;
#44448 = ORIENTED_EDGE ( 'NONE', *, *, #24053, .T. ) ;
#44447 = EDGE_CURVE ( 'NONE', #44656, #3958, #37800, .T. ) ;
#44449 = ORIENTED_EDGE ( 'NONE', *, *, #47394, .T. ) ;
#44450 = FACE_OUTER_BOUND ( 'NONE', #26895, .T. ) ;
#44451 = LINE ( 'NONE', #33115, #26090 ) ;
#44452 = CARTESIAN_POINT ( 'NONE',  ( -0.5455278134075208785, 3.346456692913386100, 0.6299212598425164567 ) ) ;
#44453 = B_SPLINE_CURVE_WITH_KNOTS ( 'NONE', 3,
 ( #28232, #27724, #8373, #43465 ),
 .UNSPECIFIED., .F., .F.,
 ( 4, 4 ),
 ( 0.1211873102087489551, 0.1625992483279400380 ),
 .UNSPECIFIED. ) ;
#44454 = ORIENTED_EDGE ( 'NONE', *, *, #14073, .T. ) ;
#44455 = DIRECTION ( 'NONE',  ( -0.000000000000000000, 1.000000000000000000, -0.000000000000000000 ) ) ;
#44456 = DIRECTION ( 'NONE',  ( -3.469446951953613696E-16, 0.000000000000000000, -1.000000000000000000 ) ) ;
#44457 = AXIS2_PLACEMENT_3D ( 'NONE', #11939, #27674, #43673 ) ;
#44458 = CARTESIAN_POINT ( 'NONE',  ( 0.000000000000000000, 3.267716535433071279, -1.456692913385822630 ) ) ;
#44459 = EDGE_LOOP ( 'NONE', ( #147, #20322, #29042, #7809 ) ) ;
#44460 = DIRECTION ( 'NONE',  ( 1.000000000000000000, -0.000000000000000000, 0.000000000000000000 ) ) ;
#44461 = DIRECTION ( 'NONE',  ( -0.000000000000000000, 1.000000000000000000, -0.000000000000000000 ) ) ;
#44462 = CARTESIAN_POINT ( 'NONE',  ( -2.122513613727505799, 1.575480814016643638, -0.4339716895473832436 ) ) ;
#44463 = ORIENTED_EDGE ( 'NONE', *, *, #10693, .F. ) ;
#44464 = EDGE_LOOP ( 'NONE', ( #28532, #7423, #12057, #29259 ) ) ;
#44465 = LINE ( 'NONE', #47796, #15539 ) ;
#44466 = VECTOR ( 'NONE', #4405, 39.37007874015748143 ) ;
#44467 = CARTESIAN_POINT ( 'NONE',  ( -1.067222945812429824, 0.5249316497054297148, -1.552631840991228973 ) ) ;
#44468 = LINE ( 'NONE', #33130, #38518 ) ;
#44470 = VECTOR ( 'NONE', #12499, 39.37007874015748143 ) ;
#44469 = DIRECTION ( 'NONE',  ( -1.000000000000000000, -0.000000000000000000, -0.000000000000000000 ) ) ;
#44471 = ORIENTED_EDGE ( 'NONE', *, *, #44080, .T. ) ;
#44472 = VERTEX_POINT ( 'NONE', #43923 ) ;
#44473 = CARTESIAN_POINT ( 'NONE',  ( 2.393386496973425981, 1.651176226490313592, 0.8294036017652782755 ) ) ;
#44474 = VECTOR ( 'NONE', #21024, 39.37007874015748143 ) ;
#44475 = ORIENTED_EDGE ( 'NONE', *, *, #15970, .F. ) ;
#44476 = CARTESIAN_POINT ( 'NONE',  ( 1.363819533518803251, 3.267716535433071279, -2.365849761790805487E-16 ) ) ;
#44477 = PLANE ( 'NONE',  #24277 ) ;
#44478 = LINE ( 'NONE', #48576, #39875 ) ;
#44479 = EDGE_CURVE ( 'NONE', #45444, #32706, #8316, .T. ) ;
#44480 = DIRECTION ( 'NONE',  ( -0.000000000000000000, 0.000000000000000000, 1.000000000000000000 ) ) ;
#44481 = DIRECTION ( 'NONE',  ( 0.6584236824419781309, 0.000000000000000000, 0.7526474967735860000 ) ) ;
#44482 = EDGE_LOOP ( 'NONE', ( #4849, #8536, #26485, #45583 ) ) ;
#44483 = EDGE_CURVE ( 'NONE', #14063, #19810, #31305, .T. ) ;
#44484 = DIRECTION ( 'NONE',  ( 1.734723475976806848E-16, -0.000000000000000000, 1.000000000000000000 ) ) ;
#44485 = DIRECTION ( 'NONE',  ( -0.000000000000000000, 1.000000000000000000, -0.000000000000000000 ) ) ;
#44486 = EDGE_CURVE ( 'NONE', #4657, #30221, #32077, .T. ) ;
#44487 = ORIENTED_EDGE ( 'NONE', *, *, #27278, .F. ) ;
#44488 = CARTESIAN_POINT ( 'NONE',  ( -1.330356682269850044, 1.588168657012911877, -1.747353411991260819 ) ) ;
#44489 = DIRECTION ( 'NONE',  ( -0.000000000000000000, 1.000000000000000000, -0.000000000000000000 ) ) ;
#44490 = DIRECTION ( 'NONE',  ( -0.000000000000000000, 1.000000000000000000, -0.000000000000000000 ) ) ;
#44491 = VECTOR ( 'NONE', #43611, 39.37007874015748143 ) ;
#44492 = ORIENTED_EDGE ( 'NONE', *, *, #44124, .F. ) ;
#44493 = LINE ( 'NONE', #4240, #43125 ) ;
#44494 = LINE ( 'NONE', #9137, #20934 ) ;
#44495 = ORIENTED_EDGE ( 'NONE', *, *, #32270, .F. ) ;
#44496 = CARTESIAN_POINT ( 'NONE',  ( 0.000000000000000000, 3.267716535433071279, 0.4724409448818871482 ) ) ;
#44497 = LINE ( 'NONE', #32654, #35294 ) ;
#44498 = ORIENTED_EDGE ( 'NONE', *, *, #48742, .F. ) ;
#44499 = CARTESIAN_POINT ( 'NONE',  ( 0.000000000000000000, 3.346456692913386100, 0.000000000000000000 ) ) ;
#44500 = VECTOR ( 'NONE', #42508, 39.37007874015748143 ) ;
#44501 = DIRECTION ( 'NONE',  ( 1.000000000000000000, 0.000000000000000000, 0.000000000000000000 ) ) ;
#44502 = ADVANCED_FACE ( 'NONE', ( #39043 ), #46998, .F. ) ;
#44503 = CARTESIAN_POINT ( 'NONE',  ( -0.2727639067037608278, 0.000000000000000000, -0.3543307086614175816 ) ) ;
#44504 = CARTESIAN_POINT ( 'NONE',  ( 0.000000000000000000, 3.267716535433071279, 0.000000000000000000 ) ) ;
#44505 = CARTESIAN_POINT ( 'NONE',  ( -2.014664160120487768, 1.577208220393157223, -0.8075893616760145832 ) ) ;
#44506 = ORIENTED_EDGE ( 'NONE', *, *, #33623, .F. ) ;
#44507 = ORIENTED_EDGE ( 'NONE', *, *, #18329, .F. ) ;
#44508 = LINE ( 'NONE', #9152, #41348 ) ;
#44509 = DIRECTION ( 'NONE',  ( -0.000000000000000000, 1.000000000000000000, -0.000000000000000000 ) ) ;
#44510 = ADVANCED_FACE ( 'NONE', ( #43412 ), #18138, .T. ) ;
#44511 = ORIENTED_EDGE ( 'NONE', *, *, #48589, .T. ) ;
#44512 = LINE ( 'NONE', #28252, #32519 ) ;
#44513 = DIRECTION ( 'NONE',  ( -1.000000000000000000, 0.000000000000000000, 1.734723475976806848E-16 ) ) ;
#44514 = CIRCLE ( 'NONE', #7411, 2.106299212598425008 ) ;
#44515 = CARTESIAN_POINT ( 'NONE',  ( -1.735196932040237394, 1.680109596358665636, 1.320828101803479315 ) ) ;
#44516 = CARTESIAN_POINT ( 'NONE',  ( 2.889674983507178219, 5.905511811023623991, -0.6090712660037602699 ) ) ;
#44517 = VERTEX_POINT ( 'NONE', #27414 ) ;
#44518 = ORIENTED_EDGE ( 'NONE', *, *, #39709, .T. ) ;
#44519 = PLANE ( 'NONE',  #20483 ) ;
#44520 = LINE ( 'NONE', #31906, #26631 ) ;
#44521 = CARTESIAN_POINT ( 'NONE',  ( 0.000000000000000000, 6.692913385826772199, 0.000000000000000000 ) ) ;
#44522 = VERTEX_POINT ( 'NONE', #28179 ) ;
#44523 = PLANE ( 'NONE',  #30656 ) ;
#44524 = FACE_BOUND ( 'NONE', #9264, .T. ) ;
#44525 = ORIENTED_EDGE ( 'NONE', *, *, #47753, .T. ) ;
#44526 = CYLINDRICAL_SURFACE ( 'NONE', #50427, 2.165354330708661568 ) ;
#44527 = ORIENTED_EDGE ( 'NONE', *, *, #50951, .F. ) ;
#44528 = EDGE_LOOP ( 'NONE', ( #21695, #7081, #703, #47361 ) ) ;
#44529 = CARTESIAN_POINT ( 'NONE',  ( -2.356851836761542529, 1.575923956308009632, -0.5884142439354561605 ) ) ;
#44530 = ORIENTED_EDGE ( 'NONE', *, *, #38808, .T. ) ;
#44531 = CARTESIAN_POINT ( 'NONE',  ( 2.168245791271197209, 1.753049777144058297, -2.004968704497248844 ) ) ;
#44532 = ORIENTED_EDGE ( 'NONE', *, *, #39249, .T. ) ;
#44533 = FACE_OUTER_BOUND ( 'NONE', #11544, .T. ) ;
#44534 = CARTESIAN_POINT ( 'NONE',  ( 0.000000000000000000, 0.000000000000000000, 0.000000000000000000 ) ) ;
#44535 = CARTESIAN_POINT ( 'NONE',  ( 1.807908292590730825, 0.5224481969157015460, 1.378813476911973535 ) ) ;
#44536 = AXIS2_PLACEMENT_3D ( 'NONE', #27775, #24169, #43258 ) ;
#44537 = VECTOR ( 'NONE', #33129, 39.37007874015748143 ) ;
#44538 = DIRECTION ( 'NONE',  ( -0.000000000000000000, 0.000000000000000000, 1.000000000000000000 ) ) ;
#44539 = EDGE_CURVE ( 'NONE', #2307, #12681, #17567, .T. ) ;
#44540 = CARTESIAN_POINT ( 'NONE',  ( 0.2841802383804452603, 0.03247133209088205741, 1.841575167587790718 ) ) ;
#44541 = LINE ( 'NONE', #4551, #16288 ) ;
#44542 = ORIENTED_EDGE ( 'NONE', *, *, #26840, .T. ) ;
#44543 = EDGE_CURVE ( 'NONE', #29386, #40287, #16060, .T. ) ;
#44544 = CARTESIAN_POINT ( 'NONE',  ( 1.091055626815042645, 0.000000000000000000, 1.259842519685033357 ) ) ;
#44545 = AXIS2_PLACEMENT_3D ( 'NONE', #23741, #23232, #4381 ) ;
#44546 = LINE ( 'NONE', #45298, #1756 ) ;
#44547 = ADVANCED_FACE ( 'NONE', ( #35432 ), #49, .F. ) ;
#44548 = ORIENTED_EDGE ( 'NONE', *, *, #17551, .F. ) ;
#44549 = FACE_OUTER_BOUND ( 'NONE', #6983, .T. ) ;
#44550 = CARTESIAN_POINT ( 'NONE',  ( 1.232620761116212771, 5.905511811023623991, -1.780282403660734980 ) ) ;
#44551 = ORIENTED_EDGE ( 'NONE', *, *, #5451, .F. ) ;
#44552 = LINE ( 'NONE', #12823, #27885 ) ;
#44553 = FACE_OUTER_BOUND ( 'NONE', #4344, .T. ) ;
#44554 = CARTESIAN_POINT ( 'NONE',  ( -2.044241703397525978, 1.205361022782829114E-17, -0.7159595814952911530 ) ) ;
#44555 = EDGE_LOOP ( 'NONE', ( #32191, #24464, #37855, #16720 ) ) ;
#44556 = DIRECTION ( 'NONE',  ( 0.04486483035050446017, 0.000000000000000000, 0.9989930665413151445 ) ) ;
#44557 = ORIENTED_EDGE ( 'NONE', *, *, #46001, .F. ) ;
#44558 = FACE_BOUND ( 'NONE', #8041, .T. ) ;
#44559 = DIRECTION ( 'NONE',  ( -3.469446951953613696E-16, 0.000000000000000000, -1.000000000000000000 ) ) ;
#44560 = DIRECTION ( 'NONE',  ( 0.000000000000000000, 1.000000000000000000, 0.000000000000000000 ) ) ;
#44561 = ADVANCED_FACE ( 'NONE', ( #16318 ), #15556, .T. ) ;
#44562 = DIRECTION ( 'NONE',  ( -1.000000000000000000, 0.000000000000000000, 0.000000000000000000 ) ) ;
#44563 = ORIENTED_EDGE ( 'NONE', *, *, #42791, .F. ) ;
#44564 = EDGE_LOOP ( 'NONE', ( #10724, #22233, #41070, #11645 ) ) ;
#44565 = DIRECTION ( 'NONE',  ( -3.469446951953613696E-16, 0.000000000000000000, -1.000000000000000000 ) ) ;
#44566 = EDGE_LOOP ( 'NONE', ( #32275, #18892, #5076, #42611 ) ) ;
#44567 = EDGE_CURVE ( 'NONE', #24292, #39823, #16579, .T. ) ;
#44568 = LINE ( 'NONE', #5344, #43356 ) ;
#44569 = VERTEX_POINT ( 'NONE', #15796 ) ;
#44570 = VECTOR ( 'NONE', #16495, 39.37007874015748854 ) ;
#44571 = CARTESIAN_POINT ( 'NONE',  ( -1.636583440222563635, 0.000000000000000000, 1.259842519685033357 ) ) ;
#44572 = VECTOR ( 'NONE', #28051, 39.37007874015748143 ) ;
#44573 = EDGE_LOOP ( 'NONE', ( #2559, #26509, #15692, #49129 ) ) ;
#44574 = LINE ( 'NONE', #8713, #33222 ) ;
#44575 = CARTESIAN_POINT ( 'NONE',  ( 0.1250607540065018508, 1.205361022782829114E-17, -1.938545675207280272 ) ) ;
#44576 = ORIENTED_EDGE ( 'NONE', *, *, #13629, .T. ) ;
#44577 = FACE_OUTER_BOUND ( 'NONE', #26171, .T. ) ;
#44578 = ORIENTED_EDGE ( 'NONE', *, *, #34174, .F. ) ;
#44579 = CONICAL_SURFACE ( 'NONE', #17398, 2.246510896728926010, 0.01601546068027819014 ) ;
#44580 = ORIENTED_EDGE ( 'NONE', *, *, #8718, .T. ) ;
#44581 = EDGE_CURVE ( 'NONE', #30461, #11143, #31820, .T. ) ;
#44582 = ORIENTED_EDGE ( 'NONE', *, *, #48477, .T. ) ;
#44583 = EDGE_LOOP ( 'NONE', ( #5199, #20, #7277, #42937 ) ) ;
#44584 = CARTESIAN_POINT ( 'NONE',  ( -0.2727639067037608278, 0.000000000000000000, 0.2755905511810995412 ) ) ;
#44585 = CARTESIAN_POINT ( 'NONE',  ( 0.000000000000000000, 3.267716535433071279, -0.9448818897637762948 ) ) ;
#44586 = ORIENTED_EDGE ( 'NONE', *, *, #761, .F. ) ;
#44587 = CARTESIAN_POINT ( 'NONE',  ( 0.1735763337869204448, 1.714436956846898896, -2.477597915911436299 ) ) ;
#44588 = VERTEX_POINT ( 'NONE', #12186 ) ;
#44589 = LINE ( 'NONE', #23964, #35967 ) ;
#44590 = DIRECTION ( 'NONE',  ( -0.9998717552508122886, -0.01601477604151182316, 0.000000000000000000 ) ) ;
#44591 = VERTEX_POINT ( 'NONE', #42904 ) ;
#44592 = CARTESIAN_POINT ( 'NONE',  ( 0.000000000000000000, 3.267716535433071279, -1.161035397307311917E-15 ) ) ;
#44593 = CARTESIAN_POINT ( 'NONE',  ( -0.5455278134075208785, 0.000000000000000000, 1.889763779527550369 ) ) ;
#44594 = CARTESIAN_POINT ( 'NONE',  ( 2.278027606577265107, 1.645963535160160696, -0.4694667435916627385 ) ) ;
#44595 = LINE ( 'NONE', #29118, #23321 ) ;
#44596 = DIRECTION ( 'NONE',  ( 1.000000000000000000, 0.000000000000000000, 0.000000000000000000 ) ) ;
#44597 = LINE ( 'NONE', #31993, #15747 ) ;
#44598 = EDGE_CURVE ( 'NONE', #31898, #13220, #12347, .T. ) ;
#44599 = VECTOR ( 'NONE', #4873, 39.37007874015748143 ) ;
#44600 = VECTOR ( 'NONE', #1341, 39.37007874015748143 ) ;
#44601 = DIRECTION ( 'NONE',  ( 0.5773502691896256200, 0.5773502691896271743, -0.5773502691896242878 ) ) ;
#44602 = EDGE_CURVE ( 'NONE', #1849, #39003, #47767, .T. ) ;
#44603 = ORIENTED_EDGE ( 'NONE', *, *, #23166, .F. ) ;
#44604 = DIRECTION ( 'NONE',  ( 1.000000000000000000, 0.000000000000000000, 0.000000000000000000 ) ) ;
#44605 = EDGE_CURVE ( 'NONE', #4372, #46764, #2748, .T. ) ;
#44606 = DIRECTION ( 'NONE',  ( 0.000000000000000000, 0.000000000000000000, 1.000000000000000000 ) ) ;
#44607 = EDGE_LOOP ( 'NONE', ( #24601, #15730, #40004, #36158 ) ) ;
#44608 = LINE ( 'NONE', #37148, #10255 ) ;
#44609 = CONICAL_SURFACE ( 'NONE', #28957, 3.483074324928249421, 1.244861948955335196 ) ;
#44610 = ORIENTED_EDGE ( 'NONE', *, *, #26274, .T. ) ;
#44611 = DIRECTION ( 'NONE',  ( 1.000000000000000000, 0.000000000000000000, 0.000000000000000000 ) ) ;
#44612 = CARTESIAN_POINT ( 'NONE',  ( 0.5455278134075212115, 0.000000000000000000, 0.6299212598425161236 ) ) ;
#44613 = VECTOR ( 'NONE', #46869, 39.37007874015748143 ) ;
#44614 = CARTESIAN_POINT ( 'NONE',  ( 0.5455278134075212115, 3.346456692913386100, 0.3149606299212576177 ) ) ;
#44615 = CARTESIAN_POINT ( 'NONE',  ( -2.182111253630085734, 0.000000000000000000, -0.8267716535433052849 ) ) ;
#44616 = EDGE_CURVE ( 'NONE', #11168, #25127, #27666, .T. ) ;
#44617 = CARTESIAN_POINT ( 'NONE',  ( 0.5905511811023621549, 0.000000000000000000, -4.133858267716536083 ) ) ;
#44618 = VERTEX_POINT ( 'NONE', #19915 ) ;
#44619 = CARTESIAN_POINT ( 'NONE',  ( -1.083598637574820334, 1.702374950942735499, 2.747180975113330259 ) ) ;
#44620 = FACE_BOUND ( 'NONE', #6793, .T. ) ;
#44621 = ORIENTED_EDGE ( 'NONE', *, *, #15834, .T. ) ;
#44622 = PLANE ( 'NONE',  #48487 ) ;
#44623 = ORIENTED_EDGE ( 'NONE', *, *, #42116, .F. ) ;
#44624 = CARTESIAN_POINT ( 'NONE',  ( 1.636583440222563857, 3.346456692913386100, -0.5118110236220471121 ) ) ;
#44625 = CARTESIAN_POINT ( 'NONE',  ( -1.363819533518803029, 0.000000000000000000, 0.2755905511810996522 ) ) ;
#44626 = B_SPLINE_CURVE_WITH_KNOTS ( 'NONE', 3,
 ( #14660, #2532, #46125, #10780 ),
 .UNSPECIFIED., .F., .F.,
 ( 4, 4 ),
 ( 1.995997118274627782E-07, 0.001216554165443645879 ),
 .UNSPECIFIED. ) ;
#44627 = EDGE_CURVE ( 'NONE', #26908, #49287, #36042, .T. ) ;
#44628 = DIRECTION ( 'NONE',  ( 0.000000000000000000, 0.000000000000000000, -1.000000000000000000 ) ) ;
#44629 = CARTESIAN_POINT ( 'NONE',  ( -2.494510946366233384, 1.676303183382823025, -1.012685720897419150 ) ) ;
#44630 = ORIENTED_EDGE ( 'NONE', *, *, #23973, .F. ) ;
#44631 = ORIENTED_EDGE ( 'NONE', *, *, #46300, .T. ) ;
#44632 = LINE ( 'NONE', #5413, #35885 ) ;
#44633 = CARTESIAN_POINT ( 'NONE',  ( -2.100227814008681637, 1.588094595312779855, -2.076109931251943763 ) ) ;
#44634 = FACE_BOUND ( 'NONE', #25961, .T. ) ;
#44635 = EDGE_LOOP ( 'NONE', ( #48203, #37795, #38578, #40672 ) ) ;
#44636 = ADVANCED_FACE ( 'NONE', ( #8311 ), #12960, .F. ) ;
#44637 = VECTOR ( 'NONE', #18469, 39.37007874015748143 ) ;
#44638 = VECTOR ( 'NONE', #1163, 39.37007874015748143 ) ;
#44639 = CARTESIAN_POINT ( 'NONE',  ( -0.6214413264104945434, 3.267716535433071279, -1.732283464566922726 ) ) ;
#44640 = CARTESIAN_POINT ( 'NONE',  ( -1.053808008129011320, 3.267716535433071279, 2.204724409448808764 ) ) ;
#44641 = ORIENTED_EDGE ( 'NONE', *, *, #21549, .T. ) ;
#44642 = DIRECTION ( 'NONE',  ( -1.000000000000000000, 0.000000000000000000, 0.000000000000000000 ) ) ;
#44643 = VECTOR ( 'NONE', #46825, 39.37007874015748143 ) ;
#44644 = CARTESIAN_POINT ( 'NONE',  ( -0.8182917201112819283, 0.000000000000000000, 2.047244094488179567 ) ) ;
#44645 = EDGE_CURVE ( 'NONE', #25916, #25164, #28853, .T. ) ;
#44646 = EDGE_LOOP ( 'NONE', ( #23790, #24767, #15636, #154 ) ) ;
#44647 = ORIENTED_EDGE ( 'NONE', *, *, #7946, .T. ) ;
#44648 = AXIS2_PLACEMENT_3D ( 'NONE', #8461, #31706, #11569 ) ;
#44650 = EDGE_CURVE ( 'NONE', #4308, #41410, #36457, .T. ) ;
#44649 = ORIENTED_EDGE ( 'NONE', *, *, #9634, .T. ) ;
#44651 = CARTESIAN_POINT ( 'NONE',  ( 1.636583440222563857, 3.267716535433071279, -2.839019714148966584E-16 ) ) ;
#44652 = VECTOR ( 'NONE', #9899, 39.37007874015748143 ) ;
#44653 = DIRECTION ( 'NONE',  ( -3.469446951953613696E-16, 0.000000000000000000, -1.000000000000000000 ) ) ;
#44654 = CARTESIAN_POINT ( 'NONE',  ( 0.1067246931122726866, 0.02962905676920215767, 0.000000000000000000 ) ) ;
#44655 = DIRECTION ( 'NONE',  ( 0.01601477604151182663, -0.9998717552508123996, 0.000000000000000000 ) ) ;
#44656 = VERTEX_POINT ( 'NONE', #41344 ) ;
#44657 = ORIENTED_EDGE ( 'NONE', *, *, #41925, .T. ) ;
#44658 = CARTESIAN_POINT ( 'NONE',  ( -1.636583440222563635, 3.346456692913386100, 0.3149606299212578953 ) ) ;
#44659 = FACE_OUTER_BOUND ( 'NONE', #30879, .T. ) ;
#44660 = DIRECTION ( 'NONE',  ( 1.734723475976806848E-16, 0.000000000000000000, 1.000000000000000000 ) ) ;
#44661 = CARTESIAN_POINT ( 'NONE',  ( 0.3734705886643994721, 2.755905511811024056, -0.02018660888377523527 ) ) ;
#44662 = CARTESIAN_POINT ( 'NONE',  ( -1.712496953225537188, 3.267716535433071279, 0.5905511811023582691 ) ) ;
#44663 = EDGE_CURVE ( 'NONE', #19974, #50372, #21727, .T. ) ;
#44664 = DIRECTION ( 'NONE',  ( 1.734723475976806848E-16, -0.000000000000000000, 1.000000000000000000 ) ) ;
#44665 = EDGE_CURVE ( 'NONE', #2713, #26706, #40836, .T. ) ;
#44666 = EDGE_CURVE ( 'NONE', #18530, #924, #24830, .T. ) ;
#44667 = DIRECTION ( 'NONE',  ( -3.986037398843765983E-20, -1.000000000000000000, -1.160734090543304660E-16 ) ) ;
#44668 = VERTEX_POINT ( 'NONE', #44684 ) ;
#44669 = LINE ( 'NONE', #45426, #9412 ) ;
#44670 = LINE ( 'NONE', #9321, #25239 ) ;
#44671 = ORIENTED_EDGE ( 'NONE', *, *, #36085, .F. ) ;
#44672 = ORIENTED_EDGE ( 'NONE', *, *, #42591, .F. ) ;
#44673 = DIRECTION ( 'NONE',  ( 0.000000000000000000, -1.000000000000000000, 0.000000000000000000 ) ) ;
#44674 = VECTOR ( 'NONE', #44460, 39.37007874015748143 ) ;
#44675 = CARTESIAN_POINT ( 'NONE',  ( 0.5455278134075217666, 3.346456692913386100, 2.034427629037600660 ) ) ;
#44676 = EDGE_LOOP ( 'NONE', ( #24689, #35110, #4341, #25087 ) ) ;
#44677 = AXIS2_PLACEMENT_3D ( 'NONE', #44883, #44628, #11682 ) ;
#44678 = ORIENTED_EDGE ( 'NONE', *, *, #38034, .T. ) ;
#44679 = CARTESIAN_POINT ( 'NONE',  ( -1.712496953225537188, 3.346456692913386100, 0.4724409448818871482 ) ) ;
#44680 = CONICAL_SURFACE ( 'NONE', #45527, 3.483074324928249421, 1.244861948955335196 ) ;
#44681 = VERTEX_POINT ( 'NONE', #5205 ) ;
#44682 = VECTOR ( 'NONE', #43279, 39.37007874015748143 ) ;
#44683 = LINE ( 'NONE', #29722, #31766 ) ;
#44684 = CARTESIAN_POINT ( 'NONE',  ( 2.182111253630085290, 3.267716535433071279, -0.3149606299212596716 ) ) ;
#44685 = EDGE_CURVE ( 'NONE', #24976, #18933, #28947, .T. ) ;
#44686 = VERTEX_POINT ( 'NONE', #1073 ) ;
#44687 = VERTEX_POINT ( 'NONE', #9336 ) ;
#44688 = ORIENTED_EDGE ( 'NONE', *, *, #16757, .F. ) ;
#44689 = FACE_OUTER_BOUND ( 'NONE', #49141, .T. ) ;
#44690 = ORIENTED_EDGE ( 'NONE', *, *, #27335, .T. ) ;
#44691 = ORIENTED_EDGE ( 'NONE', *, *, #13409, .F. ) ;
#44692 = DIRECTION ( 'NONE',  ( 1.000000000000000000, -0.000000000000000000, 0.000000000000000000 ) ) ;
#44693 = DIRECTION ( 'NONE',  ( 0.000000000000000000, 1.000000000000000000, 0.000000000000000000 ) ) ;
#44694 = DIRECTION ( 'NONE',  ( 1.734723475976806848E-16, -0.000000000000000000, 1.000000000000000000 ) ) ;
#44695 = EDGE_CURVE ( 'NONE', #14934, #17666, #25086, .T. ) ;
#44696 = ORIENTED_EDGE ( 'NONE', *, *, #13225, .F. ) ;
#44697 = EDGE_CURVE ( 'NONE', #47149, #46941, #45188, .T. ) ;
#44698 = LINE ( 'NONE', #25103, #26309 ) ;
#44699 = CARTESIAN_POINT ( 'NONE',  ( 0.1155636338427008941, -0.5222242541845523167, 0.000000000000000000 ) ) ;
#44700 = LINE ( 'NONE', #9612, #22074 ) ;
#44701 = EDGE_CURVE ( 'NONE', #46419, #2713, #25336, .T. ) ;
#44702 = ORIENTED_EDGE ( 'NONE', *, *, #4071, .T. ) ;
#44703 = DIRECTION ( 'NONE',  ( 0.000000000000000000, 1.000000000000000000, -0.000000000000000000 ) ) ;
#44704 = DIRECTION ( 'NONE',  ( -0.000000000000000000, 1.000000000000000000, -0.000000000000000000 ) ) ;
#44705 = LINE ( 'NONE', #9358, #38978 ) ;
#44706 = ORIENTED_EDGE ( 'NONE', *, *, #3587, .F. ) ;
#44707 = VERTEX_POINT ( 'NONE', #1591 ) ;
#44708 = DIRECTION ( 'NONE',  ( 0.000000000000000000, 0.000000000000000000, -1.000000000000000000 ) ) ;
#44710 = AXIS2_PLACEMENT_3D ( 'NONE', #40539, #5164, #24533 ) ;
#44709 = CARTESIAN_POINT ( 'NONE',  ( -1.091055626815042201, 3.346456692913386100, 0.9448818897637749625 ) ) ;
#44711 = LINE ( 'NONE', #25115, #16249 ) ;
#44712 = CARTESIAN_POINT ( 'NONE',  ( -0.7328193673159020260, 1.696164507524817511, 2.092647490920610309 ) ) ;
#44713 = EDGE_LOOP ( 'NONE', ( #29875, #4958, #30493, #47629 ) ) ;
#44714 = ORIENTED_EDGE ( 'NONE', *, *, #21064, .T. ) ;
#44715 = VECTOR ( 'NONE', #31130, 39.37007874015748143 ) ;
#44716 = CARTESIAN_POINT ( 'NONE',  ( 1.363819533518803251, 3.267716535433071279, -0.7874015748031473194 ) ) ;
#44717 = VECTOR ( 'NONE', #40518, 39.37007874015748143 ) ;
#44718 = ORIENTED_EDGE ( 'NONE', *, *, #29460, .T. ) ;
#44719 = PLANE ( 'NONE',  #44244 ) ;
#44720 = LINE ( 'NONE', #25627, #46501 ) ;
#44721 = AXIS2_PLACEMENT_3D ( 'NONE', #14013, #9886, #25121 ) ;
#44722 = ADVANCED_FACE ( 'NONE', ( #48024 ), #24576, .F. ) ;
#44723 = B_SPLINE_CURVE_WITH_KNOTS ( 'NONE', 3,
 ( #37752, #33121, #13992, #2375 ),
 .UNSPECIFIED., .F., .F.,
 ( 4, 4 ),
 ( 0.1211775127643062860, 0.1625894504277921315 ),
 .UNSPECIFIED. ) ;
#44724 = VECTOR ( 'NONE', #1048, 39.37007874015748143 ) ;
#44725 = ADVANCED_FACE ( 'NONE', ( #4951 ), #48788, .F. ) ;
#44726 = ADVANCED_FACE ( 'NONE', ( #28433 ), #9594, .F. ) ;
#44727 = CARTESIAN_POINT ( 'NONE',  ( -1.560823827823494936, 0.000000000000000000, 0.8212364767474445992 ) ) ;
#44728 = LINE ( 'NONE', #49083, #6298 ) ;
#44729 = FACE_OUTER_BOUND ( 'NONE', #882, .T. ) ;
#44730 = EDGE_LOOP ( 'NONE', ( #1684, #6004, #35062, #21040 ) ) ;
#44731 = CARTESIAN_POINT ( 'NONE',  ( 0.000000000000000000, 0.5905511811023621549, -1.062992125984252079 ) ) ;
#44732 = EDGE_CURVE ( 'NONE', #6991, #38732, #16834, .T. ) ;
#44733 = B_SPLINE_CURVE_WITH_KNOTS ( 'NONE', 3,
 ( #29741, #49820, #22002, #49566 ),
 .UNSPECIFIED., .F., .F.,
 ( 4, 4 ),
 ( 2.271247881248620160E-07, 0.002500295357758199402 ),
 .UNSPECIFIED. ) ;
#44734 = DIRECTION ( 'NONE',  ( 1.734723475976806848E-16, -0.000000000000000000, 1.000000000000000000 ) ) ;
#44735 = ORIENTED_EDGE ( 'NONE', *, *, #46224, .T. ) ;
#44736 = CARTESIAN_POINT ( 'NONE',  ( 2.106197740627112402, 3.346456692913386100, 0.7874015748031456541 ) ) ;
#44737 = CARTESIAN_POINT ( 'NONE',  ( 0.5455278134075212115, 3.346456692913386100, -0.6299212598425181220 ) ) ;
#44738 = CARTESIAN_POINT ( 'NONE',  ( -2.121605289024800722, 3.346456692913386100, 0.4330708661417290162 ) ) ;
#44739 = EDGE_LOOP ( 'NONE', ( #12802, #21930, #38713, #26382 ) ) ;
#44740 = DIRECTION ( 'NONE',  ( -0.000000000000000000, -1.000000000000000000, 0.000000000000000000 ) ) ;
#44741 = B_SPLINE_CURVE_WITH_KNOTS ( 'NONE', 3,
 ( #42484, #26980, #50677, #3502 ),
 .UNSPECIFIED., .F., .F.,
 ( 4, 4 ),
 ( 0.1211873102087489551, 0.1625992483279400380 ),
 .UNSPECIFIED. ) ;
#44742 = CARTESIAN_POINT ( 'NONE',  ( 2.491402175429653809, 1.458524810485662959, -1.585592796919505609 ) ) ;
#44743 = ORIENTED_EDGE ( 'NONE', *, *, #22760, .T. ) ;
#44744 = CARTESIAN_POINT ( 'NONE',  ( 0.000000000000000000, 3.267716535433071279, 0.000000000000000000 ) ) ;
#44745 = CARTESIAN_POINT ( 'NONE',  ( -2.258024766633058622, 3.346456692913386100, -0.03937007874015881204 ) ) ;
#44746 = ORIENTED_EDGE ( 'NONE', *, *, #49140, .T. ) ;
#44747 = FACE_OUTER_BOUND ( 'NONE', #40949, .T. ) ;
#44748 = CARTESIAN_POINT ( 'NONE',  ( 0.6770709118595397147, 1.627661423436544519, -2.638295496325671063 ) ) ;
#44749 = DIRECTION ( 'NONE',  ( 0.000000000000000000, 0.000000000000000000, -1.000000000000000000 ) ) ;
#44750 = PLANE ( 'NONE',  #1257 ) ;
#44751 = CARTESIAN_POINT ( 'NONE',  ( 3.927031490892378253E-16, 0.000000000000000000, 2.007874015748021268 ) ) ;
#44752 = VECTOR ( 'NONE', #7573, 39.37007874015748143 ) ;
#44753 = ORIENTED_EDGE ( 'NONE', *, *, #8929, .F. ) ;
#44754 = VERTEX_POINT ( 'NONE', #1846 ) ;
#44755 = DIRECTION ( 'NONE',  ( -0.000000000000000000, 1.000000000000000000, -0.000000000000000000 ) ) ;
#44756 = DIRECTION ( 'NONE',  ( 0.000000000000000000, 0.000000000000000000, -1.000000000000000000 ) ) ;
#44757 = ORIENTED_EDGE ( 'NONE', *, *, #28998, .T. ) ;
#44758 = DIRECTION ( 'NONE',  ( -3.469446951953613696E-16, 0.000000000000000000, -1.000000000000000000 ) ) ;
#44759 = DIRECTION ( 'NONE',  ( -3.469446951953613696E-16, 0.000000000000000000, -1.000000000000000000 ) ) ;
#44760 = CARTESIAN_POINT ( 'NONE',  ( -1.556712866041156662, 1.548291375251236834, 2.509548638715847435 ) ) ;
#44761 = AXIS2_PLACEMENT_3D ( 'NONE', #42070, #17815, #37448 ) ;
#44762 = DIRECTION ( 'NONE',  ( -0.6579387259397136978, 0.000000000000000000, 0.7530714660036097463 ) ) ;
#44763 = VECTOR ( 'NONE', #29955, 39.37007874015748143 ) ;
#44764 = EDGE_LOOP ( 'NONE', ( #28726, #48455, #692, #24336 ) ) ;
#44765 = EDGE_LOOP ( 'NONE', ( #41142, #14725, #19245, #23503 ) ) ;
#44766 = EDGE_CURVE ( 'NONE', #448, #31173, #33357, .T. ) ;
#44767 = LINE ( 'NONE', #1671, #10610 ) ;
#44768 = DIRECTION ( 'NONE',  ( 0.000000000000000000, -0.000000000000000000, -1.000000000000000000 ) ) ;
#44769 = DIRECTION ( 'NONE',  ( -3.469446951953613696E-16, 0.000000000000000000, -1.000000000000000000 ) ) ;
#44770 = ORIENTED_EDGE ( 'NONE', *, *, #41350, .T. ) ;
#44771 = LINE ( 'NONE', #36286, #15784 ) ;
#44772 = EDGE_CURVE ( 'NONE', #36107, #1640, #26386, .T. ) ;
#44773 = FACE_BOUND ( 'NONE', #28453, .T. ) ;
#44774 = VECTOR ( 'NONE', #29834, 39.37007874015748143 ) ;
#44775 = ORIENTED_EDGE ( 'NONE', *, *, #2303, .T. ) ;
#44776 = DIRECTION ( 'NONE',  ( 1.000000000000000000, 0.000000000000000000, 0.000000000000000000 ) ) ;
#44777 = EDGE_LOOP ( 'NONE', ( #23889, #35867, #18281, #14125 ) ) ;
#44778 = VERTEX_POINT ( 'NONE', #50053 ) ;
#44779 = DIRECTION ( 'NONE',  ( -1.000000000000000000, -0.000000000000000000, -0.000000000000000000 ) ) ;
#44780 = ORIENTED_EDGE ( 'NONE', *, *, #32146, .T. ) ;
#44781 = FACE_OUTER_BOUND ( 'NONE', #23018, .T. ) ;
#44782 = CARTESIAN_POINT ( 'NONE',  ( -0.5455278134075214336, 0.000000000000000000, -0.8267716535433049518 ) ) ;
#44783 = EDGE_LOOP ( 'NONE', ( #27519, #23121, #6379, #20846 ) ) ;
#44784 = EDGE_CURVE ( 'NONE', #42119, #13544, #44514, .T. ) ;
#44785 = LENGTH_MEASURE_WITH_UNIT ( LENGTH_MEASURE( 0.02539999999999999897 ), #13571 );
#44786 = CARTESIAN_POINT ( 'NONE',  ( 0.8182917201112819283, 0.000000000000000000, 0.9055118110236164419 ) ) ;
#44787 = DIRECTION ( 'NONE',  ( -0.000000000000000000, 0.000000000000000000, 1.000000000000000000 ) ) ;
#44788 = EDGE_CURVE ( 'NONE', #8152, #12919, #3365, .T. ) ;
#44789 = DIRECTION ( 'NONE',  ( 1.734723475976806848E-16, -0.000000000000000000, 1.000000000000000000 ) ) ;
#44790 = EDGE_CURVE ( 'NONE', #42413, #25659, #34112, .T. ) ;
#44791 = AXIS2_PLACEMENT_3D ( 'NONE', #4907, #43106, #35132 ) ;
#44792 = CARTESIAN_POINT ( 'NONE',  ( 0.2727639067037610499, 0.000000000000000000, 2.047244094488179567 ) ) ;
#44793 = CARTESIAN_POINT ( 'NONE',  ( -2.145573069125249699, 1.587379441712122086, -2.028682512702774332 ) ) ;
#44794 = ORIENTED_EDGE ( 'NONE', *, *, #33754, .T. ) ;
#44795 = PLANE ( 'NONE',  #25809 ) ;
#44796 = EDGE_CURVE ( 'NONE', #6021, #38746, #37987, .T. ) ;
#44797 = EDGE_CURVE ( 'NONE', #35652, #18042, #4034, .T. ) ;
#44798 = LINE ( 'NONE', #10213, #15781 ) ;
#44799 = CONICAL_SURFACE ( 'NONE', #10214, 1.850107469027523210, 0.6386652850508578450 ) ;
#44800 = VECTOR ( 'NONE', #46115, 39.37007874015748143 ) ;
#44801 = ORIENTED_EDGE ( 'NONE', *, *, #27102, .T. ) ;
#44802 = CARTESIAN_POINT ( 'NONE',  ( 1.958513403246152640, 1.640845930445798073, -1.233835998176425308 ) ) ;
#44804 = CARTESIAN_POINT ( 'NONE',  ( -2.100227814008681637, 0.000000000000000000, -2.076109931251943763 ) ) ;
#44803 = B_SPLINE_CURVE_WITH_KNOTS ( 'NONE', 3,
 ( #30709, #39206, #46667, #30460 ),
 .UNSPECIFIED., .F., .F.,
 ( 4, 4 ),
 ( 0.01092706744755390577, 0.03073589647694806304 ),
 .UNSPECIFIED. ) ;
#44805 = EDGE_LOOP ( 'NONE', ( #49086, #28354, #14421, #40544 ) ) ;
#44806 = DIRECTION ( 'NONE',  ( 0.7071067811865466846, 0.000000000000000000, 0.7071067811865483499 ) ) ;
#44807 = CARTESIAN_POINT ( 'NONE',  ( -0.8942052331142552601, 3.267716535433071279, -1.259842519685034690 ) ) ;
#44808 = LINE ( 'NONE', #45557, #11202 ) ;
#44809 = VECTOR ( 'NONE', #26211, 39.37007874015748143 ) ;
#44810 = VERTEX_POINT ( 'NONE', #49546 ) ;
#44811 = DIRECTION ( 'NONE',  ( -0.000000000000000000, 1.000000000000000000, -0.000000000000000000 ) ) ;
#44812 = ORIENTED_EDGE ( 'NONE', *, *, #29200, .F. ) ;
#44813 = FACE_BOUND ( 'NONE', #45255, .T. ) ;
#44814 = CARTESIAN_POINT ( 'NONE',  ( 0.5455278134075212115, 3.267716535433071279, 0.6299212598425161236 ) ) ;
#44815 = DIRECTION ( 'NONE',  ( 1.000000000000000000, 0.000000000000000000, -3.469446951953613696E-16 ) ) ;
#44816 = LINE ( 'NONE', #20314, #32598 ) ;
#44817 = ORIENTED_EDGE ( 'NONE', *, *, #6210, .T. ) ;
#44818 = VERTEX_POINT ( 'NONE', #14226 ) ;
#44819 = FACE_OUTER_BOUND ( 'NONE', #20590, .T. ) ;
#44820 = ORIENTED_EDGE ( 'NONE', *, *, #12182, .F. ) ;
#44821 = LINE ( 'NONE', #25222, #35979 ) ;
#44822 = ORIENTED_EDGE ( 'NONE', *, *, #14715, .F. ) ;
#44823 = FACE_OUTER_BOUND ( 'NONE', #15108, .T. ) ;
#44824 = ORIENTED_EDGE ( 'NONE', *, *, #8200, .T. ) ;
#44825 = CARTESIAN_POINT ( 'NONE',  ( -2.923830769312651068, 1.673677222459564851, 0.4126138247051237551 ) ) ;
#44826 = AXIS2_PLACEMENT_3D ( 'NONE', #18450, #17431, #37573 ) ;
#44827 = LINE ( 'NONE', #969, #24009 ) ;
#44828 = EDGE_CURVE ( 'NONE', #8308, #38746, #42346, .T. ) ;
#44829 = VERTEX_POINT ( 'NONE', #6232 ) ;
#44830 = EDGE_CURVE ( 'NONE', #32755, #10321, #41220, .T. ) ;
#44831 = LINE ( 'NONE', #8716, #30662 ) ;
#44832 = VECTOR ( 'NONE', #6665, 39.37007874015748143 ) ;
#44833 = ORIENTED_EDGE ( 'NONE', *, *, #38648, .F. ) ;
#44834 = ORIENTED_EDGE ( 'NONE', *, *, #33139, .T. ) ;
#44835 = EDGE_CURVE ( 'NONE', #25675, #721, #13979, .T. ) ;
#44836 = AXIS2_PLACEMENT_3D ( 'NONE', #31745, #49602, #33916 ) ;
#44837 = VECTOR ( 'NONE', #46735, 39.37007874015748143 ) ;
#44838 = VERTEX_POINT ( 'NONE', #14990 ) ;
#44839 = ORIENTED_EDGE ( 'NONE', *, *, #9407, .T. ) ;
#44840 = CARTESIAN_POINT ( 'NONE',  ( -1.712496953225537188, 3.267716535433071279, 5.941417334598190051E-16 ) ) ;
#44841 = VECTOR ( 'NONE', #1057, 39.37007874015748143 ) ;
#44842 = ORIENTED_EDGE ( 'NONE', *, *, #22861, .T. ) ;
#44843 = LINE ( 'NONE', #9752, #37837 ) ;
#44844 = ORIENTED_EDGE ( 'NONE', *, *, #47370, .F. ) ;
#44845 = CARTESIAN_POINT ( 'NONE',  ( 2.151809081513405442, 2.755905511811027164, 0.2418202932658665705 ) ) ;
#44846 = ADVANCED_FACE ( 'NONE', ( #14741 ), #18866, .F. ) ;
#44847 = PLANE ( 'NONE',  #22261 ) ;
#44848 = VERTEX_POINT ( 'NONE', #42099 ) ;
#44849 = CARTESIAN_POINT ( 'NONE',  ( -2.695799277629577162, 1.571269479597534824, -1.205759334241492731 ) ) ;
#44850 = CARTESIAN_POINT ( 'NONE',  ( -1.221295136473707243, 0.000000000000000000, 1.323086612934683215 ) ) ;
#44851 = ORIENTED_EDGE ( 'NONE', *, *, #4644, .T. ) ;
#44852 = LINE ( 'NONE', #27521, #15919 ) ;
#44853 = DIRECTION ( 'NONE',  ( 1.734723475976806848E-16, -0.000000000000000000, 1.000000000000000000 ) ) ;
#44854 = EDGE_CURVE ( 'NONE', #11368, #34116, #18105, .T. ) ;
#44855 = DIRECTION ( 'NONE',  ( -0.7818314824680309139, -7.233942271706491519E-17, 0.6234898018587318180 ) ) ;
#44856 = CARTESIAN_POINT ( 'NONE',  ( -1.985260859929297572, 0.000000000000000000, -6.146657985744592735E-16 ) ) ;
#44857 = DIRECTION ( 'NONE',  ( 0.9998717552508121775, 0.01601477604151182663, 0.000000000000000000 ) ) ;
#44858 = ORIENTED_EDGE ( 'NONE', *, *, #37655, .T. ) ;
#44859 = CARTESIAN_POINT ( 'NONE',  ( -0.7728391137233561192, 0.5249316497054296038, -1.718240423813754747 ) ) ;
#44860 = CARTESIAN_POINT ( 'NONE',  ( -1.236813753895213086, 1.699986652445209634, -2.681693691597581974 ) ) ;
#44861 = B_SPLINE_CURVE_WITH_KNOTS ( 'NONE', 3,
 ( #37475, #25583, #2092, #17838 ),
 .UNSPECIFIED., .F., .F.,
 ( 4, 4 ),
 ( 0.03694420483709656700, 0.03855293945462513056 ),
 .UNSPECIFIED. ) ;
#44862 = ORIENTED_EDGE ( 'NONE', *, *, #11042, .T. ) ;
#44863 = LINE ( 'NONE', #3225, #37503 ) ;
#44864 = VECTOR ( 'NONE', #17378, 39.37007874015748143 ) ;
#44865 = AXIS2_PLACEMENT_3D ( 'NONE', #16451, #36842, #5590 ) ;
#44866 = VERTEX_POINT ( 'NONE', #7245 ) ;
#44867 = ADVANCED_FACE ( 'NONE', ( #6737 ), #22486, .F. ) ;
#44868 = AXIS2_PLACEMENT_3D ( 'NONE', #36903, #12890, #36644 ) ;
#44870 = VECTOR ( 'NONE', #10025, 39.37007874015748143 ) ;
#44869 = DIRECTION ( 'NONE',  ( 1.000000000000000000, -0.000000000000000000, 0.000000000000000000 ) ) ;
#44871 = LINE ( 'NONE', #13396, #8909 ) ;
#44872 = CARTESIAN_POINT ( 'NONE',  ( 0.000000000000000000, 3.267716535433071279, 1.062992125984246083 ) ) ;
#44873 = LINE ( 'NONE', #44113, #40922 ) ;
#44874 = VERTEX_POINT ( 'NONE', #29975 ) ;
#44875 = DIRECTION ( 'NONE',  ( 1.000000000000000000, -0.000000000000000000, 0.000000000000000000 ) ) ;
#44876 = VECTOR ( 'NONE', #25515, 39.37007874015748143 ) ;
#44877 = FACE_BOUND ( 'NONE', #19996, .T. ) ;
#44878 = ORIENTED_EDGE ( 'NONE', *, *, #15765, .T. ) ;
#44879 = CARTESIAN_POINT ( 'NONE',  ( 2.378961647330872786, 3.243536745096756047, 0.6063129507101621130 ) ) ;
#44880 = VERTEX_POINT ( 'NONE', #45692 ) ;
#44881 = DIRECTION ( 'NONE',  ( 1.000000000000000000, 0.000000000000000000, -3.469446951953613696E-16 ) ) ;
#44882 = PLANE ( 'NONE',  #24772 ) ;
#44883 = CARTESIAN_POINT ( 'NONE',  ( -1.909347346926324462, 0.000000000000000000, 0.5905511811023582691 ) ) ;
#44884 = DIRECTION ( 'NONE',  ( 1.734723475976806848E-16, -0.000000000000000000, 1.000000000000000000 ) ) ;
#44885 = ORIENTED_EDGE ( 'NONE', *, *, #30997, .T. ) ;
#44887 = ORIENTED_EDGE ( 'NONE', *, *, #15124, .T. ) ;
#44886 = ADVANCED_FACE ( 'NONE', ( #46199 ), #6990, .F. ) ;
#44888 = LINE ( 'NONE', #33307, #38370 ) ;
#44889 = CARTESIAN_POINT ( 'NONE',  ( 0.000000000000000000, 3.267716535433071279, -0.5118110236220467790 ) ) ;
#44890 = FACE_BOUND ( 'NONE', #18906, .T. ) ;
#44891 = ORIENTED_EDGE ( 'NONE', *, *, #7842, .F. ) ;
#44892 = EDGE_CURVE ( 'NONE', #3654, #5972, #26103, .T. ) ;
#44893 = DIRECTION ( 'NONE',  ( -0.000000000000000000, 0.000000000000000000, 1.000000000000000000 ) ) ;
#44894 = CARTESIAN_POINT ( 'NONE',  ( -1.325491792074585229, 5.905511811023623991, -2.638988599164752369 ) ) ;
#44895 = EDGE_CURVE ( 'NONE', #46251, #6728, #30739, .T. ) ;
#44896 = EDGE_CURVE ( 'NONE', #31511, #36611, #45313, .T. ) ;
#44897 = VERTEX_POINT ( 'NONE', #45438 ) ;
#44898 = LINE ( 'NONE', #10315, #35659 ) ;
#44899 = AXIS2_PLACEMENT_3D ( 'NONE', #24547, #47741, #43387 ) ;
#44900 = LINE ( 'NONE', #41813, #40252 ) ;
#44901 = ORIENTED_EDGE ( 'NONE', *, *, #34521, .F. ) ;
#44902 = CONICAL_SURFACE ( 'NONE', #23456, 2.246510896728926010, 0.01601546068027819014 ) ;
#44903 = ORIENTED_EDGE ( 'NONE', *, *, #49603, .T. ) ;
#44904 = AXIS2_PLACEMENT_3D ( 'NONE', #13280, #25655, #44501 ) ;
#44905 = ORIENTED_EDGE ( 'NONE', *, *, #8495, .F. ) ;
#44906 = DIRECTION ( 'NONE',  ( 0.01601477604151182663, -0.9998717552508123996, 0.000000000000000000 ) ) ;
#44907 = DIRECTION ( 'NONE',  ( 1.000000000000000000, 0.000000000000000000, 0.000000000000000000 ) ) ;
#44908 = EDGE_CURVE ( 'NONE', #29976, #33624, #10103, .T. ) ;
#44909 = DIRECTION ( 'NONE',  ( -1.000000000000000000, -0.000000000000000000, -0.000000000000000000 ) ) ;
#44910 = CARTESIAN_POINT ( 'NONE',  ( 1.091055626815043311, 3.346456692913386100, 1.889763779527550369 ) ) ;
#44911 = VERTEX_POINT ( 'NONE', #42846 ) ;
#44912 = ORIENTED_EDGE ( 'NONE', *, *, #30155, .T. ) ;
#44913 = AXIS2_PLACEMENT_3D ( 'NONE', #19628, #38515, #46472 ) ;
#44914 = FACE_OUTER_BOUND ( 'NONE', #35084, .T. ) ;
#44915 = PRESENTATION_STYLE_ASSIGNMENT (( #13442 ) ) ;
#44916 = DIRECTION ( 'NONE',  ( 0.8090169943749506709, 0.000000000000000000, -0.5877852522924684742 ) ) ;
#44917 = EDGE_CURVE ( 'NONE', #19997, #23450, #50797, .T. ) ;
#44918 = CARTESIAN_POINT ( 'NONE',  ( -1.720314620805551087, 0.000000000000000000, 0.2826945007888154726 ) ) ;
#44919 = CARTESIAN_POINT ( 'NONE',  ( -1.453832412804729302, 0.000000000000000000, -1.018633753700964428 ) ) ;
#44920 = CARTESIAN_POINT ( 'NONE',  ( 0.8182917201112824834, 0.000000000000000000, 1.417322834645662777 ) ) ;
#44921 = EDGE_CURVE ( 'NONE', #12966, #36796, #260, .T. ) ;
#44922 = CARTESIAN_POINT ( 'NONE',  ( -1.363819533518803029, 0.000000000000000000, 1.102362204724404160 ) ) ;
#44923 = EDGE_LOOP ( 'NONE', ( #1364, #2790, #22133, #21243 ) ) ;
#44924 = CARTESIAN_POINT ( 'NONE',  ( -0.2727639067037611054, 3.267716535433071279, -2.088563196121306476 ) ) ;
#44925 = DIRECTION ( 'NONE',  ( -0.6579387259397136978, 0.000000000000000000, 0.7530714660036097463 ) ) ;
#44926 = ORIENTED_EDGE ( 'NONE', *, *, #28330, .F. ) ;
#44927 = ADVANCED_FACE ( 'NONE', ( #39749 ), #7995, .F. ) ;
#44928 = ORIENTED_EDGE ( 'NONE', *, *, #27968, .F. ) ;
#44929 = CARTESIAN_POINT ( 'NONE',  ( 1.997134316236881091, 3.346456692913386100, -0.6692913385826764205 ) ) ;
#44930 = CARTESIAN_POINT ( 'NONE',  ( -0.6214413264104939882, 0.000000000000000000, 0.4724409448818872592 ) ) ;
#44931 = ORIENTED_EDGE ( 'NONE', *, *, #29700, .F. ) ;
#44932 = VECTOR ( 'NONE', #4295, 39.37007874015748143 ) ;
#44933 = VECTOR ( 'NONE', #690, 39.37007874015748143 ) ;
#44934 = EDGE_CURVE ( 'NONE', #17812, #32722, #31755, .T. ) ;
#44935 = ORIENTED_EDGE ( 'NONE', *, *, #23698, .F. ) ;
#44936 = VECTOR ( 'NONE', #44102, 39.37007874015748143 ) ;
#44937 = PLANE ( 'NONE',  #15506 ) ;
#44938 = VECTOR ( 'NONE', #46698, 39.37007874015748143 ) ;
#44939 = ORIENTED_EDGE ( 'NONE', *, *, #49451, .F. ) ;
#44940 = EDGE_CURVE ( 'NONE', #3623, #7160, #31249, .T. ) ;
#44941 = CARTESIAN_POINT ( 'NONE',  ( -0.1450934409768900590, 0.000000000000000000, 2.161127057262024032 ) ) ;
#44942 = DIRECTION ( 'NONE',  ( 0.000000000000000000, -1.000000000000000000, 0.000000000000000000 ) ) ;
#44943 = ORIENTED_EDGE ( 'NONE', *, *, #6694, .T. ) ;
#44944 = ORIENTED_EDGE ( 'NONE', *, *, #47434, .T. ) ;
#44945 = VERTEX_POINT ( 'NONE', #35375 ) ;
#44946 = VECTOR ( 'NONE', #46820, 39.37007874015748143 ) ;
#44947 = CARTESIAN_POINT ( 'NONE',  ( 0.9319704666822036243, 0.04284687812831378811, 1.655805649632502430 ) ) ;
#44948 = ORIENTED_EDGE ( 'NONE', *, *, #6912, .T. ) ;
#44949 = ORIENTED_EDGE ( 'NONE', *, *, #24929, .T. ) ;
#44950 = LINE ( 'NONE', #10111, #27285 ) ;
#44951 = FACE_OUTER_BOUND ( 'NONE', #30927, .T. ) ;
#44952 = CARTESIAN_POINT ( 'NONE',  ( 1.091055626815042423, 0.000000000000000000, -1.574803149606294417 ) ) ;
#44953 = ADVANCED_FACE ( 'NONE', ( #35622 ), #38983, .T. ) ;
#44954 = EDGE_LOOP ( 'NONE', ( #30317, #47292, #12331, #34495 ) ) ;
#44955 = FACE_OUTER_BOUND ( 'NONE', #15040, .T. ) ;
#44956 =( BOUNDED_CURVE ( )  B_SPLINE_CURVE ( 3, ( #28672, #20153, #47744, #36689 ),
 .UNSPECIFIED., .F., .F. ) 
 B_SPLINE_CURVE_WITH_KNOTS ( ( 4, 4 ),
 ( 1.282939940669038714, 1.333860994033941205 ),
 .UNSPECIFIED. ) 
 CURVE ( )  GEOMETRIC_REPRESENTATION_ITEM ( )  RATIONAL_B_SPLINE_CURVE ( ( 1.000000000000000000, 0.9997839321993498007, 0.9997839321993498007, 1.000000000000000000 ) ) 
 REPRESENTATION_ITEM ( '' )  );
#44957 = LINE ( 'NONE', #9351, #30801 ) ;
#44958 = CARTESIAN_POINT ( 'NONE',  ( 1.232620761116212771, 6.692913385826772199, -1.780282403660734758 ) ) ;
#44959 = ADVANCED_FACE ( 'NONE', ( #35878 ), #18178, .F. ) ;
#44960 = ORIENTED_EDGE ( 'NONE', *, *, #9271, .T. ) ;
#44961 = CARTESIAN_POINT ( 'NONE',  ( 0.7423782071083091516, 3.346456692913386100, 1.062992125984246083 ) ) ;
#44962 = DIRECTION ( 'NONE',  ( 0.000000000000000000, 0.000000000000000000, 1.000000000000000000 ) ) ;
#44963 = DIRECTION ( 'NONE',  ( -0.000000000000000000, 1.000000000000000000, -0.000000000000000000 ) ) ;
#44964 = VERTEX_POINT ( 'NONE', #3620 ) ;
#44965 = ORIENTED_EDGE ( 'NONE', *, *, #10962, .T. ) ;
#44966 =( NAMED_UNIT ( * ) PLANE_ANGLE_UNIT ( ) SI_UNIT ( $, .RADIAN. ) );
#44967 = CARTESIAN_POINT ( 'NONE',  ( 0.7381027496705269142, 1.205361022782829114E-17, -2.859439394060913298 ) ) ;
#44968 = CARTESIAN_POINT ( 'NONE',  ( 1.836615784862988932, 1.645866884192403123, 2.027377764185913200 ) ) ;
#44969 = PLANE ( 'NONE',  #31247 ) ;
#44970 = ORIENTED_EDGE ( 'NONE', *, *, #9108, .T. ) ;
#44971 = ORIENTED_EDGE ( 'NONE', *, *, #39375, .T. ) ;
#44972 = VECTOR ( 'NONE', #44166, 39.37007874015748143 ) ;
#44973 = AXIS2_PLACEMENT_3D ( 'NONE', #7457, #3584, #19317 ) ;
#44974 = CARTESIAN_POINT ( 'NONE',  ( -0.8942052331142552601, 3.346456692913386100, -7.512581982576723358E-16 ) ) ;
#44975 = VERTEX_POINT ( 'NONE', #19350 ) ;
#44976 = CARTESIAN_POINT ( 'NONE',  ( -2.182111253630085290, 0.000000000000000000, 0.3149606299212578953 ) ) ;
#44977 = CARTESIAN_POINT ( 'NONE',  ( 0.8182917201112822614, 3.267716535433071279, -1.419509857074483785E-16 ) ) ;
#44978 = VECTOR ( 'NONE', #16255, 39.37007874015748143 ) ;
#44979 = VECTOR ( 'NONE', #43616, 39.37007874015748143 ) ;
#44980 = EDGE_CURVE ( 'NONE', #43175, #39048, #46943, .T. ) ;
#44981 = DIRECTION ( 'NONE',  ( -0.000000000000000000, 0.000000000000000000, 1.000000000000000000 ) ) ;
#44982 = LINE ( 'NONE', #17634, #7941 ) ;
#44983 = CARTESIAN_POINT ( 'NONE',  ( 0.4696143004045484903, 3.346456692913386100, 2.047244094488179567 ) ) ;
#44984 = AXIS2_PLACEMENT_3D ( 'NONE', #13921, #46144, #11058 ) ;
#44985 = ORIENTED_EDGE ( 'NONE', *, *, #45338, .F. ) ;
#44986 = CARTESIAN_POINT ( 'NONE',  ( 1.443077687459978886, 1.639689301329355198, 2.319355385847401418 ) ) ;
#44987 = CARTESIAN_POINT ( 'NONE',  ( 0.8182917201112824834, 3.346456692913386100, 1.220472440944875281 ) ) ;
#44988 = CARTESIAN_POINT ( 'NONE',  ( -1.716666360678977155, 3.346456692913386100, 1.220472440944875059 ) ) ;
#44989 = ADVANCED_FACE ( 'NONE', ( #34865 ), #29712, .F. ) ;
#44990 = ORIENTED_EDGE ( 'NONE', *, *, #24776, .T. ) ;
#44991 = CARTESIAN_POINT ( 'NONE',  ( -1.478704527843389682, 1.589829732135338070, -1.951536704579532433 ) ) ;
#44992 = EDGE_CURVE ( 'NONE', #36525, #36526, #27352, .T. ) ;
#44993 = CARTESIAN_POINT ( 'NONE',  ( 0.08139965876239094178, 1.610780518492231694, 0.000000000000000000 ) ) ;
#44994 = DIRECTION ( 'NONE',  ( -0.000000000000000000, 1.000000000000000000, -0.000000000000000000 ) ) ;
#44996 = EDGE_CURVE ( 'NONE', #17115, #3832, #7741, .T. ) ;
#44995 = ORIENTED_EDGE ( 'NONE', *, *, #5595, .T. ) ;
#44997 = DIRECTION ( 'NONE',  ( 0.000000000000000000, 0.000000000000000000, 1.000000000000000000 ) ) ;
#44998 = CARTESIAN_POINT ( 'NONE',  ( 2.013079221890065273, 0.03945196200391452857, -0.1396696942857607870 ) ) ;
#44999 = EDGE_CURVE ( 'NONE', #29935, #30018, #23482, .T. ) ;
#45000 = VERTEX_POINT ( 'NONE', #51051 ) ;
#45001 = DIRECTION ( 'NONE',  ( -0.3090169943749582204, 0.000000000000000000, 0.9510565162951500895 ) ) ;
#45002 = PLANE ( 'NONE',  #2700 ) ;
#45003 = EDGE_LOOP ( 'NONE', ( #15261, #30379, #933, #2421 ) ) ;
#45004 = DIRECTION ( 'NONE',  ( 1.734723475976806848E-16, 0.000000000000000000, 1.000000000000000000 ) ) ;
#45005 = DIRECTION ( 'NONE',  ( 0.000000000000000000, 0.000000000000000000, 1.000000000000000000 ) ) ;
#45006 = DIRECTION ( 'NONE',  ( 0.000000000000000000, 0.000000000000000000, 1.000000000000000000 ) ) ;
#45007 = CARTESIAN_POINT ( 'NONE',  ( 0.000000000000000000, 6.692913385826772199, 0.000000000000000000 ) ) ;
#45008 = AXIS2_PLACEMENT_3D ( 'NONE', #14526, #50336, #2901 ) ;
#45009 = FACE_OUTER_BOUND ( 'NONE', #417, .T. ) ;
#45010 = ORIENTED_EDGE ( 'NONE', *, *, #21936, .F. ) ;
#45011 = ORIENTED_EDGE ( 'NONE', *, *, #39319, .T. ) ;
#45012 = CARTESIAN_POINT ( 'NONE',  ( -0.5455278134075214336, 3.346456692913386100, -1.456692913385822630 ) ) ;
#45013 = CIRCLE ( 'NONE', #36780, 2.106299212598425008 ) ;
#45014 = FACE_OUTER_BOUND ( 'NONE', #39475, .T. ) ;
#45015 = VECTOR ( 'NONE', #19513, 39.37007874015748143 ) ;
#45016 = ORIENTED_EDGE ( 'NONE', *, *, #48835, .T. ) ;
#45017 = DIRECTION ( 'NONE',  ( 1.000000000000000000, 0.000000000000000000, -3.469446951953613696E-16 ) ) ;
#45018 = DIRECTION ( 'NONE',  ( -0.000000000000000000, -1.000000000000000000, 0.000000000000000000 ) ) ;
#45019 = DIRECTION ( 'NONE',  ( -0.000000000000000000, 1.000000000000000000, -0.000000000000000000 ) ) ;
#45020 = CIRCLE ( 'NONE', #3828, 2.443628662382284489 ) ;
#45021 = EDGE_CURVE ( 'NONE', #13400, #51046, #16517, .T. ) ;
#45022 = ORIENTED_EDGE ( 'NONE', *, *, #40092, .F. ) ;
#45023 = ORIENTED_EDGE ( 'NONE', *, *, #11633, .F. ) ;
#45024 = CARTESIAN_POINT ( 'NONE',  ( -0.07591351300297277671, 3.346456692913386100, 1.417322834645662777 ) ) ;
#45025 = VECTOR ( 'NONE', #44461, 39.37007874015748143 ) ;
#45026 = CARTESIAN_POINT ( 'NONE',  ( -1.843472447131334624, 1.579950168977349412, -1.157898127912315944 ) ) ;
#45027 = EDGE_CURVE ( 'NONE', #39907, #47540, #5115, .T. ) ;
#45028 = ORIENTED_EDGE ( 'NONE', *, *, #33029, .T. ) ;
#45029 = DIRECTION ( 'NONE',  ( -1.000000000000000000, -0.000000000000000000, -0.000000000000000000 ) ) ;
#45031 = VECTOR ( 'NONE', #31901, 39.37007874015748143 ) ;
#45030 = FACE_BOUND ( 'NONE', #39198, .T. ) ;
#45032 = EDGE_LOOP ( 'NONE', ( #36040, #49874, #13985, #39221 ) ) ;
#45033 = CARTESIAN_POINT ( 'NONE',  ( -1.712496953225537188, 0.000000000000000000, 0.2755905511810996522 ) ) ;
#45034 = ORIENTED_EDGE ( 'NONE', *, *, #5283, .F. ) ;
#45035 = ORIENTED_EDGE ( 'NONE', *, *, #13214, .F. ) ;
#45036 = CARTESIAN_POINT ( 'NONE',  ( 2.378961647330872786, 0.000000000000000000, -0.3149606299212596716 ) ) ;
#45037 = ORIENTED_EDGE ( 'NONE', *, *, #10814, .F. ) ;
#45038 = DIRECTION ( 'NONE',  ( -0.000000000000000000, 0.000000000000000000, 1.000000000000000000 ) ) ;
#45039 = LINE ( 'NONE', #6832, #38697 ) ;
#45040 = VERTEX_POINT ( 'NONE', #28116 ) ;
#45041 = LINE ( 'NONE', #25951, #5486 ) ;
#45042 = LINE ( 'NONE', #9950, #23454 ) ;
#45043 = VECTOR ( 'NONE', #22904, 39.37007874015748143 ) ;
#45044 = DIRECTION ( 'NONE',  ( 1.000000000000000000, 0.000000000000000000, 0.000000000000000000 ) ) ;
#45045 = DIRECTION ( 'NONE',  ( -0.000000000000000000, 1.000000000000000000, -0.000000000000000000 ) ) ;
#45046 = CARTESIAN_POINT ( 'NONE',  ( -0.3136974817027967100, 1.522126940893053337, -2.936457595020224520 ) ) ;
#45047 = CIRCLE ( 'NONE', #7111, 2.106299212598425008 ) ;
#45048 = ORIENTED_EDGE ( 'NONE', *, *, #25228, .F. ) ;
#45049 = CARTESIAN_POINT ( 'NONE',  ( 1.636583440222563857, 0.000000000000000000, 1.574803149606291974 ) ) ;
#45050 = VECTOR ( 'NONE', #39594, 39.37007874015748143 ) ;
#45051 = CARTESIAN_POINT ( 'NONE',  ( -1.909347346926324462, 3.267716535433071279, 0.2755905511810996522 ) ) ;
#45052 = ORIENTED_EDGE ( 'NONE', *, *, #4538, .T. ) ;
#45053 = CARTESIAN_POINT ( 'NONE',  ( -0.6214413264104945434, 0.000000000000000000, -0.7874015748031467643 ) ) ;
#45054 = EDGE_CURVE ( 'NONE', #27411, #45218, #43861, .T. ) ;
#45055 = CARTESIAN_POINT ( 'NONE',  ( 0.000000000000000000, 7.874015748031496287, -0.3740157480314960647 ) ) ;
#45056 = ORIENTED_EDGE ( 'NONE', *, *, #16531, .T. ) ;
#45057 = CARTESIAN_POINT ( 'NONE',  ( -2.160407304981126764, 1.574803149606302854, -0.1462862061266896330 ) ) ;
#45058 = VECTOR ( 'NONE', #45534, 39.37007874015748143 ) ;
#45059 = EDGE_CURVE ( 'NONE', #34396, #19510, #30989, .T. ) ;
#45060 = CARTESIAN_POINT ( 'NONE',  ( -0.5968551078519344077, 0.01230706739460726146, 1.730372017133659845 ) ) ;
#45061 = EDGE_CURVE ( 'NONE', #12747, #37485, #36395, .T. ) ;
#45062 = CARTESIAN_POINT ( 'NONE',  ( 1.287906020515829919, 3.267716535433071279, -4.468321617281354090E-16 ) ) ;
#45063 = ORIENTED_EDGE ( 'NONE', *, *, #82, .T. ) ;
#45064 = LINE ( 'NONE', #5330, #30706 ) ;
#45065 = ORIENTED_EDGE ( 'NONE', *, *, #18268, .F. ) ;
#45066 = FACE_BOUND ( 'NONE', #47410, .T. ) ;
#45067 = DIRECTION ( 'NONE',  ( 0.000000000000000000, 1.000000000000000000, 0.000000000000000000 ) ) ;
#45068 = DIRECTION ( 'NONE',  ( -0.000000000000000000, 0.000000000000000000, 1.000000000000000000 ) ) ;
#45069 = CARTESIAN_POINT ( 'NONE',  ( -1.062992125984251413, 0.5314960629921257063, -1.122047244094488416 ) ) ;
#45070 = ORIENTED_EDGE ( 'NONE', *, *, #39906, .F. ) ;
#45071 = EDGE_LOOP ( 'NONE', ( #26960, #21327, #6579, #6377, #16198 ) ) ;
#45072 = CARTESIAN_POINT ( 'NONE',  ( 0.5455278134075208785, 3.267716535433071279, -1.574803149606293529 ) ) ;
#45073 = ORIENTED_EDGE ( 'NONE', *, *, #47536, .F. ) ;
#45074 = EDGE_CURVE ( 'NONE', #17294, #31774, #1532, .T. ) ;
#45075 = FACE_OUTER_BOUND ( 'NONE', #2896, .T. ) ;
#45076 = VERTEX_POINT ( 'NONE', #16520 ) ;
#45077 = CARTESIAN_POINT ( 'NONE',  ( 0.000000000000000000, 3.346456692913386100, 0.000000000000000000 ) ) ;
#45078 = ADVANCED_FACE ( 'NONE', ( #1277 ), #44882, .F. ) ;
#45079 = ORIENTED_EDGE ( 'NONE', *, *, #49907, .F. ) ;
#45080 = DIRECTION ( 'NONE',  ( -0.000000000000000000, 1.000000000000000000, -0.000000000000000000 ) ) ;
#45081 = AXIS2_PLACEMENT_3D ( 'NONE', #6349, #26217, #2478 ) ;
#45082 = ADVANCED_FACE ( 'NONE', ( #5403 ), #770, .F. ) ;
#45083 = CARTESIAN_POINT ( 'NONE',  ( -2.154691421597259904, 1.673393017852502718, -0.2175766031914168064 ) ) ;
#45084 = VECTOR ( 'NONE', #38467, 39.37007874015748143 ) ;
#45085 = EDGE_LOOP ( 'NONE', ( #27248, #18956, #18536, #7395 ) ) ;
#45086 = EDGE_CURVE ( 'NONE', #9369, #20825, #12903, .T. ) ;
#45087 = CARTESIAN_POINT ( 'NONE',  ( -1.743145509346914590, -1.899488058094683170E-15, 0.000000000000000000 ) ) ;
#45088 = EDGE_LOOP ( 'NONE', ( #7829, #29491, #49741, #21729 ) ) ;
#45089 = ORIENTED_EDGE ( 'NONE', *, *, #20569, .T. ) ;
#45090 = VECTOR ( 'NONE', #11708, 39.37007874015748143 ) ;
#45091 = EDGE_LOOP ( 'NONE', ( #44688, #41489, #35326, #18790 ) ) ;
#45092 = ORIENTED_EDGE ( 'NONE', *, *, #15041, .T. ) ;
#45093 = DIRECTION ( 'NONE',  ( 0.000000000000000000, 1.000000000000000000, 0.000000000000000000 ) ) ;
#45094 = ORIENTED_EDGE ( 'NONE', *, *, #31264, .F. ) ;
#45095 = CARTESIAN_POINT ( 'NONE',  ( 0.4696143004045476577, 3.267716535433071279, -1.732283464566922726 ) ) ;
#45096 = FACE_OUTER_BOUND ( 'NONE', #9008, .T. ) ;
#45097 = LINE ( 'NONE', #5368, #32181 ) ;
#45098 = EDGE_LOOP ( 'NONE', ( #13902, #40366, #31959, #18317 ) ) ;
#45099 = LINE ( 'NONE', #9759, #18721 ) ;
#45100 = LINE ( 'NONE', #34273, #29574 ) ;
#45101 = VERTEX_POINT ( 'NONE', #9279 ) ;
#45102 = CARTESIAN_POINT ( 'NONE',  ( 4.439252989704372263E-17, 3.267716535433071279, -7.700876377040399808E-33 ) ) ;
#45103 = CARTESIAN_POINT ( 'NONE',  ( -1.198202975868765119, 3.346456692913386100, -1.732283464566922726 ) ) ;
#45104 = DIRECTION ( 'NONE',  ( -1.000000000000000000, 0.000000000000000000, 0.000000000000000000 ) ) ;
#45105 = CARTESIAN_POINT ( 'NONE',  ( 0.000000000000000000, 3.346456692913386100, 0.000000000000000000 ) ) ;
#45106 = CARTESIAN_POINT ( 'NONE',  ( -0.8182917201112819283, 3.267716535433071279, -1.614173228346451605 ) ) ;
#45107 = CARTESIAN_POINT ( 'NONE',  ( -1.363819533518803473, 3.346456692913386100, 2.047244094488179567 ) ) ;
#45108 = ORIENTED_EDGE ( 'NONE', *, *, #41668, .F. ) ;
#45109 = LINE ( 'NONE', #45869, #46051 ) ;
#45110 = VECTOR ( 'NONE', #21485, 39.37007874015748143 ) ;
#45111 = VECTOR ( 'NONE', #44172, 39.37007874015748143 ) ;
#45112 = CARTESIAN_POINT ( 'NONE',  ( 0.000000000000000000, 3.267716535433071279, 0.5905511811023582691 ) ) ;
#45113 = ADVANCED_FACE ( 'NONE', ( #47964 ), #28637, .F. ) ;
#45114 = ORIENTED_EDGE ( 'NONE', *, *, #30782, .T. ) ;
#45115 = VECTOR ( 'NONE', #45045, 39.37007874015748143 ) ;
#45116 = CARTESIAN_POINT ( 'NONE',  ( 1.636583440222563857, 3.346456692913386100, 0.3149606299212576177 ) ) ;
#45117 = EDGE_CURVE ( 'NONE', #44259, #50692, #24872, .T. ) ;
#45118 = ORIENTED_EDGE ( 'NONE', *, *, #30682, .T. ) ;
#45119 = CARTESIAN_POINT ( 'NONE',  ( 0.8182917201112817063, 0.000000000000000000, -2.047244094488181343 ) ) ;
#45120 = EDGE_CURVE ( 'NONE', #22175, #40166, #34687, .T. ) ;
#45121 = CARTESIAN_POINT ( 'NONE',  ( -0.3857230305054721864, 0.000000000000000000, 1.849896105471422025 ) ) ;
#45122 = LINE ( 'NONE', #1774, #356 ) ;
#45123 = LINE ( 'NONE', #1775, #36793 ) ;
#45124 = ORIENTED_EDGE ( 'NONE', *, *, #12692, .T. ) ;
#45125 = DIRECTION ( 'NONE',  ( -1.000000000000000000, 0.000000000000000000, -0.000000000000000000 ) ) ;
#45126 = ORIENTED_EDGE ( 'NONE', *, *, #29515, .F. ) ;
#45127 = CARTESIAN_POINT ( 'NONE',  ( 0.000000000000000000, 3.346456692913386100, 0.000000000000000000 ) ) ;
#45128 = ORIENTED_EDGE ( 'NONE', *, *, #33301, .T. ) ;
#45129 = DIRECTION ( 'NONE',  ( -0.9998717552508122886, -0.01601477604151185785, 0.000000000000000000 ) ) ;
#45130 = VECTOR ( 'NONE', #39661, 39.37007874015748143 ) ;
#45131 = LINE ( 'NONE', #25531, #30993 ) ;
#45132 = ORIENTED_EDGE ( 'NONE', *, *, #7752, .T. ) ;
#45133 = DIRECTION ( 'NONE',  ( 0.000000000000000000, 0.000000000000000000, -1.000000000000000000 ) ) ;
#45134 = EDGE_CURVE ( 'NONE', #21655, #1296, #25534, .T. ) ;
#45135 = CARTESIAN_POINT ( 'NONE',  ( 1.472219874544873131, 0.000000000000000000, 2.560030851058970214 ) ) ;
#45136 = CARTESIAN_POINT ( 'NONE',  ( 1.909347346926324684, 0.000000000000000000, -0.1574803149606304187 ) ) ;
#45137 = ORIENTED_EDGE ( 'NONE', *, *, #430, .F. ) ;
#45138 = VERTEX_POINT ( 'NONE', #21162 ) ;
#45139 = ADVANCED_FACE ( 'NONE', ( #48728 ), #9536, .F. ) ;
#45140 = DIRECTION ( 'NONE',  ( -0.9998717552508121775, -0.01601477604151182663, 0.000000000000000000 ) ) ;
#45141 = FACE_BOUND ( 'NONE', #43471, .T. ) ;
#45142 = PLANE ( 'NONE',  #36112 ) ;
#45143 = CARTESIAN_POINT ( 'NONE',  ( -0.07591351300297340121, 3.267716535433071279, -1.299212598425193210 ) ) ;
#45144 = AXIS2_PLACEMENT_3D ( 'NONE', #49857, #42405, #26408 ) ;
#45145 = VECTOR ( 'NONE', #756, 39.37007874015748143 ) ;
#45146 = ORIENTED_EDGE ( 'NONE', *, *, #38571, .F. ) ;
#45147 = ORIENTED_EDGE ( 'NONE', *, *, #11979, .T. ) ;
#45148 = CARTESIAN_POINT ( 'NONE',  ( -0.8942052331142552601, 3.267716535433071279, -2.086614173228339641 ) ) ;
#45149 = CARTESIAN_POINT ( 'NONE',  ( 0.000000000000000000, 3.267716535433071279, 0.000000000000000000 ) ) ;
#45150 = ORIENTED_EDGE ( 'NONE', *, *, #2973, .T. ) ;
#45151 = ORIENTED_EDGE ( 'NONE', *, *, #23506, .T. ) ;
#45152 = VECTOR ( 'NONE', #43366, 39.37007874015748143 ) ;
#45153 = VERTEX_POINT ( 'NONE', #28378 ) ;
#45154 = LINE ( 'NONE', #9818, #47414 ) ;
#45155 = DIRECTION ( 'NONE',  ( 0.000000000000000000, 0.000000000000000000, 1.000000000000000000 ) ) ;
#45156 = CARTESIAN_POINT ( 'NONE',  ( 1.909347346926324684, 3.267716535433071279, -3.312189666507128175E-16 ) ) ;
#45157 = DIRECTION ( 'NONE',  ( 1.000000000000000000, 0.000000000000000000, 0.000000000000000000 ) ) ;
#45158 = VECTOR ( 'NONE', #5932, 39.37007874015748143 ) ;
#45159 = ORIENTED_EDGE ( 'NONE', *, *, #7530, .F. ) ;
#45160 = VERTEX_POINT ( 'NONE', #17037 ) ;
#45161 = LINE ( 'NONE', #37714, #6828 ) ;
#45162 = DIRECTION ( 'NONE',  ( -0.000000000000000000, 1.000000000000000000, -0.000000000000000000 ) ) ;
#45163 = CARTESIAN_POINT ( 'NONE',  ( 1.636583440222563857, 3.267716535433071279, 1.259842519685033135 ) ) ;
#45164 = CIRCLE ( 'NONE', #20454, 2.164630168518208109 ) ;
#45165 = DIRECTION ( 'NONE',  ( -0.000000000000000000, 0.000000000000000000, 1.000000000000000000 ) ) ;
#45166 = CARTESIAN_POINT ( 'NONE',  ( -2.339241080213612545, 0.000000000000000000, 1.802537235681884065 ) ) ;
#45167 = DIRECTION ( 'NONE',  ( 1.734723475976806848E-16, -0.000000000000000000, 1.000000000000000000 ) ) ;
#45168 = LINE ( 'NONE', #12945, #1138 ) ;
#45169 = EDGE_CURVE ( 'NONE', #7335, #39537, #32792, .T. ) ;
#45170 = ORIENTED_EDGE ( 'NONE', *, *, #32815, .F. ) ;
#45171 = DIRECTION ( 'NONE',  ( -0.000000000000000000, 1.000000000000000000, -0.000000000000000000 ) ) ;
#45172 = PLANE ( 'NONE',  #11236 ) ;
#45173 = EDGE_CURVE ( 'NONE', #30240, #20976, #29820, .T. ) ;
#45174 = ORIENTED_EDGE ( 'NONE', *, *, #28070, .T. ) ;
#45175 = EDGE_CURVE ( 'NONE', #16977, #35527, #25283, .T. ) ;
#45176 = ORIENTED_EDGE ( 'NONE', *, *, #20888, .F. ) ;
#45177 = LINE ( 'NONE', #13209, #21638 ) ;
#45178 = DIRECTION ( 'NONE',  ( 0.5128992774058948045, 0.000000000000000000, 0.8584487936018727616 ) ) ;
#45179 = VECTOR ( 'NONE', #959, 39.37007874015748143 ) ;
#45180 = ORIENTED_EDGE ( 'NONE', *, *, #30230, .T. ) ;
#45181 = ADVANCED_FACE ( 'NONE', ( #41042 ), #21413, .F. ) ;
#45182 = ORIENTED_EDGE ( 'NONE', *, *, #7096, .T. ) ;
#45183 = CARTESIAN_POINT ( 'NONE',  ( -3.414809992080329023E-17, 3.346456692913386100, -0.1968503937007874405 ) ) ;
#45184 = AXIS2_PLACEMENT_3D ( 'NONE', #38332, #41435, #17941 ) ;
#45185 = ORIENTED_EDGE ( 'NONE', *, *, #38514, .T. ) ;
#45186 = VECTOR ( 'NONE', #34858, 39.37007874015748143 ) ;
#45187 = DIRECTION ( 'NONE',  ( -1.000000000000000000, 0.000000000000000000, 1.734723475976806848E-16 ) ) ;
#45188 = LINE ( 'NONE', #9852, #40412 ) ;
#45189 = EDGE_CURVE ( 'NONE', #28145, #21463, #8767, .T. ) ;
#45190 = VECTOR ( 'NONE', #36556, 39.37007874015748143 ) ;
#45191 = ORIENTED_EDGE ( 'NONE', *, *, #19937, .T. ) ;
#45192 = EDGE_LOOP ( 'NONE', ( #23487, #36169, #6415, #25897 ) ) ;
#45193 = DIRECTION ( 'NONE',  ( -1.000000000000000000, -0.000000000000000000, -0.000000000000000000 ) ) ;
#45194 = ORIENTED_EDGE ( 'NONE', *, *, #29236, .F. ) ;
#45195 = ORIENTED_EDGE ( 'NONE', *, *, #16465, .T. ) ;
#45196 = EDGE_CURVE ( 'NONE', #43525, #24410, #20640, .T. ) ;
#45197 = DIRECTION ( 'NONE',  ( -1.000000000000000000, 0.000000000000000000, 0.000000000000000000 ) ) ;
#45198 = FACE_OUTER_BOUND ( 'NONE', #14407, .T. ) ;
#45199 = DIRECTION ( 'NONE',  ( -0.000000000000000000, 0.000000000000000000, 1.000000000000000000 ) ) ;
#45200 = AXIS2_PLACEMENT_3D ( 'NONE', #18534, #6659, #45362 ) ;
#45201 = ORIENTED_EDGE ( 'NONE', *, *, #13967, .T. ) ;
#45202 = CARTESIAN_POINT ( 'NONE',  ( 1.091055626815042645, 3.267716535433071279, -0.3149606299212596716 ) ) ;
#45203 = CARTESIAN_POINT ( 'NONE',  ( -0.3486774197067334380, 0.000000000000000000, 1.889763779527550369 ) ) ;
#45204 = EDGE_CURVE ( 'NONE', #15077, #28112, #14429, .T. ) ;
#45205 = DIRECTION ( 'NONE',  ( -3.469446951953613696E-16, 0.000000000000000000, -1.000000000000000000 ) ) ;
#45206 = VERTEX_POINT ( 'NONE', #41796 ) ;
#45207 = LINE ( 'NONE', #27119, #19945 ) ;
#45208 = DIRECTION ( 'NONE',  ( 1.734723475976806848E-16, 0.000000000000000000, 1.000000000000000000 ) ) ;
#45209 = PLANE ( 'NONE',  #19990 ) ;
#45210 = EDGE_LOOP ( 'NONE', ( #21462, #46741, #15841, #15208 ) ) ;
#45211 = VERTEX_POINT ( 'NONE', #26044 ) ;
#45212 = ADVANCED_FACE ( 'NONE', ( #2047 ), #30173, .F. ) ;
#45213 = DIRECTION ( 'NONE',  ( -3.469446951953613696E-16, 0.000000000000000000, -1.000000000000000000 ) ) ;
#45214 = CIRCLE ( 'NONE', #34523, 2.106299212598425008 ) ;
#45215 = CARTESIAN_POINT ( 'NONE',  ( -1.181102362204724088, 0.4724409448818890911, 1.181102362204724088 ) ) ;
#45216 = LINE ( 'NONE', #5998, #4090 ) ;
#45217 = ORIENTED_EDGE ( 'NONE', *, *, #33399, .T. ) ;
#45218 = VERTEX_POINT ( 'NONE', #21925 ) ;
#45219 = CARTESIAN_POINT ( 'NONE',  ( -0.3486774197067340486, 3.346456692913386100, -1.141732283464563791 ) ) ;
#45220 = VERTEX_POINT ( 'NONE', #25788 ) ;
#45221 = DIRECTION ( 'NONE',  ( -3.469446951953613696E-16, 0.000000000000000000, -1.000000000000000000 ) ) ;
#45222 = DIRECTION ( 'NONE',  ( 1.000000000000000000, -0.000000000000000000, 0.000000000000000000 ) ) ;
#45223 = VECTOR ( 'NONE', #28709, 39.37007874015748143 ) ;
#45224 = VECTOR ( 'NONE', #36523, 39.37007874015748143 ) ;
#45225 = VECTOR ( 'NONE', #40302, 39.37007874015748143 ) ;
#45226 = CARTESIAN_POINT ( 'NONE',  ( -0.3486774197067334380, 3.346456692913386100, 0.9448818897637749625 ) ) ;
#45227 = CARTESIAN_POINT ( 'NONE',  ( 1.287906020515830141, 3.346456692913386100, 0.1181102362204704270 ) ) ;
#45228 = CARTESIAN_POINT ( 'NONE',  ( 4.439252989704605840E-17, 3.267716535433071279, -7.700876377040806239E-33 ) ) ;
#45229 = EDGE_LOOP ( 'NONE', ( #5275, #2818, #26312, #26064 ) ) ;
#45230 = CARTESIAN_POINT ( 'NONE',  ( 1.015142113812069979, 3.346456692913386100, 1.417322834645662777 ) ) ;
#45231 = DIRECTION ( 'NONE',  ( 1.734723475976806848E-16, -0.000000000000000000, 1.000000000000000000 ) ) ;
#45232 = VECTOR ( 'NONE', #44237, 39.37007874015748143 ) ;
#45233 = LINE ( 'NONE', #25637, #35589 ) ;
#45234 = EDGE_CURVE ( 'NONE', #39032, #42424, #30680, .T. ) ;
#45235 = ORIENTED_EDGE ( 'NONE', *, *, #5257, .F. ) ;
#45236 = LINE ( 'NONE', #20747, #25694 ) ;
#45237 = CARTESIAN_POINT ( 'NONE',  ( 0.1067246931122726866, 0.02962905676920215767, 0.000000000000000000 ) ) ;
#45238 = CARTESIAN_POINT ( 'NONE',  ( 1.015142113812069313, 0.000000000000000000, -0.3543307086614175816 ) ) ;
#45239 = EDGE_CURVE ( 'NONE', #41605, #24016, #37685, .T. ) ;
#45240 = ORIENTED_EDGE ( 'NONE', *, *, #29703, .F. ) ;
#45241 = FACE_OUTER_BOUND ( 'NONE', #6028, .T. ) ;
#45242 = EDGE_CURVE ( 'NONE', #1339, #20947, #2299, .T. ) ;
#45243 = LINE ( 'NONE', #17904, #11852 ) ;
#45244 = EDGE_LOOP ( 'NONE', ( #22954, #41427, #31886, #41882 ) ) ;
#45245 = CARTESIAN_POINT ( 'NONE',  ( -1.712496953225537855, 3.346456692913386100, -1.226315847645294221 ) ) ;
#45246 = PLANE ( 'NONE',  #16711 ) ;
#45247 = ORIENTED_EDGE ( 'NONE', *, *, #24113, .T. ) ;
#45248 = CARTESIAN_POINT ( 'NONE',  ( -0.7380211471543357549, 0.01609890615456165824, -1.645940171248041928 ) ) ;
#45249 = DIRECTION ( 'NONE',  ( -1.000000000000000000, 0.000000000000000000, -0.000000000000000000 ) ) ;
#45250 = DIRECTION ( 'NONE',  ( 1.734723475976806848E-16, -0.000000000000000000, 1.000000000000000000 ) ) ;
#45251 = FACE_OUTER_BOUND ( 'NONE', #24026, .T. ) ;
#45252 =( BOUNDED_CURVE ( )  B_SPLINE_CURVE ( 3, ( #26887, #42382, #10398, #6533 ),
 .UNSPECIFIED., .F., .F. ) 
 B_SPLINE_CURVE_WITH_KNOTS ( ( 4, 4 ),
 ( 6.208269093772826430, 6.259010602608490181 ),
 .UNSPECIFIED. ) 
 CURVE ( )  GEOMETRIC_REPRESENTATION_ITEM ( )  RATIONAL_B_SPLINE_CURVE ( ( 1.000000000000000000, 0.9997854531153357316, 0.9997854531153357316, 1.000000000000000000 ) ) 
 REPRESENTATION_ITEM ( '' )  );
#45253 = VECTOR ( 'NONE', #25920, 39.37007874015748143 ) ;
#45254 = CARTESIAN_POINT ( 'NONE',  ( 1.287906020515830141, 0.000000000000000000, -0.1968503937007883287 ) ) ;
#45255 = EDGE_LOOP ( 'NONE', ( #36974, #738, #48330, #45463 ) ) ;
#45256 = ORIENTED_EDGE ( 'NONE', *, *, #2064, .T. ) ;
#45257 = CARTESIAN_POINT ( 'NONE',  ( 0.5455278134075217666, 0.000000000000000000, 1.259842519685033357 ) ) ;
#45258 = DIRECTION ( 'NONE',  ( -1.000000000000000000, -0.000000000000000000, -0.000000000000000000 ) ) ;
#45259 = VERTEX_POINT ( 'NONE', #45892 ) ;
#45260 = DIRECTION ( 'NONE',  ( -1.000000000000000000, 0.000000000000000000, -0.000000000000000000 ) ) ;
#45261 = FACE_OUTER_BOUND ( 'NONE', #49124, .T. ) ;
#45262 = DIRECTION ( 'NONE',  ( -1.000000000000000000, -0.000000000000000000, -0.000000000000000000 ) ) ;
#45263 = VECTOR ( 'NONE', #13823, 39.37007874015748143 ) ;
#45264 = VERTEX_POINT ( 'NONE', #2810 ) ;
#45265 = ORIENTED_EDGE ( 'NONE', *, *, #42395, .F. ) ;
#45266 = LINE ( 'NONE', #13806, #38658 ) ;
#45267 = DIRECTION ( 'NONE',  ( 0.000000000000000000, 0.000000000000000000, -1.000000000000000000 ) ) ;
#45268 = EDGE_CURVE ( 'NONE', #421, #5106, #30432, .T. ) ;
#45269 = CARTESIAN_POINT ( 'NONE',  ( 0.5905511811023627100, 0.000000000000000000, 2.165354330708661568 ) ) ;
#45270 = ORIENTED_EDGE ( 'NONE', *, *, #29275, .F. ) ;
#45271 = VECTOR ( 'NONE', #3739, 39.37007874015748143 ) ;
#45272 = LINE ( 'NONE', #6817, #19902 ) ;
#45273 = DIRECTION ( 'NONE',  ( -3.469446951953613696E-16, 0.000000000000000000, -1.000000000000000000 ) ) ;
#45274 = ORIENTED_EDGE ( 'NONE', *, *, #30882, .T. ) ;
#45275 = CARTESIAN_POINT ( 'NONE',  ( 0.000000000000000000, 3.267716535433071279, 2.047244094488179567 ) ) ;
#45276 = ORIENTED_EDGE ( 'NONE', *, *, #50581, .T. ) ;
#45277 = ORIENTED_EDGE ( 'NONE', *, *, #11585, .F. ) ;
#45278 = AXIS2_PLACEMENT_3D ( 'NONE', #2915, #18912, #46745 ) ;
#45279 = CARTESIAN_POINT ( 'NONE',  ( 0.2508718039770792552, 1.711920121901901348, -2.238407143905190910 ) ) ;
#45280 = CARTESIAN_POINT ( 'NONE',  ( -1.247273217833388514, 0.007942302252338809612, -1.260601835943744087 ) ) ;
#45281 = EDGE_CURVE ( 'NONE', #39129, #9746, #50000, .T. ) ;
#45282 = ADVANCED_FACE ( 'NONE', ( #6684 ), #34560, .F. ) ;
#45283 = VERTEX_POINT ( 'NONE', #46394 ) ;
#45284 = DIRECTION ( 'NONE',  ( -1.267583980596140612E-16, 1.000000000000000000, 2.300325776299552367E-17 ) ) ;
#45285 = DIRECTION ( 'NONE',  ( 1.734723475976806848E-16, 0.000000000000000000, 1.000000000000000000 ) ) ;
#45286 = ORIENTED_EDGE ( 'NONE', *, *, #47553, .F. ) ;
#45287 = EDGE_CURVE ( 'NONE', #23634, #17198, #33811, .T. ) ;
#45288 = DIRECTION ( 'NONE',  ( 1.000000000000000000, 0.000000000000000000, -3.469446951953613696E-16 ) ) ;
#45289 = CARTESIAN_POINT ( 'NONE',  ( 0.08139965876239094178, 1.610780518492231694, 0.000000000000000000 ) ) ;
#45290 = EDGE_CURVE ( 'NONE', #1678, #11612, #50287, .T. ) ;
#45291 = VECTOR ( 'NONE', #30436, 39.37007874015748143 ) ;
#45292 = LINE ( 'NONE', #1439, #26410 ) ;
#45293 = CARTESIAN_POINT ( 'NONE',  ( 2.059921668671832240, 6.692913385826772199, 0.7210543110491620666 ) ) ;
#45294 = FACE_OUTER_BOUND ( 'NONE', #34941, .T. ) ;
#45295 = ORIENTED_EDGE ( 'NONE', *, *, #10414, .F. ) ;
#45296 = DIRECTION ( 'NONE',  ( -1.000000000000000000, 0.000000000000000000, -0.000000000000000000 ) ) ;
#45297 = B_SPLINE_CURVE_WITH_KNOTS ( 'NONE', 3,
 ( #13704, #1821, #9572, #17574 ),
 .UNSPECIFIED., .F., .F.,
 ( 4, 4 ),
 ( 0.02707144773250385814, 0.02825827685263899644 ),
 .UNSPECIFIED. ) ;
#45298 = CARTESIAN_POINT ( 'NONE',  ( 0.2727639067037607168, 3.267716535433071279, -4.731699523581612823E-17 ) ) ;
#45299 = EDGE_CURVE ( 'NONE', #65, #40996, #49743, .T. ) ;
#45300 = AXIS2_PLACEMENT_3D ( 'NONE', #33639, #1619, #2128 ) ;
#45301 = ORIENTED_EDGE ( 'NONE', *, *, #6261, .F. ) ;
#45302 = DIRECTION ( 'NONE',  ( -1.000000000000000000, 0.000000000000000000, 0.000000000000000000 ) ) ;
#45303 = CARTESIAN_POINT ( 'NONE',  ( -1.166969139818015533, 3.346456692913386100, 1.417322834645662777 ) ) ;
#45304 = ORIENTED_EDGE ( 'NONE', *, *, #21998, .T. ) ;
#45305 = CARTESIAN_POINT ( 'NONE',  ( -0.6214413264104945434, 0.000000000000000000, -1.102362204724405492 ) ) ;
#45306 = EDGE_CURVE ( 'NONE', #31017, #2822, #10299, .T. ) ;
#45307 = CARTESIAN_POINT ( 'NONE',  ( -2.225563356869989295, 1.047115081372295142, 1.253512298962777605 ) ) ;
#45308 = ADVANCED_FACE ( 'NONE', ( #42290 ), #6937, .F. ) ;
#45309 = CARTESIAN_POINT ( 'NONE',  ( 1.959936762177996838, 0.000000000000000000, -0.8199101346145926117 ) ) ;
#45310 = ADVANCED_FACE ( 'NONE', ( #22179 ), #17791, .T. ) ;
#45311 = VERTEX_POINT ( 'NONE', #18559 ) ;
#45312 = DIRECTION ( 'NONE',  ( -0.000000000000000000, 1.000000000000000000, -0.000000000000000000 ) ) ;
#45313 = CIRCLE ( 'NONE', #23078, 2.244934639244525076 ) ;
#45314 = EDGE_LOOP ( 'NONE', ( #9064, #40170, #33395, #2414 ) ) ;
#45315 = FACE_BOUND ( 'NONE', #27820, .T. ) ;
#45316 = CARTESIAN_POINT ( 'NONE',  ( 0.08119777152254364916, 1.623385212329073957, 0.000000000000000000 ) ) ;
#45317 = CYLINDRICAL_SURFACE ( 'NONE', #8662, 0.3740157480314960647 ) ;
#45318 = DIRECTION ( 'NONE',  ( -0.000000000000000000, 0.000000000000000000, 1.000000000000000000 ) ) ;
#45319 = EDGE_LOOP ( 'NONE', ( #32020, #22514, #14087, #18582 ) ) ;
#45320 = ORIENTED_EDGE ( 'NONE', *, *, #5121, .T. ) ;
#45321 = CARTESIAN_POINT ( 'NONE',  ( 0.000000000000000000, 3.267716535433071279, 0.000000000000000000 ) ) ;
#45322 = ORIENTED_EDGE ( 'NONE', *, *, #11123, .T. ) ;
#45323 = CARTESIAN_POINT ( 'NONE',  ( 0.000000000000000000, 6.692913385826772199, 0.000000000000000000 ) ) ;
#45324 = ORIENTED_EDGE ( 'NONE', *, *, #38123, .F. ) ;
#45325 = CARTESIAN_POINT ( 'NONE',  ( -1.636583440222564301, 3.346456692913386100, -0.8267716535433052849 ) ) ;
#45326 = AXIS2_PLACEMENT_3D ( 'NONE', #10692, #49627, #37817 ) ;
#45327 = VERTEX_POINT ( 'NONE', #37426 ) ;
#45328 = LINE ( 'NONE', #22121, #34019 ) ;
#45329 = EDGE_CURVE ( 'NONE', #46654, #12774, #3061, .T. ) ;
#45330 = CARTESIAN_POINT ( 'NONE',  ( 2.473328170516846836, 1.757793565757150178, -1.612973743985320008 ) ) ;
#45331 = VERTEX_POINT ( 'NONE', #41540 ) ;
#45332 = CARTESIAN_POINT ( 'NONE',  ( -0.4788131938641533303, 1.711801685632677428, 2.914091152102185944 ) ) ;
#45333 = EDGE_LOOP ( 'NONE', ( #4683, #34550, #25083, #36777, #50159 ) ) ;
#45334 = ORIENTED_EDGE ( 'NONE', *, *, #43563, .F. ) ;
#45335 = EDGE_CURVE ( 'NONE', #9748, #22703, #46645, .T. ) ;
#45336 = VECTOR ( 'NONE', #43322, 39.37007874015748143 ) ;
#45337 = AXIS2_PLACEMENT_3D ( 'NONE', #2701, #49392, #41944 ) ;
#45338 = EDGE_CURVE ( 'NONE', #34034, #48695, #8203, .T. ) ;
#45339 = ADVANCED_FACE ( 'NONE', ( #31189 ), #7687, .F. ) ;
#45340 = ORIENTED_EDGE ( 'NONE', *, *, #50057, .T. ) ;
#45341 = ORIENTED_EDGE ( 'NONE', *, *, #23160, .T. ) ;
#45342 = LINE ( 'NONE', #36868, #8759 ) ;
#45343 = EDGE_CURVE ( 'NONE', #5165, #31344, #23427, .T. ) ;
#45344 = ORIENTED_EDGE ( 'NONE', *, *, #19760, .F. ) ;
#45345 = VECTOR ( 'NONE', #44382, 39.37007874015748143 ) ;
#45346 = DIRECTION ( 'NONE',  ( -0.7071067811865466846, -0.7071067811865483499, 7.903458058585701571E-16 ) ) ;
#45347 = CARTESIAN_POINT ( 'NONE',  ( 0.000000000000000000, 2.755905511811022723, 0.000000000000000000 ) ) ;
#45348 = DIRECTION ( 'NONE',  ( 1.734723475976806848E-16, -0.000000000000000000, 1.000000000000000000 ) ) ;
#45349 = EDGE_CURVE ( 'NONE', #41090, #15209, #27298, .T. ) ;
#45350 = EDGE_LOOP ( 'NONE', ( #15581, #7626, #5826, #46012 ) ) ;
#45351 = CARTESIAN_POINT ( 'NONE',  ( 0.002207914879453961969, 6.692913385826772199, 0.04916304461325451958 ) ) ;
#45352 = CARTESIAN_POINT ( 'NONE',  ( -0.2052282226254269204, 0.000000000000000000, -1.731265419273310346 ) ) ;
#45353 = ORIENTED_EDGE ( 'NONE', *, *, #49540, .F. ) ;
#45354 = LINE ( 'NONE', #37394, #23320 ) ;
#45355 = DIRECTION ( 'NONE',  ( 1.000000000000000000, 0.000000000000000000, -3.469446951953613696E-16 ) ) ;
#45356 = EDGE_CURVE ( 'NONE', #41290, #37129, #4324, .T. ) ;
#45357 = CARTESIAN_POINT ( 'NONE',  ( 0.2727639067037602172, 3.346456692913386100, -2.047244094488182231 ) ) ;
#45358 = CARTESIAN_POINT ( 'NONE',  ( -1.636583440222564301, 0.000000000000000000, -1.259842519685034468 ) ) ;
#45359 = CARTESIAN_POINT ( 'NONE',  ( 0.7090793742677682365, 0.03927686936677046714, 1.749277966691849429 ) ) ;
#45360 = FACE_OUTER_BOUND ( 'NONE', #20309, .T. ) ;
#45361 = ORIENTED_EDGE ( 'NONE', *, *, #27385, .F. ) ;
#45362 = DIRECTION ( 'NONE',  ( -3.469446951953613696E-16, 0.000000000000000000, -1.000000000000000000 ) ) ;
#45363 = DIRECTION ( 'NONE',  ( 1.000000000000000000, 0.000000000000000000, -3.469446951953613696E-16 ) ) ;
#45364 = EDGE_CURVE ( 'NONE', #508, #39624, #39439, .T. ) ;
#45365 = ORIENTED_EDGE ( 'NONE', *, *, #49938, .F. ) ;
#45366 = DIRECTION ( 'NONE',  ( -0.000000000000000000, 0.000000000000000000, 1.000000000000000000 ) ) ;
#45367 = ADVANCED_FACE ( 'NONE', ( #20055 ), #31441, .F. ) ;
#45368 = EDGE_CURVE ( 'NONE', #26820, #13480, #15937, .T. ) ;
#45369 = ORIENTED_EDGE ( 'NONE', *, *, #49254, .T. ) ;
#45370 = CARTESIAN_POINT ( 'NONE',  ( 0.1580252402616749152, 0.000000000000000000, -1.939804032141613899 ) ) ;
#45371 = DIRECTION ( 'NONE',  ( -0.000000000000000000, 0.000000000000000000, 1.000000000000000000 ) ) ;
#45372 = AXIS2_PLACEMENT_3D ( 'NONE', #1947, #44538, #21066 ) ;
#45373 = LINE ( 'NONE', #25012, #45987 ) ;
#45374 = CIRCLE ( 'NONE', #42906, 2.165354330708661568 ) ;
#45375 = CARTESIAN_POINT ( 'NONE',  ( 1.068402561569975484, 0.000000000000000000, -1.884154513482173554 ) ) ;
#45376 = LINE ( 'NONE', #33545, #50753 ) ;
#45377 = ORIENTED_EDGE ( 'NONE', *, *, #11167, .F. ) ;
#45378 = CARTESIAN_POINT ( 'NONE',  ( -1.942732458483407143, 5.905511811023623991, 2.223636218514597029 ) ) ;
#45379 = EDGE_LOOP ( 'NONE', ( #33961, #30448, #23349, #37304 ) ) ;
#45380 = ORIENTED_EDGE ( 'NONE', *, *, #24030, .T. ) ;
#45381 = CARTESIAN_POINT ( 'NONE',  ( 1.560669927219590747, 3.346456692913386100, 0.4724409448818871482 ) ) ;
#45382 = ORIENTED_EDGE ( 'NONE', *, *, #36631, .T. ) ;
#45383 = CARTESIAN_POINT ( 'NONE',  ( -1.364345965745727973, 1.205361022782829114E-17, 1.150974876880269893 ) ) ;
#45384 = CONICAL_SURFACE ( 'NONE', #13276, 2.246510896728926010, 0.01601546068027819014 ) ;
#45385 = CARTESIAN_POINT ( 'NONE',  ( -0.2727639067037607723, 0.000000000000000000, -1.102362204724405714 ) ) ;
#45386 = EDGE_LOOP ( 'NONE', ( #41488, #1408, #19865, #49304 ) ) ;
#45387 = DIRECTION ( 'NONE',  ( 0.000000000000000000, -1.000000000000000000, 0.000000000000000000 ) ) ;
#45388 = CARTESIAN_POINT ( 'NONE',  ( -0.8182917201112819283, 3.346456692913386100, -1.732283464566922726 ) ) ;
#45389 = CARTESIAN_POINT ( 'NONE',  ( -1.741986320419516954, 0.0003450591842249390597, 0.08333880254314324221 ) ) ;
#45390 = ORIENTED_EDGE ( 'NONE', *, *, #36473, .F. ) ;
#45391 = ORIENTED_EDGE ( 'NONE', *, *, #4351, .F. ) ;
#45392 = CARTESIAN_POINT ( 'NONE',  ( 0.000000000000000000, 3.267716535433071279, 0.9055118110236167750 ) ) ;
#45393 = FACE_BOUND ( 'NONE', #30701, .T. ) ;
#45394 = EDGE_LOOP ( 'NONE', ( #38809, #19091, #15198, #32517 ) ) ;
#45395 = FACE_OUTER_BOUND ( 'NONE', #21849, .T. ) ;
#45396 = CARTESIAN_POINT ( 'NONE',  ( -1.985260859929298238, 3.346456692913386100, -1.141732283464563791 ) ) ;
#45397 = EDGE_CURVE ( 'NONE', #5904, #17447, #451, .T. ) ;
#45398 = ORIENTED_EDGE ( 'NONE', *, *, #3587, .T. ) ;
#45399 = VERTEX_POINT ( 'NONE', #46889 ) ;
#45400 = DIRECTION ( 'NONE',  ( -1.000000000000000000, -0.000000000000000000, -0.000000000000000000 ) ) ;
#45401 = ADVANCED_FACE ( 'NONE', ( #16202 ), #23177, .T. ) ;
#45402 = EDGE_CURVE ( 'NONE', #5663, #8594, #38931, .T. ) ;
#45403 = CARTESIAN_POINT ( 'NONE',  ( 1.833433833923351353, 3.267716535433071279, -0.5118110236220471121 ) ) ;
#45404 = ORIENTED_EDGE ( 'NONE', *, *, #34091, .T. ) ;
#45405 = VERTEX_POINT ( 'NONE', #3563 ) ;
#45406 = ORIENTED_EDGE ( 'NONE', *, *, #36826, .F. ) ;
#45407 = CARTESIAN_POINT ( 'NONE',  ( -1.909347346926324462, 0.000000000000000000, 1.102362204724404160 ) ) ;
#45408 = VECTOR ( 'NONE', #32833, 39.37007874015748143 ) ;
#45409 = CARTESIAN_POINT ( 'NONE',  ( 2.579472588755252050E-16, 3.346456692913386100, 2.106299212598425008 ) ) ;
#45410 = VECTOR ( 'NONE', #2244, 39.37007874015748143 ) ;
#45411 = DIRECTION ( 'NONE',  ( 1.000000000000000000, 0.000000000000000000, 0.000000000000000000 ) ) ;
#45412 = CARTESIAN_POINT ( 'NONE',  ( -0.5756566573089010319, 5.905511811023623103, 2.896516654582635297 ) ) ;
#45413 = VERTEX_POINT ( 'NONE', #19297 ) ;
#45414 = VERTEX_POINT ( 'NONE', #50739 ) ;
#45415 = DIRECTION ( 'NONE',  ( 0.9998717552508121775, 0.01601477604151182663, 0.000000000000000000 ) ) ;
#45416 = LINE ( 'NONE', #17571, #31588 ) ;
#45417 = CONICAL_SURFACE ( 'NONE', #13315, 3.033577403570480779, 1.554780866114618743 ) ;
#45418 = ADVANCED_FACE ( 'NONE', ( #19550 ), #35319, .F. ) ;
#45419 = LINE ( 'NONE', #41076, #37523 ) ;
#45420 = DIRECTION ( 'NONE',  ( -1.000000000000000000, 0.000000000000000000, 0.000000000000000000 ) ) ;
#45421 = VECTOR ( 'NONE', #32192, 39.37007874015748143 ) ;
#45422 = EDGE_CURVE ( 'NONE', #23012, #12697, #50059, .T. ) ;
#45423 = CYLINDRICAL_SURFACE ( 'NONE', #26775, 2.164630168518208109 ) ;
#45424 = LINE ( 'NONE', #25827, #46473 ) ;
#45425 = VERTEX_POINT ( 'NONE', #15187 ) ;
#45426 = CARTESIAN_POINT ( 'NONE',  ( -0.6233543567505155369, 6.692913385826772199, -2.073689640095379705 ) ) ;
#45427 = CARTESIAN_POINT ( 'NONE',  ( 0.07982360342473591996, 1.709180471932028711, 0.000000000000000000 ) ) ;
#45428 = EDGE_CURVE ( 'NONE', #30012, #43842, #30937, .T. ) ;
#45429 = ORIENTED_EDGE ( 'NONE', *, *, #45612, .F. ) ;
#45430 = ORIENTED_EDGE ( 'NONE', *, *, #14029, .F. ) ;
#45431 = CARTESIAN_POINT ( 'NONE',  ( 2.793030215715258446, 1.762782749918499814, 0.9592557174602684977 ) ) ;
#45432 = ORIENTED_EDGE ( 'NONE', *, *, #8366, .F. ) ;
#45433 = VERTEX_POINT ( 'NONE', #22934 ) ;
#45434 = CARTESIAN_POINT ( 'NONE',  ( 1.287906020515830585, 3.267716535433071279, 1.377952755905504256 ) ) ;
#45435 = ORIENTED_EDGE ( 'NONE', *, *, #40309, .T. ) ;
#45436 = VECTOR ( 'NONE', #27782, 39.37007874015748143 ) ;
#45437 = DIRECTION ( 'NONE',  ( -1.000000000000000000, 0.000000000000000000, 0.000000000000000000 ) ) ;
#45438 = CARTESIAN_POINT ( 'NONE',  ( -0.6214413264104939882, 3.346456692913386100, 1.535433070866133898 ) ) ;
#45439 = VECTOR ( 'NONE', #3255, 39.37007874015748143 ) ;
#45440 = ORIENTED_EDGE ( 'NONE', *, *, #24793, .F. ) ;
#45441 = ORIENTED_EDGE ( 'NONE', *, *, #46252, .T. ) ;
#45442 = VECTOR ( 'NONE', #23115, 39.37007874015748143 ) ;
#45443 = CARTESIAN_POINT ( 'NONE',  ( 0.1968503937007872462, 3.267716535433071279, -0.8267716535433052849 ) ) ;
#45444 = VERTEX_POINT ( 'NONE', #23688 ) ;
#45445 = ORIENTED_EDGE ( 'NONE', *, *, #19726, .T. ) ;
#45446 = CARTESIAN_POINT ( 'NONE',  ( -0.8244711865321519006, 0.01471425056033665718, -1.598608591632243892 ) ) ;
#45447 = DIRECTION ( 'NONE',  ( 0.000000000000000000, 0.000000000000000000, 1.000000000000000000 ) ) ;
#45448 = VECTOR ( 'NONE', #10247, 39.37007874015748143 ) ;
#45449 = FACE_OUTER_BOUND ( 'NONE', #14098, .T. ) ;
#45450 = B_SPLINE_CURVE_WITH_KNOTS ( 'NONE', 3,
 ( #26144, #13766, #30017, #1886 ),
 .UNSPECIFIED., .F., .F.,
 ( 4, 4 ),
 ( 2.331048520511536045E-07, 0.002500624525913899138 ),
 .UNSPECIFIED. ) ;
#45451 = AXIS2_PLACEMENT_3D ( 'NONE', #19719, #35480, #12239 ) ;
#45452 = ORIENTED_EDGE ( 'NONE', *, *, #49323, .F. ) ;
#45453 = CARTESIAN_POINT ( 'NONE',  ( 0.8182917201112819283, 3.267716535433071279, 0.1574803149606286423 ) ) ;
#45454 = CARTESIAN_POINT ( 'NONE',  ( 0.000000000000000000, 3.267716535433071279, 0.000000000000000000 ) ) ;
#45455 = LINE ( 'NONE', #10376, #6409 ) ;
#45456 = ORIENTED_EDGE ( 'NONE', *, *, #46972, .T. ) ;
#45457 = CARTESIAN_POINT ( 'NONE',  ( 0.7423782071083085965, 0.000000000000000000, 0.7480314960629872445 ) ) ;
#45458 = LINE ( 'NONE', #14505, #30991 ) ;
#45459 = EDGE_CURVE ( 'NONE', #29978, #15353, #38687, .T. ) ;
#45460 = EDGE_CURVE ( 'NONE', #35067, #1831, #20585, .T. ) ;
#45461 = CARTESIAN_POINT ( 'NONE',  ( 2.093903048064389427, 0.000000000000000000, -0.4274415146361335571 ) ) ;
#45462 = VERTEX_POINT ( 'NONE', #28577 ) ;
#45463 = ORIENTED_EDGE ( 'NONE', *, *, #15683, .T. ) ;
#45464 = EDGE_CURVE ( 'NONE', #48582, #7654, #25224, .T. ) ;
#45465 = EDGE_CURVE ( 'NONE', #31969, #1849, #20578, .T. ) ;
#45466 = CARTESIAN_POINT ( 'NONE',  ( 2.182111253630085290, 3.346456692913386100, -0.5118110236220471121 ) ) ;
#45467 = CARTESIAN_POINT ( 'NONE',  ( 0.1968503937007877735, 3.267716535433071279, 1.062992125984246083 ) ) ;
#45468 = EDGE_CURVE ( 'NONE', #22488, #39500, #32215, .T. ) ;
#45469 = CARTESIAN_POINT ( 'NONE',  ( 0.8182917201112824834, 3.346456692913386100, 1.732283464566921172 ) ) ;
#45470 = VERTEX_POINT ( 'NONE', #16460 ) ;
#45471 = ORIENTED_EDGE ( 'NONE', *, *, #23704, .T. ) ;
#45472 = DIRECTION ( 'NONE',  ( -3.469446951953613696E-16, 0.000000000000000000, -1.000000000000000000 ) ) ;
#45473 = ORIENTED_EDGE ( 'NONE', *, *, #10997, .F. ) ;
#45474 = LINE ( 'NONE', #37517, #39794 ) ;
#45475 = CARTESIAN_POINT ( 'NONE',  ( 1.636583440222563857, 3.346456692913386100, 0.3149606299212576177 ) ) ;
#45476 = VECTOR ( 'NONE', #16882, 39.37007874015748143 ) ;
#45477 = VECTOR ( 'NONE', #3195, 39.37007874015748143 ) ;
#45478 = EDGE_CURVE ( 'NONE', #5602, #13181, #13104, .T. ) ;
#45479 = CARTESIAN_POINT ( 'NONE',  ( 0.5455278134075216556, 0.000000000000000000, 1.377952755905504256 ) ) ;
#45481 = DIRECTION ( 'NONE',  ( 0.000000000000000000, -1.000000000000000000, 0.000000000000000000 ) ) ;
#45480 = VECTOR ( 'NONE', #26548, 39.37007874015748143 ) ;
#45482 = ORIENTED_EDGE ( 'NONE', *, *, #23160, .F. ) ;
#45483 = LINE ( 'NONE', #9640, #50507 ) ;
#45484 = CARTESIAN_POINT ( 'NONE',  ( 0.000000000000000000, 3.267716535433071279, 0.000000000000000000 ) ) ;
#45485 = EDGE_CURVE ( 'NONE', #36932, #35018, #9481, .T. ) ;
#45486 = VECTOR ( 'NONE', #33945, 39.37007874015748143 ) ;
#45487 = LINE ( 'NONE', #10147, #8393 ) ;
#45488 = ORIENTED_EDGE ( 'NONE', *, *, #32686, .F. ) ;
#45489 = VECTOR ( 'NONE', #24560, 39.37007874015748143 ) ;
#45490 = DIRECTION ( 'NONE',  ( -0.9998717552508121775, -0.01601477604151185438, 0.000000000000000000 ) ) ;
#45491 = LINE ( 'NONE', #18155, #28614 ) ;
#45492 = FACE_OUTER_BOUND ( 'NONE', #29238, .T. ) ;
#45493 = VERTEX_POINT ( 'NONE', #965 ) ;
#45494 = CARTESIAN_POINT ( 'NONE',  ( 1.909347346926324462, 3.346456692913386100, -1.102362204724406602 ) ) ;
#45495 = ORIENTED_EDGE ( 'NONE', *, *, #47119, .T. ) ;
#45496 = PLANE ( 'NONE',  #17255 ) ;
#45497 = CARTESIAN_POINT ( 'NONE',  ( 1.080407128400152184, 1.049866565067838264, 1.712347114214678001 ) ) ;
#45498 = VERTEX_POINT ( 'NONE', #36083 ) ;
#45499 = CARTESIAN_POINT ( 'NONE',  ( -0.8221900955658372201, 5.905511811023623991, 2.050660405798877317 ) ) ;
#45500 = EDGE_CURVE ( 'NONE', #5175, #7776, #9221, .T. ) ;
#45501 = CARTESIAN_POINT ( 'NONE',  ( -0.2727639067037608278, 3.346456692913386100, -1.614173228346451605 ) ) ;
#45502 = CARTESIAN_POINT ( 'NONE',  ( 0.000000000000000000, 6.692913385826772199, 0.000000000000000000 ) ) ;
#45503 = DIRECTION ( 'NONE',  ( 1.000000000000000000, 0.000000000000000000, 0.000000000000000000 ) ) ;
#45504 = DIRECTION ( 'NONE',  ( 0.000000000000000000, 0.000000000000000000, -1.000000000000000000 ) ) ;
#45505 = ORIENTED_EDGE ( 'NONE', *, *, #27616, .T. ) ;
#45506 = VERTEX_POINT ( 'NONE', #4584 ) ;
#45507 = DIRECTION ( 'NONE',  ( -1.000000000000000000, -0.000000000000000000, -0.000000000000000000 ) ) ;
#45508 = CARTESIAN_POINT ( 'NONE',  ( 1.441820561149283586, 0.5249316497054297148, 1.212758805029070741 ) ) ;
#45509 = VERTEX_POINT ( 'NONE', #24463 ) ;
#45510 = CARTESIAN_POINT ( 'NONE',  ( -1.325491792074585451, 1.600165750963108646, -2.638988599164751481 ) ) ;
#45511 = CARTESIAN_POINT ( 'NONE',  ( 0.5455278134075212115, 3.346456692913386100, 0.6299212598425161236 ) ) ;
#45512 = DIRECTION ( 'NONE',  ( 1.734723475976806848E-16, -0.000000000000000000, 1.000000000000000000 ) ) ;
#45513 = ORIENTED_EDGE ( 'NONE', *, *, #48026, .F. ) ;
#45514 = CIRCLE ( 'NONE', #31532, 2.106299212598425008 ) ;
#45515 = ORIENTED_EDGE ( 'NONE', *, *, #43348, .T. ) ;
#45516 = DIRECTION ( 'NONE',  ( 1.734723475976806848E-16, 0.000000000000000000, 1.000000000000000000 ) ) ;
#45517 = PLANE ( 'NONE',  #3527 ) ;
#45518 = CARTESIAN_POINT ( 'NONE',  ( 0.000000000000000000, 3.267716535433071279, 1.850393700787391849 ) ) ;
#45519 = ORIENTED_EDGE ( 'NONE', *, *, #40884, .T. ) ;
#45520 = LINE ( 'NONE', #37311, #42188 ) ;
#45521 = VECTOR ( 'NONE', #45080, 39.37007874015748143 ) ;
#45522 = FACE_BOUND ( 'NONE', #4032, .T. ) ;
#45523 = VERTEX_POINT ( 'NONE', #8968 ) ;
#45524 = EDGE_CURVE ( 'NONE', #3116, #12576, #5091, .T. ) ;
#45525 = CARTESIAN_POINT ( 'NONE',  ( 0.000000000000000000, 3.267716535433071279, 1.417322834645662777 ) ) ;
#45526 = ORIENTED_EDGE ( 'NONE', *, *, #14715, .T. ) ;
#45527 = AXIS2_PLACEMENT_3D ( 'NONE', #31911, #35010, #399 ) ;
#45528 = ORIENTED_EDGE ( 'NONE', *, *, #2021, .T. ) ;
#45529 = CARTESIAN_POINT ( 'NONE',  ( 1.630393911741433000, 1.635590496292660179, -1.626902725537468619 ) ) ;
#45530 = EDGE_CURVE ( 'NONE', #47803, #8328, #35528, .T. ) ;
#45531 = DIRECTION ( 'NONE',  ( 1.000000000000000000, 0.000000000000000000, -3.469446951953613696E-16 ) ) ;
#45532 = EDGE_CURVE ( 'NONE', #924, #37147, #1472, .T. ) ;
#45533 = EDGE_LOOP ( 'NONE', ( #32117, #14090, #37105, #20599 ) ) ;
#45534 = DIRECTION ( 'NONE',  ( -3.469446951953613696E-16, 0.000000000000000000, -1.000000000000000000 ) ) ;
#45535 = ADVANCED_FACE ( 'NONE', ( #24721 ), #45384, .T. ) ;
#45536 = CARTESIAN_POINT ( 'NONE',  ( -0.4371342596750092402, -0.6299212598425202314, -1.309652049997256373 ) ) ;
#45537 = VERTEX_POINT ( 'NONE', #29085 ) ;
#45538 = VERTEX_POINT ( 'NONE', #1223 ) ;
#45539 = CARTESIAN_POINT ( 'NONE',  ( 0.8182917201112819283, 3.267716535433071279, -0.6692913385826764205 ) ) ;
#45540 = CARTESIAN_POINT ( 'NONE',  ( 1.526828301548457834, 3.346456692913386100, 1.535433070866133898 ) ) ;
#45541 = EDGE_CURVE ( 'NONE', #2720, #36292, #21102, .T. ) ;
#45542 = CARTESIAN_POINT ( 'NONE',  ( -2.099568260077699478, 5.905511811023623991, -0.5296909464896105701 ) ) ;
#45543 = DIRECTION ( 'NONE',  ( -1.000000000000000000, 0.000000000000000000, 1.734723475976806848E-16 ) ) ;
#45544 = DIRECTION ( 'NONE',  ( 0.8865472742777344983, 0.000000000000000000, 0.4626380123495249519 ) ) ;
#45545 = ORIENTED_EDGE ( 'NONE', *, *, #13584, .T. ) ;
#45546 = DIRECTION ( 'NONE',  ( -1.000000000000000000, 0.000000000000000000, 1.734723475976806848E-16 ) ) ;
#45547 = ADVANCED_FACE ( 'NONE', ( #28836 ), #24967, .F. ) ;
#45548 = B_SPLINE_CURVE_WITH_KNOTS ( 'NONE', 3,
 ( #35850, #1500, #13377, #44850 ),
 .UNSPECIFIED., .F., .F.,
 ( 4, 4 ),
 ( 0.0008755238761999696888, 0.001539766364033689182 ),
 .UNSPECIFIED. ) ;
#45549 = CARTESIAN_POINT ( 'NONE',  ( -0.9794755770252101534, 0.000000000000000000, 1.097585813245683051 ) ) ;
#45550 = VERTEX_POINT ( 'NONE', #20323 ) ;
#45551 = PLANE ( 'NONE',  #20708 ) ;
#45552 = CARTESIAN_POINT ( 'NONE',  ( 0.000000000000000000, 3.267716535433071279, 0.3149606299212578953 ) ) ;
#45553 = ORIENTED_EDGE ( 'NONE', *, *, #49241, .F. ) ;
#45554 = LINE ( 'NONE', #10220, #46845 ) ;
#45555 = EDGE_CURVE ( 'NONE', #9666, #9591, #17232, .T. ) ;
#45556 = CARTESIAN_POINT ( 'NONE',  ( 1.636583440222563857, 3.346456692913386100, 0.1181102362204701633 ) ) ;
#45557 = CARTESIAN_POINT ( 'NONE',  ( 0.000000000000000000, 3.267716535433071279, 1.850393700787392293 ) ) ;
#45558 = VECTOR ( 'NONE', #26429, 39.37007874015748143 ) ;
#45559 = ORIENTED_EDGE ( 'NONE', *, *, #48548, .T. ) ;
#45560 = DIRECTION ( 'NONE',  ( 0.000000000000000000, 0.000000000000000000, 1.000000000000000000 ) ) ;
#45561 = ORIENTED_EDGE ( 'NONE', *, *, #45905, .T. ) ;
#45562 = FACE_BOUND ( 'NONE', #21017, .T. ) ;
#45563 = EDGE_CURVE ( 'NONE', #1604, #8994, #37107, .T. ) ;
#45564 = CARTESIAN_POINT ( 'NONE',  ( 0.2727639067037605503, 3.267716535433071279, -4.731699523581609741E-17 ) ) ;
#45565 = VECTOR ( 'NONE', #25500, 39.37007874015748143 ) ;
#45566 = VECTOR ( 'NONE', #12412, 39.37007874015748143 ) ;
#45567 = CARTESIAN_POINT ( 'NONE',  ( 0.8182917201112823724, 3.267716535433071279, 1.940849049717691122 ) ) ;
#45568 = LINE ( 'NONE', #45069, #23501 ) ;
#45569 = ORIENTED_EDGE ( 'NONE', *, *, #10238, .T. ) ;
#45570 = ORIENTED_EDGE ( 'NONE', *, *, #46121, .T. ) ;
#45571 = VECTOR ( 'NONE', #1699, 39.37007874015748143 ) ;
#45572 = CARTESIAN_POINT ( 'NONE',  ( -2.823445274216743073, 1.573787237234608005, 0.8656477926280277124 ) ) ;
#45573 = ADVANCED_FACE ( 'NONE', ( #44823 ), #40984, .F. ) ;
#45574 = DIRECTION ( 'NONE',  ( -0.01601477604151182663, 0.9998717552508123996, -0.000000000000000000 ) ) ;
#45575 = ORIENTED_EDGE ( 'NONE', *, *, #50156, .T. ) ;
#45576 = ADVANCED_FACE ( 'NONE', ( #41989 ), #6108, .F. ) ;
#45577 = CARTESIAN_POINT ( 'NONE',  ( -0.5905738936209794510, 0.01846054376545745376, 1.713635781666723146 ) ) ;
#45578 = ORIENTED_EDGE ( 'NONE', *, *, #36695, .F. ) ;
#45579 = DIRECTION ( 'NONE',  ( -1.000000000000000000, 0.000000000000000000, -0.000000000000000000 ) ) ;
#45580 = CARTESIAN_POINT ( 'NONE',  ( 2.576863348864710801, 1.759415398959654819, 1.442554885838449819 ) ) ;
#45581 = ORIENTED_EDGE ( 'NONE', *, *, #26876, .T. ) ;
#45582 = CARTESIAN_POINT ( 'NONE',  ( -0.3136974817027969320, 1.205361022782829114E-17, -2.936457595020224520 ) ) ;
#45583 = ORIENTED_EDGE ( 'NONE', *, *, #2206, .F. ) ;
#45584 = ORIENTED_EDGE ( 'NONE', *, *, #50240, .T. ) ;
#45585 = EDGE_CURVE ( 'NONE', #35595, #3716, #13863, .T. ) ;
#45586 = EDGE_LOOP ( 'NONE', ( #22374, #33783, #28872, #38253 ) ) ;
#45587 = ORIENTED_EDGE ( 'NONE', *, *, #11000, .F. ) ;
#45588 = DIRECTION ( 'NONE',  ( 0.3930250316539147803, 0.000000000000000000, 0.9195277725514544587 ) ) ;
#45589 = EDGE_CURVE ( 'NONE', #32045, #19099, #29350, .T. ) ;
#45590 = B_SPLINE_CURVE_WITH_KNOTS ( 'NONE', 3,
 ( #25448, #22098, #29062, #25963 ),
 .UNSPECIFIED., .F., .F.,
 ( 4, 4 ),
 ( 0.0007385519321130311256, 0.003238853935468911406 ),
 .UNSPECIFIED. ) ;
#45591 = CIRCLE ( 'NONE', #44791, 2.244934639244525076 ) ;
#45592 = ORIENTED_EDGE ( 'NONE', *, *, #33232, .F. ) ;
#45593 = AXIS2_PLACEMENT_3D ( 'NONE', #3226, #47057, #18975 ) ;
#45594 = CARTESIAN_POINT ( 'NONE',  ( 1.388309139374679146, 1.631713065620022274, -1.827118126197171399 ) ) ;
#45595 = CARTESIAN_POINT ( 'NONE',  ( -0.8942052331142552601, 0.000000000000000000, -1.889763779527552146 ) ) ;
#45596 = CIRCLE ( 'NONE', #19228, 2.106299212598425008 ) ;
#45597 = VECTOR ( 'NONE', #37139, 39.37007874015748143 ) ;
#45598 = FACE_OUTER_BOUND ( 'NONE', #21223, .T. ) ;
#45599 = LINE ( 'NONE', #5628, #21190 ) ;
#45600 = DIRECTION ( 'NONE',  ( 5.500355109725658086E-17, -1.000000000000000000, 1.022137253806229789E-16 ) ) ;
#45601 = AXIS2_PLACEMENT_3D ( 'NONE', #36249, #43707, #616 ) ;
#45602 = ORIENTED_EDGE ( 'NONE', *, *, #21250, .T. ) ;
#45603 = CARTESIAN_POINT ( 'NONE',  ( 0.4932906694934566239, 1.621072181458971251, 2.442642652141415738 ) ) ;
#45604 = CARTESIAN_POINT ( 'NONE',  ( 0.000000000000000000, 6.692913385826772199, 0.000000000000000000 ) ) ;
#45605 = DIRECTION ( 'NONE',  ( 0.000000000000000000, 0.000000000000000000, -1.000000000000000000 ) ) ;
#45606 = DIRECTION ( 'NONE',  ( 0.000000000000000000, -1.000000000000000000, 0.000000000000000000 ) ) ;
#45607 = ORIENTED_EDGE ( 'NONE', *, *, #51039, .T. ) ;
#45608 = CARTESIAN_POINT ( 'NONE',  ( -1.363819533518803473, 0.000000000000000000, -0.3543307086614174151 ) ) ;
#45609 = CARTESIAN_POINT ( 'NONE',  ( 0.000000000000000000, 3.267716535433071279, 0.000000000000000000 ) ) ;
#45610 = EDGE_LOOP ( 'NONE', ( #14901, #10248, #37680, #20117 ) ) ;
#45611 = CARTESIAN_POINT ( 'NONE',  ( -0.8942052331142552601, 0.000000000000000000, -0.9448818897637760728 ) ) ;
#45612 = EDGE_CURVE ( 'NONE', #38164, #42095, #3383, .T. ) ;
#45613 = PLANE ( 'NONE',  #6160 ) ;
#45614 = VERTEX_POINT ( 'NONE', #9985 ) ;
#45615 = ORIENTED_EDGE ( 'NONE', *, *, #28452, .F. ) ;
#45616 = FACE_OUTER_BOUND ( 'NONE', #42909, .T. ) ;
#45617 = EDGE_CURVE ( 'NONE', #17233, #9022, #23038, .T. ) ;
#45618 = LINE ( 'NONE', #29654, #6932 ) ;
#45619 = CARTESIAN_POINT ( 'NONE',  ( -1.216396646496118228, 1.593988306679904321, 2.131854889095133654 ) ) ;
#45620 = EDGE_CURVE ( 'NONE', #33927, #2475, #38014, .T. ) ;
#45621 = CARTESIAN_POINT ( 'NONE',  ( -2.919426793319806368, 1.673754417692067564, 0.4451252810446391095 ) ) ;
#45622 = DIRECTION ( 'NONE',  ( -1.000000000000000000, 0.000000000000000000, -0.000000000000000000 ) ) ;
#45623 = VERTEX_POINT ( 'NONE', #48920 ) ;
#45624 = EDGE_CURVE ( 'NONE', #7189, #13035, #9960, .T. ) ;
#45625 = DIRECTION ( 'NONE',  ( 8.741157232058135226E-17, -1.000000000000000000, 7.636919086868543885E-17 ) ) ;
#45626 = AXIS2_PLACEMENT_3D ( 'NONE', #45785, #25424, #29562 ) ;
#45627 = EDGE_LOOP ( 'NONE', ( #35630, #44532, #16979, #29713 ) ) ;
#45628 = ORIENTED_EDGE ( 'NONE', *, *, #22757, .T. ) ;
#45629 = CARTESIAN_POINT ( 'NONE',  ( 0.000000000000000000, 6.692913385826772199, 0.000000000000000000 ) ) ;
#45630 = EDGE_LOOP ( 'NONE', ( #4314, #3442, #15622, #48497, #30612, #26001, #23424, #27680 ) ) ;
#45631 = LINE ( 'NONE', #38430, #37831 ) ;
#45632 = LINE ( 'NONE', #37682, #15338 ) ;
#45633 = ORIENTED_EDGE ( 'NONE', *, *, #44992, .T. ) ;
#45634 = AXIS2_PLACEMENT_3D ( 'NONE', #32669, #29021, #28769 ) ;
#45635 = AXIS2_PLACEMENT_3D ( 'NONE', #28673, #25068, #8804 ) ;
#45636 = CARTESIAN_POINT ( 'NONE',  ( -1.636583440222564301, 0.000000000000000000, -1.259842519685034468 ) ) ;
#45637 = LINE ( 'NONE', #29413, #7590 ) ;
#45638 = EDGE_CURVE ( 'NONE', #50546, #40954, #14366, .T. ) ;
#45639 = AXIS2_PLACEMENT_3D ( 'NONE', #47237, #28415, #40047 ) ;
#45640 = PLANE ( 'NONE',  #47731 ) ;
#45641 = EDGE_LOOP ( 'NONE', ( #27765, #12862, #1294, #38864 ) ) ;
#45642 = ORIENTED_EDGE ( 'NONE', *, *, #2990, .F. ) ;
#45643 = DIRECTION ( 'NONE',  ( -1.000000000000000000, 0.000000000000000000, 1.734723475976806848E-16 ) ) ;
#45644 = FACE_OUTER_BOUND ( 'NONE', #20350, .T. ) ;
#45645 = ORIENTED_EDGE ( 'NONE', *, *, #40780, .T. ) ;
#45646 = EDGE_CURVE ( 'NONE', #32620, #28023, #10239, .T. ) ;
#45647 = CARTESIAN_POINT ( 'NONE',  ( -1.774034721664383030, 0.5252446251211232431, -1.229997447203279082 ) ) ;
#45648 = DIRECTION ( 'NONE',  ( 1.734723475976806848E-16, -0.000000000000000000, 1.000000000000000000 ) ) ;
#45649 = VERTEX_POINT ( 'NONE', #49185 ) ;
#45650 = ORIENTED_EDGE ( 'NONE', *, *, #8440, .F. ) ;
#45651 = EDGE_CURVE ( 'NONE', #22497, #20299, #21866, .T. ) ;
#45652 = CARTESIAN_POINT ( 'NONE',  ( -1.636583440222563635, 3.346456692913386100, 1.259842519685033357 ) ) ;
#45653 = DIRECTION ( 'NONE',  ( -0.000000000000000000, 1.000000000000000000, -0.000000000000000000 ) ) ;
#45654 = ORIENTED_EDGE ( 'NONE', *, *, #31133, .T. ) ;
#45655 = ORIENTED_EDGE ( 'NONE', *, *, #26996, .F. ) ;
#45656 = ORIENTED_EDGE ( 'NONE', *, *, #43708, .T. ) ;
#45657 = DIRECTION ( 'NONE',  ( -1.000000000000000000, 0.000000000000000000, 1.734723475976806848E-16 ) ) ;
#45658 = CARTESIAN_POINT ( 'NONE',  ( -1.985260859929298016, 3.346456692913386100, -0.9448818897637762948 ) ) ;
#45659 = CARTESIAN_POINT ( 'NONE',  ( -0.2177357222769329415, 0.008167984067341605911, -1.870235122269071182 ) ) ;
#45660 = DIRECTION ( 'NONE',  ( -0.9998717552508122886, -0.01601477604151185785, 0.000000000000000000 ) ) ;
#45661 = B_SPLINE_CURVE_WITH_KNOTS ( 'NONE', 3,
 ( #16136, #32408, #40410, #40151 ),
 .UNSPECIFIED., .F., .F.,
 ( 4, 4 ),
 ( 0.01387794258156342664, 0.03074578613037699110 ),
 .UNSPECIFIED. ) ;
#45662 = ORIENTED_EDGE ( 'NONE', *, *, #43563, .T. ) ;
#45663 = EDGE_LOOP ( 'NONE', ( #29001, #36424, #25879, #16675 ) ) ;
#45664 = PRODUCT_DEFINITION_FORMATION_WITH_SPECIFIED_SOURCE ( 'ANY', '', #8350, .NOT_KNOWN. ) ;
#45665 = CARTESIAN_POINT ( 'NONE',  ( -0.07591351300297277671, 3.346456692913386100, 1.417322834645662777 ) ) ;
#45666 = CARTESIAN_POINT ( 'NONE',  ( -1.712496953225537188, 0.000000000000000000, -0.03937007874015881204 ) ) ;
#45667 = CARTESIAN_POINT ( 'NONE',  ( 1.909347346926324462, 0.000000000000000000, -1.102362204724406602 ) ) ;
#45668 = VECTOR ( 'NONE', #37865, 39.37007874015748143 ) ;
#45669 = CARTESIAN_POINT ( 'NONE',  ( -0.07591351300297359550, 3.346456692913386100, -2.047244094488181343 ) ) ;
#45670 = VECTOR ( 'NONE', #19156, 39.37007874015748143 ) ;
#45671 = LINE ( 'NONE', #33081, #22336 ) ;
#45672 = CIRCLE ( 'NONE', #48971, 2.165354330708661568 ) ;
#45673 = LINE ( 'NONE', #26082, #20169 ) ;
#45674 = LINE ( 'NONE', #34597, #6124 ) ;
#45675 = VECTOR ( 'NONE', #8497, 39.37007874015748143 ) ;
#45676 = EDGE_LOOP ( 'NONE', ( #21985, #28674 ) ) ;
#45677 = LINE ( 'NONE', #26583, #3613 ) ;
#45678 = CARTESIAN_POINT ( 'NONE',  ( -0.6214413264104939882, 0.000000000000000000, 0.7874015748031456541 ) ) ;
#45679 = ORIENTED_EDGE ( 'NONE', *, *, #30428, .F. ) ;
#45680 = ORIENTED_EDGE ( 'NONE', *, *, #24751, .F. ) ;
#45681 = CARTESIAN_POINT ( 'NONE',  ( 0.7148041136150539154, 6.692913385826772199, -2.044646019095610612 ) ) ;
#45682 = EDGE_CURVE ( 'NONE', #28536, #24717, #884, .T. ) ;
#45683 = EDGE_LOOP ( 'NONE', ( #34494, #29721, #28612 ) ) ;
#45684 = EDGE_CURVE ( 'NONE', #50196, #35952, #14110, .T. ) ;
#45685 = B_SPLINE_CURVE_WITH_KNOTS ( 'NONE', 3,
 ( #34148, #30266, #45982, #18649 ),
 .UNSPECIFIED., .F., .F.,
 ( 4, 4 ),
 ( 2.176057262996888679E-07, 0.01608855240560840352 ),
 .UNSPECIFIED. ) ;
#45686 = EDGE_CURVE ( 'NONE', #49770, #45076, #22318, .T. ) ;
#45687 = ORIENTED_EDGE ( 'NONE', *, *, #483, .F. ) ;
#45688 = CARTESIAN_POINT ( 'NONE',  ( 0.5455278134075208785, 0.000000000000000000, -1.574803149606293529 ) ) ;
#45689 = ORIENTED_EDGE ( 'NONE', *, *, #17019, .T. ) ;
#45690 = EDGE_CURVE ( 'NONE', #32424, #27097, #10744, .T. ) ;
#45691 = FACE_OUTER_BOUND ( 'NONE', #20429, .T. ) ;
#45692 = CARTESIAN_POINT ( 'NONE',  ( -1.152568299495734694, 6.692913385826772199, 1.833124570921535801 ) ) ;
#45693 = ORIENTED_EDGE ( 'NONE', *, *, #5890, .T. ) ;
#45694 = EDGE_LOOP ( 'NONE', ( #44445, #130, #38795, #13311 ) ) ;
#45695 = FACE_OUTER_BOUND ( 'NONE', #4103, .T. ) ;
#45696 = VECTOR ( 'NONE', #44227, 39.37007874015748143 ) ;
#45697 = ORIENTED_EDGE ( 'NONE', *, *, #43892, .F. ) ;
#45698 = EDGE_LOOP ( 'NONE', ( #23054, #1231, #22440, #3992 ) ) ;
#45699 = AXIS2_PLACEMENT_3D ( 'NONE', #31278, #27636, #35655 ) ;
#45700 = DIRECTION ( 'NONE',  ( 1.000000000000000000, 0.000000000000000000, -3.469446951953613696E-16 ) ) ;
#45701 = CARTESIAN_POINT ( 'NONE',  ( -0.9149808212874269708, 1.594821661612501940, -2.013400720915880626 ) ) ;
#45702 = CARTESIAN_POINT ( 'NONE',  ( -1.556712866041156440, 1.596563264426776207, 2.509548638715847435 ) ) ;
#45703 = DIRECTION ( 'NONE',  ( 1.000000000000000000, 0.000000000000000000, 0.000000000000000000 ) ) ;
#45704 = EDGE_CURVE ( 'NONE', #43511, #17939, #26483, .T. ) ;
#45705 = AXIS2_PLACEMENT_3D ( 'NONE', #47896, #15926, #20830 ) ;
#45706 = VECTOR ( 'NONE', #17014, 39.37007874015748143 ) ;
#45707 = ORIENTED_EDGE ( 'NONE', *, *, #41500, .F. ) ;
#45708 = ADVANCED_FACE ( 'NONE', ( #33998 ), #14084, .T. ) ;
#45709 = LINE ( 'NONE', #21995, #13122 ) ;
#45710 = DIRECTION ( 'NONE',  ( -0.000000000000000000, 1.000000000000000000, -0.000000000000000000 ) ) ;
#45711 = CARTESIAN_POINT ( 'NONE',  ( -1.183645401082143778, 0.000000000000000000, 1.279993023352344439 ) ) ;
#45712 = ORIENTED_EDGE ( 'NONE', *, *, #23612, .F. ) ;
#45713 = EDGE_CURVE ( 'NONE', #41147, #23660, #18213, .T. ) ;
#45714 = DIRECTION ( 'NONE',  ( -1.000000000000000000, 0.000000000000000000, 1.734723475976806848E-16 ) ) ;
#45715 = CARTESIAN_POINT ( 'NONE',  ( 0.4696143004045484348, 0.000000000000000000, 0.9055118110236167750 ) ) ;
#45716 = VECTOR ( 'NONE', #32982, 39.37007874015748143 ) ;
#45717 = ADVANCED_FACE ( 'NONE', ( #21607 ), #44579, .T. ) ;
#45718 = DIRECTION ( 'NONE',  ( -1.000000000000000000, 0.000000000000000000, 0.000000000000000000 ) ) ;
#45719 = ORIENTED_EDGE ( 'NONE', *, *, #41814, .T. ) ;
#45720 = ORIENTED_EDGE ( 'NONE', *, *, #43425, .F. ) ;
#45721 = EDGE_CURVE ( 'NONE', #19187, #49634, #17734, .T. ) ;
#45722 = FACE_OUTER_BOUND ( 'NONE', #13946, .T. ) ;
#45723 = DIRECTION ( 'NONE',  ( 0.000000000000000000, 0.000000000000000000, -1.000000000000000000 ) ) ;
#45724 = CARTESIAN_POINT ( 'NONE',  ( -1.057143431661240696, 3.346456692913386100, 1.889763779527550147 ) ) ;
#45725 = ORIENTED_EDGE ( 'NONE', *, *, #10772, .F. ) ;
#45726 = ORIENTED_EDGE ( 'NONE', *, *, #4675, .T. ) ;
#45727 = LINE ( 'NONE', #22268, #8658 ) ;
#45728 = VERTEX_POINT ( 'NONE', #7131 ) ;
#45729 = DIRECTION ( 'NONE',  ( 1.000000000000000000, 0.000000000000000000, -3.469446951953613696E-16 ) ) ;
#45730 = CARTESIAN_POINT ( 'NONE',  ( 0.4788131938641105312, 5.905511811023623103, 2.914091152102192162 ) ) ;
#45731 = CARTESIAN_POINT ( 'NONE',  ( 1.560669927219590747, 3.346456692913386100, 0.7874015748031454320 ) ) ;
#45732 = DIRECTION ( 'NONE',  ( 0.000000000000000000, 0.000000000000000000, 1.000000000000000000 ) ) ;
#45733 = DIRECTION ( 'NONE',  ( 0.000000000000000000, 0.000000000000000000, -1.000000000000000000 ) ) ;
#45734 = ORIENTED_EDGE ( 'NONE', *, *, #38497, .T. ) ;
#45735 = AXIS2_PLACEMENT_3D ( 'NONE', #26881, #26141, #23266 ) ;
#45736 = FACE_OUTER_BOUND ( 'NONE', #40931, .T. ) ;
#45737 = LINE ( 'NONE', #44987, #16168 ) ;
#45738 = VECTOR ( 'NONE', #48149, 39.37007874015748143 ) ;
#45739 = CIRCLE ( 'NONE', #49844, 2.106299212598425008 ) ;
#45740 = CARTESIAN_POINT ( 'NONE',  ( -2.298335196414549308, 1.562647740231880134, 1.853831591542948853 ) ) ;
#45741 = AXIS2_PLACEMENT_3D ( 'NONE', #42966, #15112, #50175 ) ;
#45742 = VERTEX_POINT ( 'NONE', #19745 ) ;
#45743 = CARTESIAN_POINT ( 'NONE',  ( -0.07591351300297340121, 3.346456692913386100, 2.165354330708650465 ) ) ;
#45744 = CARTESIAN_POINT ( 'NONE',  ( 0.1155636338427008941, -0.5222242541845523167, 0.000000000000000000 ) ) ;
#45745 = DIRECTION ( 'NONE',  ( -0.000000000000000000, 1.000000000000000000, -0.000000000000000000 ) ) ;
#45746 = EDGE_LOOP ( 'NONE', ( #24649, #34995, #27337, #37284 ) ) ;
#45747 = FACE_OUTER_BOUND ( 'NONE', #3316, .T. ) ;
#45748 = ADVANCED_FACE ( 'NONE', ( #26737 ), #7382, .F. ) ;
#45749 = CIRCLE ( 'NONE', #17771, 1.850107469027523432 ) ;
#45750 = ADVANCED_FACE ( 'NONE', ( #3504 ), #39655, .T. ) ;
#45751 = ORIENTED_EDGE ( 'NONE', *, *, #44147, .F. ) ;
#45752 = DIRECTION ( 'NONE',  ( -0.000000000000000000, -1.000000000000000000, -0.000000000000000000 ) ) ;
#45753 = DIRECTION ( 'NONE',  ( -0.000000000000000000, 1.000000000000000000, -0.000000000000000000 ) ) ;
#45754 = EDGE_LOOP ( 'NONE', ( #40823, #33006, #43190, #48789 ) ) ;
#45755 = DIRECTION ( 'NONE',  ( 1.000000000000000000, 0.000000000000000000, -3.469446951953613696E-16 ) ) ;
#45756 = EDGE_CURVE ( 'NONE', #48407, #6577, #18009, .T. ) ;
#45757 = CARTESIAN_POINT ( 'NONE',  ( 1.892591856222374469, 0.05823298773025239322, -0.4824499329568616157 ) ) ;
#45758 = PLANE ( 'NONE',  #28821 ) ;
#45759 = CARTESIAN_POINT ( 'NONE',  ( 0.2727639067037602172, 3.346456692913386100, -2.244094488188969727 ) ) ;
#45760 = ORIENTED_EDGE ( 'NONE', *, *, #5928, .F. ) ;
#45761 = ORIENTED_EDGE ( 'NONE', *, *, #17395, .F. ) ;
#45762 = CARTESIAN_POINT ( 'NONE',  ( 0.6235241006192022706, 0.000000000000000000, 2.074304693190358151 ) ) ;
#45763 = CARTESIAN_POINT ( 'NONE',  ( 0.8182917201112823724, 3.346456692913386100, 1.940849049717691122 ) ) ;
#45764 = VERTEX_POINT ( 'NONE', #22873 ) ;
#45765 = DIRECTION ( 'NONE',  ( 0.000000000000000000, 0.000000000000000000, -1.000000000000000000 ) ) ;
#45766 = CARTESIAN_POINT ( 'NONE',  ( 0.7423782071083087075, 3.346456692913386100, -0.9448818897637765168 ) ) ;
#45767 = CARTESIAN_POINT ( 'NONE',  ( 0.1155636338427008941, -0.5222242541845523167, 0.000000000000000000 ) ) ;
#45768 = ORIENTED_EDGE ( 'NONE', *, *, #27564, .T. ) ;
#45769 = VERTEX_POINT ( 'NONE', #34501 ) ;
#45770 = EDGE_CURVE ( 'NONE', #48829, #39458, #46222, .T. ) ;
#45771 = CARTESIAN_POINT ( 'NONE',  ( -2.167711126757420725, 3.254047560071126721, -1.141732283464563791 ) ) ;
#45772 = CARTESIAN_POINT ( 'NONE',  ( 0.9671406142315196464, 3.267716535433070391, -2.244094488188969283 ) ) ;
#45773 = LINE ( 'NONE', #6315, #1639 ) ;
#45774 = ORIENTED_EDGE ( 'NONE', *, *, #16932, .T. ) ;
#45775 = DIRECTION ( 'NONE',  ( 1.000000000000000000, 0.000000000000000000, 0.000000000000000000 ) ) ;
#45776 = CARTESIAN_POINT ( 'NONE',  ( 1.287906020515830141, 3.346456692913386100, 0.6299212598425161236 ) ) ;
#45777 = AXIS2_PLACEMENT_3D ( 'NONE', #33654, #25635, #41389 ) ;
#45778 = VERTEX_POINT ( 'NONE', #23120 ) ;
#45779 = ADVANCED_FACE ( 'NONE', ( #50188 ), #19239, .F. ) ;
#45780 = ADVANCED_FACE ( 'NONE', ( #23627 ), #39378, .F. ) ;
#45781 = CARTESIAN_POINT ( 'NONE',  ( -0.5455278134075208785, 3.267716535433071279, 0.9448818897637749625 ) ) ;
#45782 = ORIENTED_EDGE ( 'NONE', *, *, #30853, .F. ) ;
#45783 = ORIENTED_EDGE ( 'NONE', *, *, #16762, .F. ) ;
#45784 = PLANE ( 'NONE',  #47637 ) ;
#45785 = CARTESIAN_POINT ( 'NONE',  ( 1.091055626815042423, 0.000000000000000000, -1.771653543307081691 ) ) ;
#45786 = CIRCLE ( 'NONE', #35083, 2.165354330708661568 ) ;
#45787 = LINE ( 'NONE', #41691, #33036 ) ;
#45788 = VECTOR ( 'NONE', #17353, 39.37007874015748143 ) ;
#45789 = ORIENTED_EDGE ( 'NONE', *, *, #17489, .T. ) ;
#45790 = CARTESIAN_POINT ( 'NONE',  ( -1.936609506549060722, 1.676883605369557051, 0.9862484270667263297 ) ) ;
#45791 = LINE ( 'NONE', #6066, #37867 ) ;
#45792 = ORIENTED_EDGE ( 'NONE', *, *, #19024, .T. ) ;
#45793 = AXIS2_PLACEMENT_3D ( 'NONE', #11678, #26911, #38310 ) ;
#45794 = ORIENTED_EDGE ( 'NONE', *, *, #46353, .F. ) ;
#45795 = CARTESIAN_POINT ( 'NONE',  ( 0.1170985530868079300, 0.02979521312206013725, -1.850078377359382298 ) ) ;
#45796 = DIRECTION ( 'NONE',  ( 0.9998717552508121775, 0.01601477604151182663, 0.000000000000000000 ) ) ;
#45797 = LINE ( 'NONE', #10460, #9127 ) ;
#45798 = CARTESIAN_POINT ( 'NONE',  ( -1.636583440222563635, 3.267716535433071279, 0.6299212598425164567 ) ) ;
#45799 = LINE ( 'NONE', #1697, #5575 ) ;
#45800 = EDGE_LOOP ( 'NONE', ( #31678, #8772, #14230, #12532 ) ) ;
#45801 = CARTESIAN_POINT ( 'NONE',  ( 0.5455278134075211005, 0.000000000000000000, 0.7480314960629872445 ) ) ;
#45802 = CARTESIAN_POINT ( 'NONE',  ( 0.7423782071083091516, 3.267716535433071279, -2.575641807848711673E-16 ) ) ;
#45803 = VERTEX_POINT ( 'NONE', #35002 ) ;
#45804 = CARTESIAN_POINT ( 'NONE',  ( -1.195183497228115035E-16, 3.346456692913386100, -0.9448818897637765168 ) ) ;
#45805 = DIRECTION ( 'NONE',  ( 0.000000000000000000, 0.000000000000000000, 1.000000000000000000 ) ) ;
#45806 = ORIENTED_EDGE ( 'NONE', *, *, #9276, .T. ) ;
#45807 = CARTESIAN_POINT ( 'NONE',  ( 2.100403847690402337, 3.267716535433071279, -0.1574803149606304187 ) ) ;
#45808 = CARTESIAN_POINT ( 'NONE',  ( -0.5905738936209794510, 0.01846054376545745376, 1.713635781666723146 ) ) ;
#45809 = CARTESIAN_POINT ( 'NONE',  ( 0.8013393943173970912, 1.496885474212027223, -2.841987189051758733 ) ) ;
#45810 = EDGE_CURVE ( 'NONE', #41705, #30522, #37133, .T. ) ;
#45811 = AXIS2_PLACEMENT_3D ( 'NONE', #14531, #34908, #45993 ) ;
#45812 = EDGE_CURVE ( 'NONE', #4242, #27610, #42736, .T. ) ;
#45813 = CIRCLE ( 'NONE', #49918, 1.181102362204723200 ) ;
#45814 = ORIENTED_EDGE ( 'NONE', *, *, #28824, .F. ) ;
#45815 = CARTESIAN_POINT ( 'NONE',  ( 0.08119777152254364916, 1.623385212329073957, 0.000000000000000000 ) ) ;
#45816 = EDGE_LOOP ( 'NONE', ( #15010, #4607, #873, #13835 ) ) ;
#45817 = FACE_BOUND ( 'NONE', #42305, .T. ) ;
#45818 = VECTOR ( 'NONE', #8391, 39.37007874015748143 ) ;
#45819 = ADVANCED_FACE ( 'NONE', ( #127 ), #50681, .T. ) ;
#45820 = LINE ( 'NONE', #37353, #15181 ) ;
#45821 = CARTESIAN_POINT ( 'NONE',  ( 1.287906020515830585, 0.000000000000000000, 1.574803149606291974 ) ) ;
#45823 = EDGE_CURVE ( 'NONE', #40070, #26463, #14875, .T. ) ;
#45822 = LINE ( 'NONE', #34241, #41653 ) ;
#45824 = AXIS2_PLACEMENT_3D ( 'NONE', #27950, #50879, #46531 ) ;
#45825 = EDGE_CURVE ( 'NONE', #34034, #1329, #11506, .T. ) ;
#45826 = VECTOR ( 'NONE', #6625, 39.37007874015747433 ) ;
#45827 = ORIENTED_EDGE ( 'NONE', *, *, #35245, .F. ) ;
#45828 = ORIENTED_EDGE ( 'NONE', *, *, #32940, .T. ) ;
#45829 = PLANE ( 'NONE',  #4854 ) ;
#45830 = CARTESIAN_POINT ( 'NONE',  ( -0.1227720337126170513, 0.000000000000000000, -1.913115909999223652 ) ) ;
#45831 = DIRECTION ( 'NONE',  ( 1.000000000000000000, 0.000000000000000000, 0.000000000000000000 ) ) ;
#45832 = ORIENTED_EDGE ( 'NONE', *, *, #10913, .F. ) ;
#45833 = CARTESIAN_POINT ( 'NONE',  ( 0.07982360342473591996, 1.709180471932028711, 0.000000000000000000 ) ) ;
#45834 = EDGE_CURVE ( 'NONE', #9679, #23187, #31634, .T. ) ;
#45835 = VERTEX_POINT ( 'NONE', #19493 ) ;
#45836 = DIRECTION ( 'NONE',  ( -3.469446951953613696E-16, 0.000000000000000000, -1.000000000000000000 ) ) ;
#45837 = CARTESIAN_POINT ( 'NONE',  ( -1.909347346926324462, 0.000000000000000000, 0.1574803149606286423 ) ) ;
#45838 = EDGE_LOOP ( 'NONE', ( #20508, #31192, #35105, #18185 ) ) ;
#45839 = EDGE_CURVE ( 'NONE', #16948, #7950, #35255, .T. ) ;
#45840 = LINE ( 'NONE', #14117, #29823 ) ;
#45841 = VERTEX_POINT ( 'NONE', #15631 ) ;
#45842 = ORIENTED_EDGE ( 'NONE', *, *, #48309, .F. ) ;
#45843 = EDGE_CURVE ( 'NONE', #43652, #39871, #30620, .T. ) ;
#45844 = AXIS2_PLACEMENT_3D ( 'NONE', #34154, #49837, #50583 ) ;
#45845 = EDGE_LOOP ( 'NONE', ( #33579, #3570, #46312, #40706 ) ) ;
#45846 = ORIENTED_EDGE ( 'NONE', *, *, #28330, .T. ) ;
#45847 = DIRECTION ( 'NONE',  ( -1.206139481778042838E-16, 1.000000000000000000, 4.526717189434675613E-17 ) ) ;
#45848 = VECTOR ( 'NONE', #18601, 39.37007874015748143 ) ;
#45849 = AXIS2_PLACEMENT_3D ( 'NONE', #27828, #39714, #35843 ) ;
#45850 = ORIENTED_EDGE ( 'NONE', *, *, #18099, .F. ) ;
#45851 = CARTESIAN_POINT ( 'NONE',  ( -1.439733046521776583, 3.346456692913386100, -1.617383112398506295 ) ) ;
#45852 = EDGE_CURVE ( 'NONE', #26317, #49734, #47078, .T. ) ;
#45853 = AXIS2_PLACEMENT_3D ( 'NONE', #48859, #45018, #29545 ) ;
#45854 = DIRECTION ( 'NONE',  ( -0.000000000000000000, 1.000000000000000000, -0.000000000000000000 ) ) ;
#45855 = VECTOR ( 'NONE', #38422, 39.37007874015748143 ) ;
#45856 = LINE ( 'NONE', #26261, #9952 ) ;
#45857 = VECTOR ( 'NONE', #20774, 39.37007874015748143 ) ;
#45858 = CARTESIAN_POINT ( 'NONE',  ( 1.358062732265305605, 1.638351821497108451, 2.368963978111557456 ) ) ;
#45859 = CARTESIAN_POINT ( 'NONE',  ( -1.195183497228115035E-16, 3.346456692913386100, 0.3149606299212576177 ) ) ;
#45860 = ORIENTED_EDGE ( 'NONE', *, *, #28206, .T. ) ;
#45861 = DIRECTION ( 'NONE',  ( -3.469446951953613696E-16, 0.000000000000000000, -1.000000000000000000 ) ) ;
#45862 = CARTESIAN_POINT ( 'NONE',  ( -0.6214413264104945434, 0.000000000000000000, -0.1574803149606301411 ) ) ;
#45863 = CARTESIAN_POINT ( 'NONE',  ( -0.7680117299321171931, 1.703413802931311283, -2.597843860071421762 ) ) ;
#45864 = CARTESIAN_POINT ( 'NONE',  ( -0.4350747367504791963, 6.692913385826772199, -2.121846421795420934 ) ) ;
#45865 = ORIENTED_EDGE ( 'NONE', *, *, #32530, .T. ) ;
#45866 = CARTESIAN_POINT ( 'NONE',  ( 1.574803149606299524, 1.172985819482487146, -3.149606299212598159 ) ) ;
#45867 = CARTESIAN_POINT ( 'NONE',  ( 0.000000000000000000, 3.346456692913386100, 0.000000000000000000 ) ) ;
#45868 = VERTEX_POINT ( 'NONE', #25163 ) ;
#45869 = CARTESIAN_POINT ( 'NONE',  ( -2.182111253630085734, 3.346456692913386100, -1.141732283464563791 ) ) ;
#45870 = FACE_OUTER_BOUND ( 'NONE', #4922, .T. ) ;
#45871 = ORIENTED_EDGE ( 'NONE', *, *, #4916, .F. ) ;
#45872 = ORIENTED_EDGE ( 'NONE', *, *, #11493, .T. ) ;
#45873 = LINE ( 'NONE', #31174, #20659 ) ;
#45874 = EDGE_CURVE ( 'NONE', #12583, #33355, #24399, .T. ) ;
#45875 = CARTESIAN_POINT ( 'NONE',  ( -0.8182917201112819283, 3.267716535433071279, -1.102362204724405492 ) ) ;
#45876 = B_SPLINE_CURVE_WITH_KNOTS ( 'NONE', 3,
 ( #22856, #45809, #26221, #38108 ),
 .UNSPECIFIED., .F., .F.,
 ( 4, 4 ),
 ( 2.074235228680312165E-07, 0.002500790534950076988 ),
 .UNSPECIFIED. ) ;
#45877 = FACE_OUTER_BOUND ( 'NONE', #19858, .T. ) ;
#45878 = PLANE ( 'NONE',  #25953 ) ;
#45879 = CARTESIAN_POINT ( 'NONE',  ( -0.5455278134075214336, 3.267716535433071279, -0.3149606299212593941 ) ) ;
#45880 = VERTEX_POINT ( 'NONE', #36025 ) ;
#45881 = VECTOR ( 'NONE', #17203, 39.37007874015748143 ) ;
#45882 = ADVANCED_FACE ( 'NONE', ( #13040 ), #28772, .T. ) ;
#45883 = CARTESIAN_POINT ( 'NONE',  ( -1.979793062125317471, 0.000000000000000000, 2.191257344206539504 ) ) ;
#45884 = AXIS2_PLACEMENT_3D ( 'NONE', #8736, #47426, #20083 ) ;
#45885 = ORIENTED_EDGE ( 'NONE', *, *, #40130, .T. ) ;
#45886 = ORIENTED_EDGE ( 'NONE', *, *, #30434, .T. ) ;
#45887 = LINE ( 'NONE', #11555, #8943 ) ;
#45888 = EDGE_LOOP ( 'NONE', ( #16674, #15048, #37589, #26328 ) ) ;
#45889 = CARTESIAN_POINT ( 'NONE',  ( 1.392809637228761943, 0.03309421904702441325, -1.399748900407971064 ) ) ;
#45890 = PLANE ( 'NONE',  #44984 ) ;
#45891 = ORIENTED_EDGE ( 'NONE', *, *, #42352, .F. ) ;
#45892 = CARTESIAN_POINT ( 'NONE',  ( -1.985260859929297572, 3.267716535433071279, 0.6299212598425164567 ) ) ;
#45893 = VECTOR ( 'NONE', #35209, 39.37007874015748143 ) ;
#45894 = CARTESIAN_POINT ( 'NONE',  ( -1.636583440222564301, 3.346456692913386100, -1.325930245594398871 ) ) ;
#45895 = VECTOR ( 'NONE', #30245, 39.37007874015748143 ) ;
#45896 = PLANE ( 'NONE',  #5736 ) ;
#45897 = ORIENTED_EDGE ( 'NONE', *, *, #49008, .T. ) ;
#45898 = ORIENTED_EDGE ( 'NONE', *, *, #32828, .F. ) ;
#45899 = CARTESIAN_POINT ( 'NONE',  ( -2.182111253630085290, 3.267716535433071279, 3.785359618865288779E-16 ) ) ;
#45900 = FACE_BOUND ( 'NONE', #13548, .T. ) ;
#45901 = VERTEX_POINT ( 'NONE', #44516 ) ;
#45902 = B_SPLINE_CURVE_WITH_KNOTS ( 'NONE', 3,
 ( #45280, #37062, #29040, #9686 ),
 .UNSPECIFIED., .F., .F.,
 ( 4, 4 ),
 ( 0.0008074699510994055082, 0.001416670944113270067 ),
 .UNSPECIFIED. ) ;
#45903 = CARTESIAN_POINT ( 'NONE',  ( 0.5455278134075217666, 3.346456692913386100, 1.259842519685033357 ) ) ;
#45904 = PLANE ( 'NONE',  #50561 ) ;
#45905 = EDGE_CURVE ( 'NONE', #33786, #12621, #49524, .T. ) ;
#45906 = VERTEX_POINT ( 'NONE', #8394 ) ;
#45907 = ORIENTED_EDGE ( 'NONE', *, *, #25427, .F. ) ;
#45908 = CARTESIAN_POINT ( 'NONE',  ( 0.000000000000000000, 3.267716535433071279, 0.000000000000000000 ) ) ;
#45909 = DIRECTION ( 'NONE',  ( -0.000000000000000000, 1.000000000000000000, -0.000000000000000000 ) ) ;
#45910 = EDGE_LOOP ( 'NONE', ( #3006, #30974, #39846, #49308 ) ) ;
#45911 = ORIENTED_EDGE ( 'NONE', *, *, #26504, .F. ) ;
#45912 = EDGE_CURVE ( 'NONE', #33009, #12066, #16912, .T. ) ;
#45913 = VERTEX_POINT ( 'NONE', #44003 ) ;
#45914 = PLANE ( 'NONE',  #50708 ) ;
#45915 = DIRECTION ( 'NONE',  ( 0.000000000000000000, -1.000000000000000000, 0.000000000000000000 ) ) ;
#45916 = AXIS2_PLACEMENT_3D ( 'NONE', #15067, #50624, #29803 ) ;
#45917 = EDGE_CURVE ( 'NONE', #48631, #29859, #6317, .T. ) ;
#45918 = VECTOR ( 'NONE', #12492, 39.37007874015748143 ) ;
#45919 = CARTESIAN_POINT ( 'NONE',  ( -1.183645401082143778, 0.000000000000000000, 1.279993023352344439 ) ) ;
#45920 = ORIENTED_EDGE ( 'NONE', *, *, #20661, .T. ) ;
#45921 = ORIENTED_EDGE ( 'NONE', *, *, #26162, .T. ) ;
#45923 = CONICAL_SURFACE ( 'NONE', #49190, 3.483074324928249421, 1.244861948955335196 ) ;
#45922 = CARTESIAN_POINT ( 'NONE',  ( 2.088192093915797631, 3.267716535433071279, 0.2755905511810994302 ) ) ;
#45924 = CARTESIAN_POINT ( 'NONE',  ( -1.439733046521776139, 0.000000000000000000, 0.6299212598425164567 ) ) ;
#45925 = CARTESIAN_POINT ( 'NONE',  ( 1.052867436300554349, 1.491216683892185646, 2.758714587863916989 ) ) ;
#45926 = ADVANCED_FACE ( 'NONE', ( #20524 ), #45417, .F. ) ;
#45927 = DIRECTION ( 'NONE',  ( 0.01601477604151182663, -0.9998717552508123996, 0.000000000000000000 ) ) ;
#45928 = EDGE_CURVE ( 'NONE', #28890, #44964, #47047, .T. ) ;
#45929 = DIRECTION ( 'NONE',  ( 0.2225209339563041788, -1.131720761168132053E-16, 0.9749279121818259508 ) ) ;
#45930 = DIRECTION ( 'NONE',  ( 1.000000000000000000, 0.000000000000000000, 0.000000000000000000 ) ) ;
#45931 = DIRECTION ( 'NONE',  ( -0.000000000000000000, 0.000000000000000000, 1.000000000000000000 ) ) ;
#45932 = EDGE_LOOP ( 'NONE', ( #18507, #9191, #4733, #42553 ) ) ;
#45933 = DIRECTION ( 'NONE',  ( -1.000000000000000000, 0.000000000000000000, 0.000000000000000000 ) ) ;
#45934 = DIRECTION ( 'NONE',  ( -0.000000000000000000, 1.000000000000000000, -0.000000000000000000 ) ) ;
#45935 = AXIS2_PLACEMENT_3D ( 'NONE', #18592, #13954, #34086 ) ;
#45936 = VERTEX_POINT ( 'NONE', #28256 ) ;
#45938 = EDGE_CURVE ( 'NONE', #14593, #48594, #16141, .T. ) ;
#45937 = ORIENTED_EDGE ( 'NONE', *, *, #18580, .F. ) ;
#45939 = FACE_OUTER_BOUND ( 'NONE', #14573, .T. ) ;
#45940 = ORIENTED_EDGE ( 'NONE', *, *, #9235, .T. ) ;
#45941 = EDGE_CURVE ( 'NONE', #43368, #12647, #1413, .T. ) ;
#45942 = ORIENTED_EDGE ( 'NONE', *, *, #14795, .T. ) ;
#45943 = LINE ( 'NONE', #18860, #3159 ) ;
#45944 = ORIENTED_EDGE ( 'NONE', *, *, #17880, .T. ) ;
#45945 = FACE_OUTER_BOUND ( 'NONE', #48245, .T. ) ;
#45946 = DIRECTION ( 'NONE',  ( 0.000000000000000000, -1.000000000000000000, 0.000000000000000000 ) ) ;
#45947 = VECTOR ( 'NONE', #38548, 39.37007874015748143 ) ;
#45948 = AXIS2_PLACEMENT_3D ( 'NONE', #6727, #34359, #49791 ) ;
#45949 = ORIENTED_EDGE ( 'NONE', *, *, #16892, .T. ) ;
#45950 = ORIENTED_EDGE ( 'NONE', *, *, #34008, .T. ) ;
#45951 = CARTESIAN_POINT ( 'NONE',  ( -1.645058990017820300, 1.685622884702261626, 1.808123370684439513 ) ) ;
#45952 = ORIENTED_EDGE ( 'NONE', *, *, #15737, .T. ) ;
#45953 = ORIENTED_EDGE ( 'NONE', *, *, #10212, .F. ) ;
#45954 = CARTESIAN_POINT ( 'NONE',  ( -1.909347346926324906, 0.000000000000000000, -0.9842519685039344823 ) ) ;
#45955 = CARTESIAN_POINT ( 'NONE',  ( -2.014664160120487768, 1.577208220393157223, -0.8075893616760145832 ) ) ;
#45956 = CARTESIAN_POINT ( 'NONE',  ( 0.1155636338427008941, -0.5222242541845523167, 0.000000000000000000 ) ) ;
#45957 = CARTESIAN_POINT ( 'NONE',  ( 0.7759887336347247588, 0.04034854520891290042, -1.724780676950718794 ) ) ;
#45958 = AXIS2_PLACEMENT_3D ( 'NONE', #35636, #12140, #32282 ) ;
#45959 = ORIENTED_EDGE ( 'NONE', *, *, #33568, .F. ) ;
#45960 = DIRECTION ( 'NONE',  ( 1.000000000000000000, -0.000000000000000000, 0.000000000000000000 ) ) ;
#45961 = LINE ( 'NONE', #22250, #25017 ) ;
#45962 = CARTESIAN_POINT ( 'NONE',  ( -2.009899395340762229, 3.346456692913386100, -0.6299212598425177889 ) ) ;
#45963 = ADVANCED_FACE ( 'NONE', ( #12267 ), #36279, .F. ) ;
#45964 = ORIENTED_EDGE ( 'NONE', *, *, #21532, .F. ) ;
#45965 = AXIS2_PLACEMENT_3D ( 'NONE', #11580, #30703, #27313 ) ;
#45966 = PLANE ( 'NONE',  #49583 ) ;
#45967 = DIRECTION ( 'NONE',  ( 1.000000000000000000, 0.000000000000000000, 0.000000000000000000 ) ) ;
#45968 = VERTEX_POINT ( 'NONE', #40414 ) ;
#45969 = VERTEX_POINT ( 'NONE', #902 ) ;
#45970 = DIRECTION ( 'NONE',  ( 0.5674180297967007514, 0.5220194441718348788, -0.6368143209509024016 ) ) ;
#45971 = VECTOR ( 'NONE', #23334, 39.37007874015748143 ) ;
#45972 = B_SPLINE_CURVE_WITH_KNOTS ( 'NONE', 3,
 ( #50804, #11619, #43101, #7747 ),
 .UNSPECIFIED., .F., .F.,
 ( 4, 4 ),
 ( 3.392876324466583160E-07, 0.04779162299089171478 ),
 .UNSPECIFIED. ) ;
#45973 = CARTESIAN_POINT ( 'NONE',  ( 0.002207914879453961969, 6.692913385826772199, -2.115467123904953617 ) ) ;
#45974 = EDGE_CURVE ( 'NONE', #24477, #20150, #8902, .T. ) ;
#45975 = B_SPLINE_CURVE_WITH_KNOTS ( 'NONE', 3,
 ( #17372, #1870, #13755, #29499 ),
 .UNSPECIFIED., .F., .F.,
 ( 4, 4 ),
 ( 2.396528101364543949E-07, 0.002500331867144249369 ),
 .UNSPECIFIED. ) ;
#45976 = EDGE_CURVE ( 'NONE', #1768, #42497, #647, .T. ) ;
#45977 = LINE ( 'NONE', #10641, #31927 ) ;
#45978 = DIRECTION ( 'NONE',  ( -1.000000000000000000, 0.000000000000000000, 1.734723475976806848E-16 ) ) ;
#45979 = VERTEX_POINT ( 'NONE', #17165 ) ;
#45981 = EDGE_CURVE ( 'NONE', #28082, #24863, #27294, .T. ) ;
#45980 = ORIENTED_EDGE ( 'NONE', *, *, #42091, .F. ) ;
#45982 = CARTESIAN_POINT ( 'NONE',  ( 2.307697345854446969, 1.649818209929699186, -1.039876607722350910 ) ) ;
#45983 = ORIENTED_EDGE ( 'NONE', *, *, #48328, .T. ) ;
#45984 = FACE_OUTER_BOUND ( 'NONE', #41339, .T. ) ;
#45985 = CARTESIAN_POINT ( 'NONE',  ( 0.000000000000000000, 3.267716535433071279, -1.732283464566922726 ) ) ;
#45986 = AXIS2_PLACEMENT_3D ( 'NONE', #38925, #30931, #22174 ) ;
#45987 = VECTOR ( 'NONE', #5393, 39.37007874015748143 ) ;
#45988 = DIRECTION ( 'NONE',  ( -3.469446951953613696E-16, 0.000000000000000000, -1.000000000000000000 ) ) ;
#45989 = DIRECTION ( 'NONE',  ( -0.000000000000000000, 1.000000000000000000, -0.000000000000000000 ) ) ;
#45990 = CARTESIAN_POINT ( 'NONE',  ( 1.287906020515830141, 0.000000000000000000, -8.878505979408855953E-16 ) ) ;
#45991 = ORIENTED_EDGE ( 'NONE', *, *, #28226, .T. ) ;
#45992 = DIRECTION ( 'NONE',  ( 0.000000000000000000, 0.7071067811865466846, 0.7071067811865483499 ) ) ;
#45993 = DIRECTION ( 'NONE',  ( 0.000000000000000000, 0.000000000000000000, 1.000000000000000000 ) ) ;
#45994 = AXIS2_PLACEMENT_3D ( 'NONE', #16864, #24857, #32356 ) ;
#45995 = B_SPLINE_CURVE_WITH_KNOTS ( 'NONE', 3,
 ( #6408, #42025, #14147, #3037 ),
 .UNSPECIFIED., .F., .F.,
 ( 4, 4 ),
 ( 0.0004731792943978242651, 0.002973409787418910231 ),
 .UNSPECIFIED. ) ;
#45996 = EDGE_CURVE ( 'NONE', #5201, #37057, #47846, .T. ) ;
#45997 = LINE ( 'NONE', #22280, #41381 ) ;
#45998 = VERTEX_POINT ( 'NONE', #32412 ) ;
#46000 = LINE ( 'NONE', #41901, #42993 ) ;
#45999 = AXIS2_PLACEMENT_3D ( 'NONE', #32324, #31814, #3928 ) ;
#46001 = EDGE_CURVE ( 'NONE', #36538, #29354, #28514, .T. ) ;
#46002 = CARTESIAN_POINT ( 'NONE',  ( -0.5443978225238782498, 1.600757226547528500, -2.157565353623420723 ) ) ;
#46003 = PLANE ( 'NONE',  #40370 ) ;
#46004 = EDGE_LOOP ( 'NONE', ( #41, #4779, #8128, #47831, #19287, #29492, #31460, #39066, #21900, #22030, #23145, #11227, #3475 ) ) ;
#46005 = EDGE_CURVE ( 'NONE', #1681, #5831, #20776, .T. ) ;
#46006 = VECTOR ( 'NONE', #15648, 39.37007874015748143 ) ;
#46007 = PLANE ( 'NONE',  #23425 ) ;
#46008 = EDGE_CURVE ( 'NONE', #38012, #7287, #5541, .T. ) ;
#46009 = ADVANCED_FACE ( 'NONE', ( #46705 ), #44609, .T. ) ;
#46010 = ORIENTED_EDGE ( 'NONE', *, *, #14022, .F. ) ;
#46011 = LINE ( 'NONE', #2920, #10582 ) ;
#46012 = ORIENTED_EDGE ( 'NONE', *, *, #792, .T. ) ;
#46013 = VECTOR ( 'NONE', #48958, 39.37007874015748143 ) ;
#46014 = CARTESIAN_POINT ( 'NONE',  ( 1.091055626815042867, 3.267716535433071279, -1.892679809432644882E-16 ) ) ;
#46015 = CARTESIAN_POINT ( 'NONE',  ( 0.000000000000000000, 0.4724409448818898127, -1.014069264286642236 ) ) ;
#46016 = DIRECTION ( 'NONE',  ( -0.5128992774058948045, 9.966352232896248990E-17, -0.8584487936018727616 ) ) ;
#46017 = DIRECTION ( 'NONE',  ( 0.000000000000000000, 0.000000000000000000, -1.000000000000000000 ) ) ;
#46018 = ORIENTED_EDGE ( 'NONE', *, *, #24335, .T. ) ;
#46019 = ORIENTED_EDGE ( 'NONE', *, *, #10668, .F. ) ;
#46020 = PLANE ( 'NONE',  #29853 ) ;
#46021 = CARTESIAN_POINT ( 'NONE',  ( -0.4832241344345758471, 3.255108573300695252, -2.401574803149598036 ) ) ;
#46022 = VERTEX_POINT ( 'NONE', #30999 ) ;
#46023 = CARTESIAN_POINT ( 'NONE',  ( -1.002259110181423551, 1.593423740086483020, -1.967789019142131002 ) ) ;
#46024 = CARTESIAN_POINT ( 'NONE',  ( 2.559055118110237004, 0.000000000000000000, 2.165354330708661568 ) ) ;
#46025 = LINE ( 'NONE', #10685, #8806 ) ;
#46026 = ORIENTED_EDGE ( 'NONE', *, *, #20356, .F. ) ;
#46027 = ORIENTED_EDGE ( 'NONE', *, *, #8718, .F. ) ;
#46028 = CARTESIAN_POINT ( 'NONE',  ( 1.091055626815042645, 0.000000000000000000, -0.3149606299212596716 ) ) ;
#46029 = CARTESIAN_POINT ( 'NONE',  ( -1.068075307999488244, 6.692913385826772199, 1.883606783264637041 ) ) ;
#46030 = VECTOR ( 'NONE', #42479, 39.37007874015748143 ) ;
#46031 = CARTESIAN_POINT ( 'NONE',  ( 4.268512490100411402E-16, 3.346456692913386100, 1.259842519685033357 ) ) ;
#46032 = VERTEX_POINT ( 'NONE', #29985 ) ;
#46033 = DIRECTION ( 'NONE',  ( -0.000000000000000000, 1.000000000000000000, -0.000000000000000000 ) ) ;
#46034 = DIRECTION ( 'NONE',  ( 1.953992523340275196E-14, 0.000000000000000000, 1.000000000000000000 ) ) ;
#46035 = ORIENTED_EDGE ( 'NONE', *, *, #50619, .T. ) ;
#46036 = LINE ( 'NONE', #10699, #47973 ) ;
#46037 = ORIENTED_EDGE ( 'NONE', *, *, #40079, .T. ) ;
#46039 = EDGE_LOOP ( 'NONE', ( #17630, #36943, #19559, #11690 ) ) ;
#46038 = VECTOR ( 'NONE', #20110, 39.37007874015748143 ) ;
#46040 = DIRECTION ( 'NONE',  ( -0.01601477604151182663, 0.9998717552508123996, -0.000000000000000000 ) ) ;
#46041 = CARTESIAN_POINT ( 'NONE',  ( 2.042485253772177156, 1.205361022782829114E-17, 0.6118985000151695441 ) ) ;
#46042 = VECTOR ( 'NONE', #2044, 39.37007874015748143 ) ;
#46043 = CARTESIAN_POINT ( 'NONE',  ( 1.015142113812069313, 3.346456692913386100, 0.1574803149606286423 ) ) ;
#46044 = CARTESIAN_POINT ( 'NONE',  ( -2.454875160333845674, 3.242921367653845977, -0.03937007874015881204 ) ) ;
#46046 = DIRECTION ( 'NONE',  ( -0.000000000000000000, 1.000000000000000000, -0.000000000000000000 ) ) ;
#46045=STYLED_ITEM('',(#51101),#41044);
#46047 = B_SPLINE_CURVE_WITH_KNOTS ( 'NONE', 3,
 ( #36006, #17908, #18161, #5778 ),
 .UNSPECIFIED., .F., .F.,
 ( 4, 4 ),
 ( 7.003658972180221081E-07, 0.002501219077655048462 ),
 .UNSPECIFIED. ) ;
#46048 = VERTEX_POINT ( 'NONE', #45702 ) ;
#46049 = EDGE_CURVE ( 'NONE', #36016, #10759, #9701, .T. ) ;
#46050 = EDGE_CURVE ( 'NONE', #40640, #27577, #27112, .T. ) ;
#46051 = VECTOR ( 'NONE', #50222, 39.37007874015748143 ) ;
#46052 = ORIENTED_EDGE ( 'NONE', *, *, #48882, .T. ) ;
#46053 = LINE ( 'NONE', #2965, #40951 ) ;
#46054 = EDGE_CURVE ( 'NONE', #26348, #21582, #37997, .T. ) ;
#46055 = DIRECTION ( 'NONE',  ( -0.000000000000000000, 1.000000000000000000, -0.000000000000000000 ) ) ;
#46056 = CARTESIAN_POINT ( 'NONE',  ( -1.331808205664968492, 0.000000000000000000, 1.125026879082024367 ) ) ;
#46057 = FACE_OUTER_BOUND ( 'NONE', #45350, .T. ) ;
#46058 = CARTESIAN_POINT ( 'NONE',  ( 0.7423782071083091516, 3.267716535433071279, -2.575641807848711673E-16 ) ) ;
#46059 = ORIENTED_EDGE ( 'NONE', *, *, #49327, .T. ) ;
#46060 = CARTESIAN_POINT ( 'NONE',  ( 0.4696143004045478797, 3.267716535433071279, 0.5905511811023579360 ) ) ;
#46061 = EDGE_CURVE ( 'NONE', #5100, #28890, #38502, .T. ) ;
#46062 = CARTESIAN_POINT ( 'NONE',  ( 2.024272128602276233, 1.049866565877818347, -0.04164796393617213599 ) ) ;
#46063 = EDGE_LOOP ( 'NONE', ( #38542, #25371, #9608, #10252 ) ) ;
#46064 = CARTESIAN_POINT ( 'NONE',  ( -0.5455278134075214336, 3.267716535433071279, -1.259842519685035134 ) ) ;
#46065 = ADVANCED_FACE ( 'NONE', ( #26611 ), #15000, .F. ) ;
#46066 = CARTESIAN_POINT ( 'NONE',  ( 2.325893555657776002, 1.679538594897605819, -0.05519379784448211895 ) ) ;
#46067 = ORIENTED_EDGE ( 'NONE', *, *, #15053, .T. ) ;
#46068 = CARTESIAN_POINT ( 'NONE',  ( -1.363819533518803473, 0.000000000000000000, 2.047244094488179567 ) ) ;
#46069 = VECTOR ( 'NONE', #21731, 39.37007874015748143 ) ;
#46070 = CARTESIAN_POINT ( 'NONE',  ( -0.6214413264104952095, 3.267716535433071279, 2.156057715732903491E-16 ) ) ;
#46071 = DIRECTION ( 'NONE',  ( 1.734723475976806848E-16, -0.000000000000000000, 1.000000000000000000 ) ) ;
#46072 = EDGE_CURVE ( 'NONE', #25893, #31173, #11373, .T. ) ;
#46073 = ORIENTED_EDGE ( 'NONE', *, *, #24754, .F. ) ;
#46074 = DIRECTION ( 'NONE',  ( -0.01601477604151182663, 0.9998717552508123996, -0.000000000000000000 ) ) ;
#46075 = ORIENTED_EDGE ( 'NONE', *, *, #38036, .T. ) ;
#46076 = FACE_BOUND ( 'NONE', #5300, .T. ) ;
#46077 = VECTOR ( 'NONE', #33879, 39.37007874015748143 ) ;
#46078 = VECTOR ( 'NONE', #21820, 39.37007874015748143 ) ;
#46079 = LINE ( 'NONE', #11243, #37529 ) ;
#46080 = CARTESIAN_POINT ( 'NONE',  ( -0.8942052331142547050, 0.000000000000000000, 0.9448818897637749625 ) ) ;
#46081 = AXIS2_PLACEMENT_3D ( 'NONE', #37862, #18224, #44556 ) ;
#46082 = ORIENTED_EDGE ( 'NONE', *, *, #36957, .F. ) ;
#46083 = ORIENTED_EDGE ( 'NONE', *, *, #30089, .T. ) ;
#46084 = PLANE ( 'NONE',  #26523 ) ;
#46085 = LINE ( 'NONE', #29856, #20514 ) ;
#46086 = PLANE ( 'NONE',  #49923 ) ;
#46087 = AXIS2_PLACEMENT_3D ( 'NONE', #50659, #3991, #19721 ) ;
#46088 = CARTESIAN_POINT ( 'NONE',  ( -2.919426793319806368, 5.905511811023623991, 0.4451252810446391095 ) ) ;
#46089 = CARTESIAN_POINT ( 'NONE',  ( 0.08139965876239094178, 1.610780518492231694, 0.000000000000000000 ) ) ;
#46090 = EDGE_LOOP ( 'NONE', ( #29778, #45011, #19495, #20070 ) ) ;
#46091 = EDGE_LOOP ( 'NONE', ( #40895, #13858, #18836, #12984 ) ) ;
#46092 = LINE ( 'NONE', #10747, #1021 ) ;
#46093 = CARTESIAN_POINT ( 'NONE',  ( 0.07982360342473591996, 1.709180471932028711, 0.000000000000000000 ) ) ;
#46094 = EDGE_LOOP ( 'NONE', ( #38874, #38111, #42570, #2662 ) ) ;
#46095 = DIRECTION ( 'NONE',  ( 0.7071067811865486830, 2.775557561562891351E-17, 0.7071067811865462405 ) ) ;
#46096 = EDGE_LOOP ( 'NONE', ( #32997, #24448, #36646, #7429, #37530 ) ) ;
#46097 = VERTEX_POINT ( 'NONE', #15249 ) ;
#46098 = VECTOR ( 'NONE', #36285, 39.37007874015748143 ) ;
#46099 = ORIENTED_EDGE ( 'NONE', *, *, #35919, .F. ) ;
#46100 = ORIENTED_EDGE ( 'NONE', *, *, #50646, .T. ) ;
#46101 = CARTESIAN_POINT ( 'NONE',  ( -0.8182917201112815953, 3.267716535433071279, 1.419509857074482553E-16 ) ) ;
#46102 = EDGE_CURVE ( 'NONE', #17882, #46852, #17415, .T. ) ;
#46103 = ADVANCED_FACE ( 'NONE', ( #2873 ), #18367, .F. ) ;
#46104 = DIRECTION ( 'NONE',  ( 0.000000000000000000, 0.000000000000000000, -1.000000000000000000 ) ) ;
#46105 = CARTESIAN_POINT ( 'NONE',  ( 0.4696143004045478797, 3.346456692913386100, 0.5905511811023579360 ) ) ;
#46106 = ADVANCED_FACE ( 'NONE', ( #19111 ), #34758, .T. ) ;
#46107 = VECTOR ( 'NONE', #26628, 39.37007874015748143 ) ;
#46108 = LINE ( 'NONE', #34524, #27250 ) ;
#46109 = B_SPLINE_CURVE_WITH_KNOTS ( 'NONE', 3,
 ( #9725, #13343, #17973, #29077 ),
 .UNSPECIFIED., .F., .F.,
 ( 4, 4 ),
 ( 0.05133901200620183403, 0.05249386097095985054 ),
 .UNSPECIFIED. ) ;
#46110 = DIRECTION ( 'NONE',  ( -0.000000000000000000, 1.000000000000000000, -0.000000000000000000 ) ) ;
#46111 = DIRECTION ( 'NONE',  ( -0.4738686624729965269, -1.160734090543304660E-16, -0.8805955318567391110 ) ) ;
#46112 = VERTEX_POINT ( 'NONE', #38251 ) ;
#46113 = B_SPLINE_CURVE_WITH_KNOTS ( 'NONE', 3,
 ( #33841, #37718, #14462, #10592 ),
 .UNSPECIFIED., .F., .F.,
 ( 4, 4 ),
 ( 0.001127418191887998586, 0.003627694388309332489 ),
 .UNSPECIFIED. ) ;
#46114 = DIRECTION ( 'NONE',  ( 0.000000000000000000, -1.000000000000000000, 0.000000000000000000 ) ) ;
#46115 = DIRECTION ( 'NONE',  ( 1.000000000000000000, 0.000000000000000000, 0.000000000000000000 ) ) ;
#46116 = CONICAL_SURFACE ( 'NONE', #1625, 3.483074324928249421, 1.244861948955335196 ) ;
#46117 = FACE_OUTER_BOUND ( 'NONE', #14746, .T. ) ;
#46118 = CARTESIAN_POINT ( 'NONE',  ( -1.363819533518803473, 0.000000000000000000, -1.732283464566922726 ) ) ;
#46119 = ORIENTED_EDGE ( 'NONE', *, *, #398, .F. ) ;
#46120 = LINE ( 'NONE', #50466, #13319 ) ;
#46121 = EDGE_CURVE ( 'NONE', #12444, #44668, #18626, .T. ) ;
#46122 = CARTESIAN_POINT ( 'NONE',  ( -1.363819533518803473, 3.346456692913386100, 2.047244094488179567 ) ) ;
#46123 = ORIENTED_EDGE ( 'NONE', *, *, #11295, .F. ) ;
#46124 = LINE ( 'NONE', #18783, #16372 ) ;
#46125 = CARTESIAN_POINT ( 'NONE',  ( -2.165354330708661568, 1.673228346456695492, -0.01597875172208130037 ) ) ;
#46126 = VERTEX_POINT ( 'NONE', #30496 ) ;
#46127 = B_SPLINE_CURVE_WITH_KNOTS ( 'NONE', 3,
 ( #5282, #36024, #25161, #24906 ),
 .UNSPECIFIED., .F., .F.,
 ( 4, 4 ),
 ( 0.001455260405619622196, 0.003955466538311651695 ),
 .UNSPECIFIED. ) ;
#46128 = EDGE_CURVE ( 'NONE', #38637, #41521, #46209, .T. ) ;
#46129 = CARTESIAN_POINT ( 'NONE',  ( -1.091055626815042645, 3.346456692913386100, -1.259842519685034690 ) ) ;
#46130 = VERTEX_POINT ( 'NONE', #22997 ) ;
#46131 = DIRECTION ( 'NONE',  ( -9.390536051998764103E-17, -1.000000000000000000, -6.822623802544789917E-17 ) ) ;
#46132 = DIRECTION ( 'NONE',  ( 0.000000000000000000, -1.000000000000000000, 0.000000000000000000 ) ) ;
#46133 = LINE ( 'NONE', #22916, #44343 ) ;
#46134 = PLANE ( 'NONE',  #31696 ) ;
#46135 = CARTESIAN_POINT ( 'NONE',  ( -0.5455278134075208785, 0.000000000000000000, 1.259842519685033357 ) ) ;
#46136 = VECTOR ( 'NONE', #14306, 39.37007874015748143 ) ;
#46137 = ORIENTED_EDGE ( 'NONE', *, *, #10327, .T. ) ;
#46138 = DIRECTION ( 'NONE',  ( -0.000000000000000000, 1.000000000000000000, -0.000000000000000000 ) ) ;
#46139 = VERTEX_POINT ( 'NONE', #18876 ) ;
#46140 = ORIENTED_EDGE ( 'NONE', *, *, #33889, .F. ) ;
#46141 = LINE ( 'NONE', #38681, #50924 ) ;
#46142 = ORIENTED_EDGE ( 'NONE', *, *, #14498, .F. ) ;
#46143 = DIRECTION ( 'NONE',  ( 0.000000000000000000, 0.000000000000000000, 1.000000000000000000 ) ) ;
#46144 = DIRECTION ( 'NONE',  ( 8.859168527467109606E-18, 0.6427876096865404731, -0.7660444431189771253 ) ) ;
#46145 = ADVANCED_FACE ( 'NONE', ( #30746 ), #11126, .T. ) ;
#46146 = ORIENTED_EDGE ( 'NONE', *, *, #31264, .T. ) ;
#46147 = AXIS2_PLACEMENT_3D ( 'NONE', #16744, #19825, #35592 ) ;
#46148 = DIRECTION ( 'NONE',  ( 0.5407162030609372616, -0.6444004775717706579, 0.5407162030609374836 ) ) ;
#46149 = VECTOR ( 'NONE', #3206, 39.37007874015748143 ) ;
#46150 = CARTESIAN_POINT ( 'NONE',  ( 1.971247363764867977, 1.574803149606302854, -0.8960709840011636951 ) ) ;
#46151 = FACE_OUTER_BOUND ( 'NONE', #35161, .T. ) ;
#46152 = ORIENTED_EDGE ( 'NONE', *, *, #15524, .T. ) ;
#46153 = ORIENTED_EDGE ( 'NONE', *, *, #15047, .T. ) ;
#46154 = DIRECTION ( 'NONE',  ( 0.000000000000000000, 1.160734090543304660E-16, -1.000000000000000000 ) ) ;
#46155 = FACE_BOUND ( 'NONE', #17811, .T. ) ;
#46156 = ORIENTED_EDGE ( 'NONE', *, *, #15769, .F. ) ;
#46157 = VECTOR ( 'NONE', #1334, 39.37007874015748143 ) ;
#46158 = CARTESIAN_POINT ( 'NONE',  ( 0.000000000000000000, 3.346456692913386100, 0.000000000000000000 ) ) ;
#46159 = ORIENTED_EDGE ( 'NONE', *, *, #5101, .T. ) ;
#46160 = ORIENTED_EDGE ( 'NONE', *, *, #39482, .T. ) ;
#46161 = DIRECTION ( 'NONE',  ( 1.734723475976806848E-16, 0.000000000000000000, 1.000000000000000000 ) ) ;
#46162 = CARTESIAN_POINT ( 'NONE',  ( 0.7423782071083085965, 0.000000000000000000, 0.1181102362204701633 ) ) ;
#46163 = ORIENTED_EDGE ( 'NONE', *, *, #41851, .F. ) ;
#46164 = VERTEX_POINT ( 'NONE', #3371 ) ;
#46165 = CARTESIAN_POINT ( 'NONE',  ( -1.979793062125317471, 0.000000000000000000, 2.191257344206539504 ) ) ;
#46166 = ADVANCED_FACE ( 'NONE', ( #50551 ), #11873, .F. ) ;
#46167 = CARTESIAN_POINT ( 'NONE',  ( -1.909347346926324462, 0.000000000000000000, 0.7874015748031456541 ) ) ;
#46168 = EDGE_CURVE ( 'NONE', #24319, #45969, #19359, .T. ) ;
#46169 = EDGE_CURVE ( 'NONE', #44079, #45841, #24004, .T. ) ;
#46170 = CARTESIAN_POINT ( 'NONE',  ( 1.363819533518803251, 0.000000000000000000, -0.6692913385826764205 ) ) ;
#46171 = ORIENTED_EDGE ( 'NONE', *, *, #25927, .T. ) ;
#46172 = EDGE_LOOP ( 'NONE', ( #20701, #33564, #17270, #31859 ) ) ;
#46173 = DIRECTION ( 'NONE',  ( -0.000000000000000000, 0.000000000000000000, 1.000000000000000000 ) ) ;
#46174 = CARTESIAN_POINT ( 'NONE',  ( -0.8942052331142547050, 3.346456692913386100, 0.7480314960629874665 ) ) ;
#46175 = DIRECTION ( 'NONE',  ( 1.000000000000000000, 0.000000000000000000, -3.469446951953613696E-16 ) ) ;
#46176 = LINE ( 'NONE', #18842, #14444 ) ;
#46177 = DIRECTION ( 'NONE',  ( -1.000000000000000000, 0.000000000000000000, -0.000000000000000000 ) ) ;
#46178 = VECTOR ( 'NONE', #44789, 39.37007874015748143 ) ;
#46179 = VECTOR ( 'NONE', #48288, 39.37007874015748143 ) ;
#46180 = CARTESIAN_POINT ( 'NONE',  ( 0.9035029780573708980, 0.01393497246690909679, -1.762719797743741657 ) ) ;
#46181 = EDGE_CURVE ( 'NONE', #28099, #13566, #16006, .T. ) ;
#46182 = CARTESIAN_POINT ( 'NONE',  ( 0.5272349255864847706, 5.905511811023623991, 2.905303903342417726 ) ) ;
#46183 = ORIENTED_EDGE ( 'NONE', *, *, #43374, .F. ) ;
#46184 = CARTESIAN_POINT ( 'NONE',  ( -1.645894780863147000, 0.6447981115998608903, -1.427454079380623408 ) ) ;
#46185 = CARTESIAN_POINT ( 'NONE',  ( -1.439733046521776583, 0.000000000000000000, -0.9448818897637762948 ) ) ;
#46186 = ADVANCED_FACE ( 'NONE', ( #517 ), #35888, .F. ) ;
#46187 = VECTOR ( 'NONE', #510, 39.37007874015748143 ) ;
#46188 = ORIENTED_EDGE ( 'NONE', *, *, #18107, .T. ) ;
#46189 = ORIENTED_EDGE ( 'NONE', *, *, #27004, .T. ) ;
#46190 = FACE_OUTER_BOUND ( 'NONE', #12249, .T. ) ;
#46191 = CARTESIAN_POINT ( 'NONE',  ( -1.909347346926324462, 3.346456692913386100, 0.2755905511810996522 ) ) ;
#46192 = EDGE_LOOP ( 'NONE', ( #3251, #18677, #27303, #14197 ) ) ;
#46193 = EDGE_CURVE ( 'NONE', #10470, #38339, #49961, .T. ) ;
#46194 = VERTEX_POINT ( 'NONE', #31503 ) ;
#46195 = DIRECTION ( 'NONE',  ( -1.000000000000000000, 0.000000000000000000, 0.000000000000000000 ) ) ;
#46196 = EDGE_CURVE ( 'NONE', #19475, #21072, #27614, .T. ) ;
#46197 = VERTEX_POINT ( 'NONE', #39503 ) ;
#46198 = DIRECTION ( 'NONE',  ( 0.000000000000000000, 1.000000000000000000, 0.000000000000000000 ) ) ;
#46199 = FACE_OUTER_BOUND ( 'NONE', #10455, .T. ) ;
#46200 = B_SPLINE_CURVE_WITH_KNOTS ( 'NONE', 3,
 ( #17393, #25646, #20753, #36513 ),
 .UNSPECIFIED., .F., .F.,
 ( 4, 4 ),
 ( 4.095189062770323219E-07, 0.04904918211385326382 ),
 .UNSPECIFIED. ) ;
#46201 = VERTEX_POINT ( 'NONE', #8263 ) ;
#46202 = CARTESIAN_POINT ( 'NONE',  ( 2.064489077472676737, 1.642543324816299277, 1.055063358597729595 ) ) ;
#46203 = B_SPLINE_CURVE_WITH_KNOTS ( 'NONE', 3,
 ( #18203, #14328, #49400, #33203 ),
 .UNSPECIFIED., .F., .F.,
 ( 4, 4 ),
 ( 0.01096540280937795438, 0.03073589712859321754 ),
 .UNSPECIFIED. ) ;
#46204 = EDGE_LOOP ( 'NONE', ( #50509, #11135, #35560, #14974 ) ) ;
#46205 = ORIENTED_EDGE ( 'NONE', *, *, #1727, .T. ) ;
#46206 = EDGE_CURVE ( 'NONE', #17928, #10946, #43362, .T. ) ;
#46207 = CARTESIAN_POINT ( 'NONE',  ( -1.569555324610094393, 0.001878576622170695463, 0.7887281490750877033 ) ) ;
#46208 = CARTESIAN_POINT ( 'NONE',  ( 1.091055626815043311, 3.346456692913386100, 1.801691980386208591 ) ) ;
#46209 = LINE ( 'NONE', #6999, #18247 ) ;
#46210 = CARTESIAN_POINT ( 'NONE',  ( 0.2727639067037604947, 3.346456692913386100, -1.417322834645664331 ) ) ;
#46211 = EDGE_CURVE ( 'NONE', #15045, #12815, #31256, .T. ) ;
#46212 = VECTOR ( 'NONE', #4112, 39.37007874015748143 ) ;
#46213 = ORIENTED_EDGE ( 'NONE', *, *, #5639, .F. ) ;
#46214 = CIRCLE ( 'NONE', #6668, 2.164630168518208109 ) ;
#46215 = CARTESIAN_POINT ( 'NONE',  ( 0.4349608091550764555, 1.574803149606302854, 2.121218629000301004 ) ) ;
#46216 = CARTESIAN_POINT ( 'NONE',  ( -0.8182917201112819283, 0.000000000000000000, -0.7874015748031467643 ) ) ;
#46217 = LINE ( 'NONE', #37499, #6373 ) ;
#46218 = ORIENTED_EDGE ( 'NONE', *, *, #50051, .F. ) ;
#46219 = CARTESIAN_POINT ( 'NONE',  ( 0.000000000000000000, 3.346456692913386100, 0.000000000000000000 ) ) ;
#46220 = ORIENTED_EDGE ( 'NONE', *, *, #48688, .F. ) ;
#46221 = ORIENTED_EDGE ( 'NONE', *, *, #2556, .F. ) ;
#46222 = CIRCLE ( 'NONE', #28926, 2.086614173228346303 ) ;
#46223 = CARTESIAN_POINT ( 'NONE',  ( -3.927031490892378253E-16, 3.346456692913386100, -1.889763779527552146 ) ) ;
#46224 = EDGE_CURVE ( 'NONE', #49325, #35993, #32023, .T. ) ;
#46225 = CARTESIAN_POINT ( 'NONE',  ( -0.8182917201112819283, 3.346456692913386100, -1.417322834645664331 ) ) ;
#46226 = CARTESIAN_POINT ( 'NONE',  ( 0.1155636338427008941, -0.5222242541845523167, 0.000000000000000000 ) ) ;
#46227 = ADVANCED_FACE ( 'NONE', ( #40015 ), #4138, .T. ) ;
#46228 = EDGE_CURVE ( 'NONE', #45803, #50682, #47461, .T. ) ;
#46229 = DIRECTION ( 'NONE',  ( -0.3930250316539147803, 1.288287287306305283E-16, -0.9195277725514544587 ) ) ;
#46230 = ORIENTED_EDGE ( 'NONE', *, *, #684, .F. ) ;
#46231 = ORIENTED_EDGE ( 'NONE', *, *, #8959, .T. ) ;
#46232 = CARTESIAN_POINT ( 'NONE',  ( 4.580371886574746102E-17, 7.874015748031496287, 0.3740157480314960647 ) ) ;
#46233 = CARTESIAN_POINT ( 'NONE',  ( -0.5455278134075209895, 3.267716535433071279, 9.463399047163218249E-17 ) ) ;
#46234 = ORIENTED_EDGE ( 'NONE', *, *, #48817, .F. ) ;
#46235 = CARTESIAN_POINT ( 'NONE',  ( -1.062992125984252079, 0.000000000000000000, -1.181102362204724754 ) ) ;
#46236 = DIRECTION ( 'NONE',  ( 1.000000000000000000, 0.000000000000000000, 0.000000000000000000 ) ) ;
#46237 = CARTESIAN_POINT ( 'NONE',  ( 0.2899689346265602041, 0.02164905224627299354, 1.873473513055692763 ) ) ;
#46238 = DIRECTION ( 'NONE',  ( -0.000000000000000000, -1.000000000000000000, -0.000000000000000000 ) ) ;
#46239 = LINE ( 'NONE', #50833, #7269 ) ;
#46240 = VERTEX_POINT ( 'NONE', #12649 ) ;
#46241 = CARTESIAN_POINT ( 'NONE',  ( 2.323794147221719175, 1.745121766917047790, -0.05509951330290247667 ) ) ;
#46242 = CARTESIAN_POINT ( 'NONE',  ( -1.334208625815133553, 3.267716535433071279, 2.047244094488179567 ) ) ;
#46243 = AXIS2_PLACEMENT_3D ( 'NONE', #43567, #20597, #19817 ) ;
#46244 = FACE_OUTER_BOUND ( 'NONE', #18153, .T. ) ;
#46245 = VECTOR ( 'NONE', #8173, 39.37007874015748143 ) ;
#46246 = ORIENTED_EDGE ( 'NONE', *, *, #25775, .F. ) ;
#46247 = PLANE ( 'NONE',  #19913 ) ;
#46248 = AXIS2_PLACEMENT_3D ( 'NONE', #25348, #41607, #37745 ) ;
#46249 = CARTESIAN_POINT ( 'NONE',  ( -1.712496953225537188, 3.346456692913386100, 1.102362204724404160 ) ) ;
#46250 = LINE ( 'NONE', #11166, #27114 ) ;
#46251 = VERTEX_POINT ( 'NONE', #251 ) ;
#46252 = EDGE_CURVE ( 'NONE', #37178, #38637, #12136, .T. ) ;
#46253 = CARTESIAN_POINT ( 'NONE',  ( 0.2510238314733705400, 1.613497360050089036, -2.240096307734528835 ) ) ;
#46254 = VECTOR ( 'NONE', #2381, 39.37007874015748143 ) ;
#46255 = ORIENTED_EDGE ( 'NONE', *, *, #10751, .F. ) ;
#46256 = DIRECTION ( 'NONE',  ( 0.000000000000000000, 0.000000000000000000, -1.000000000000000000 ) ) ;
#46257 = VECTOR ( 'NONE', #40276, 39.37007874015748143 ) ;
#46258 = ORIENTED_EDGE ( 'NONE', *, *, #2825, .T. ) ;
#46259 = CARTESIAN_POINT ( 'NONE',  ( 1.833433833923351353, 3.346456692913386100, 0.3149606299212576177 ) ) ;
#46260 = EDGE_CURVE ( 'NONE', #2462, #34201, #20120, .T. ) ;
#46261 = VECTOR ( 'NONE', #1195, 39.37007874015748143 ) ;
#46262 = FACE_OUTER_BOUND ( 'NONE', #24887, .T. ) ;
#46263 = CARTESIAN_POINT ( 'NONE',  ( 1.325491792074624087, 1.739919523179865202, -2.638988599164732385 ) ) ;
#46264 = DIRECTION ( 'NONE',  ( 0.000000000000000000, 0.000000000000000000, -1.000000000000000000 ) ) ;
#46265 = EDGE_CURVE ( 'NONE', #37644, #3939, #12389, .T. ) ;
#46266 = EDGE_CURVE ( 'NONE', #32732, #20175, #43869, .T. ) ;
#46267 = ORIENTED_EDGE ( 'NONE', *, *, #255, .T. ) ;
#46268 = VERTEX_POINT ( 'NONE', #38991 ) ;
#46269 = ORIENTED_EDGE ( 'NONE', *, *, #15896, .F. ) ;
#46270 = LINE ( 'NONE', #23055, #20785 ) ;
#46271 = CARTESIAN_POINT ( 'NONE',  ( -6.488138984952638702E-17, 3.267716535433071279, 1.125512701259767226E-32 ) ) ;
#46272 = ORIENTED_EDGE ( 'NONE', *, *, #8449, .F. ) ;
#46273 = DIRECTION ( 'NONE',  ( 1.734723475976806848E-16, 0.000000000000000000, 1.000000000000000000 ) ) ;
#46274 = CARTESIAN_POINT ( 'NONE',  ( 0.4696143004045476577, 3.346456692913386100, -1.732283464566922726 ) ) ;
#46275 = CARTESIAN_POINT ( 'NONE',  ( 2.188498384461881940, 0.5221067302336409588, 0.6593410420848859754 ) ) ;
#46276 = ORIENTED_EDGE ( 'NONE', *, *, #30990, .T. ) ;
#46277 = ORIENTED_EDGE ( 'NONE', *, *, #26058, .T. ) ;
#46278 = CARTESIAN_POINT ( 'NONE',  ( 1.833433833923351353, 0.000000000000000000, -1.161035397307311917E-15 ) ) ;
#46279 = DIRECTION ( 'NONE',  ( 1.734723475976806848E-16, 0.000000000000000000, 1.000000000000000000 ) ) ;
#46280 = CARTESIAN_POINT ( 'NONE',  ( -0.2727639067037602727, 3.346456692913386100, 1.850393700787392293 ) ) ;
#46281 = EDGE_LOOP ( 'NONE', ( #4618, #26448, #7311, #19873 ) ) ;
#46282 = CARTESIAN_POINT ( 'NONE',  ( 0.7423782071083092626, 0.000000000000000000, 1.889763779527550369 ) ) ;
#46283 = FACE_BOUND ( 'NONE', #35181, .T. ) ;
#46284 = ORIENTED_EDGE ( 'NONE', *, *, #40679, .T. ) ;
#46285 = CARTESIAN_POINT ( 'NONE',  ( 0.000000000000000000, 3.267716535433071279, 0.5905511811023582691 ) ) ;
#46286 = ORIENTED_EDGE ( 'NONE', *, *, #49037, .F. ) ;
#46287 = ORIENTED_EDGE ( 'NONE', *, *, #28992, .T. ) ;
#46288 = CARTESIAN_POINT ( 'NONE',  ( -0.8182917201112819283, 3.267716535433071279, -0.03937007874015895081 ) ) ;
#46289 = CARTESIAN_POINT ( 'NONE',  ( 0.9838852166858921278, 0.000000000000000000, 1.929635236160317735 ) ) ;
#46290 = VECTOR ( 'NONE', #10468, 39.37007874015748143 ) ;
#46291 = EDGE_CURVE ( 'NONE', #30940, #31066, #3627, .T. ) ;
#46293 = VECTOR ( 'NONE', #21810, 39.37007874015748143 ) ;
#46292 = DIRECTION ( 'NONE',  ( 1.000000000000000000, 0.000000000000000000, 0.000000000000000000 ) ) ;
#46294 = DIRECTION ( 'NONE',  ( -1.000000000000000000, 0.000000000000000000, 0.000000000000000000 ) ) ;
#46295 = EDGE_CURVE ( 'NONE', #129, #19452, #11620, .T. ) ;
#46296 = EDGE_CURVE ( 'NONE', #42335, #48626, #48711, .T. ) ;
#46297 = CARTESIAN_POINT ( 'NONE',  ( 1.560669927219590525, 0.000000000000000000, 1.220472440944875281 ) ) ;
#46298 = ORIENTED_EDGE ( 'NONE', *, *, #9890, .T. ) ;
#46299 = AXIS2_PLACEMENT_3D ( 'NONE', #49370, #10167, #22048 ) ;
#46300 = EDGE_CURVE ( 'NONE', #17210, #39291, #29419, .T. ) ;
#46301 = VECTOR ( 'NONE', #9744, 39.37007874015748854 ) ;
#46302 = ORIENTED_EDGE ( 'NONE', *, *, #11042, .F. ) ;
#46303 = DIRECTION ( 'NONE',  ( 1.000000000000000000, -0.000000000000000000, -0.000000000000000000 ) ) ;
#46304 = LINE ( 'NONE', #26700, #6153 ) ;
#46305 = AXIS2_PLACEMENT_3D ( 'NONE', #47309, #39858, #27719 ) ;
#46306 = CARTESIAN_POINT ( 'NONE',  ( 1.363819533518803251, 0.000000000000000000, 0.9055118110236164419 ) ) ;
#46307 = FACE_OUTER_BOUND ( 'NONE', #4355, .T. ) ;
#46308 = CARTESIAN_POINT ( 'NONE',  ( 2.182111253630085290, 0.000000000000000000, -0.1968503937007886062 ) ) ;
#46309 = VERTEX_POINT ( 'NONE', #36401 ) ;
#46310 = CARTESIAN_POINT ( 'NONE',  ( -2.160407304981126320, 1.673304745347873324, -0.1462862061266896330 ) ) ;
#46311 = CARTESIAN_POINT ( 'NONE',  ( 0.000000000000000000, 0.5905511811023621549, 1.062992125984251413 ) ) ;
#46312 = ORIENTED_EDGE ( 'NONE', *, *, #18461, .T. ) ;
#46313 = LINE ( 'NONE', #30599, #48716 ) ;
#46314 = CARTESIAN_POINT ( 'NONE',  ( -1.363819533518803029, 3.346456692913386100, -0.03937007874015868020 ) ) ;
#46315 = DIRECTION ( 'NONE',  ( -0.000000000000000000, 0.000000000000000000, 1.000000000000000000 ) ) ;
#46316 = DIRECTION ( 'NONE',  ( 1.000000000000000000, -0.000000000000000000, 0.000000000000000000 ) ) ;
#46317 = CARTESIAN_POINT ( 'NONE',  ( 0.4349608091550758449, 6.692913385826772199, 2.121218629000301004 ) ) ;
#46318 = DIRECTION ( 'NONE',  ( 1.734723475976806848E-16, -0.000000000000000000, 1.000000000000000000 ) ) ;
#46319 = ORIENTED_EDGE ( 'NONE', *, *, #24426, .F. ) ;
#46320 = DIRECTION ( 'NONE',  ( -1.000000000000000000, 0.000000000000000000, 0.000000000000000000 ) ) ;
#46321 = ORIENTED_EDGE ( 'NONE', *, *, #5890, .F. ) ;
#46322 = FACE_BOUND ( 'NONE', #40395, .T. ) ;
#46323 = VECTOR ( 'NONE', #5988, 39.37007874015748143 ) ;
#46324 = CARTESIAN_POINT ( 'NONE',  ( -1.420868632364155282, 0.000000000000000000, 1.070159647439151707 ) ) ;
#46325 = DIRECTION ( 'NONE',  ( -1.000000000000000000, -0.000000000000000000, -0.000000000000000000 ) ) ;
#46326 = EDGE_CURVE ( 'NONE', #10170, #43507, #37176, .T. ) ;
#46327 = EDGE_CURVE ( 'NONE', #24863, #3256, #17045, .T. ) ;
#46328 = VECTOR ( 'NONE', #42910, 39.37007874015748143 ) ;
#46329 = ORIENTED_EDGE ( 'NONE', *, *, #35774, .T. ) ;
#46330 = ORIENTED_EDGE ( 'NONE', *, *, #3173, .T. ) ;
#46331 = DIRECTION ( 'NONE',  ( 1.000000000000000000, 0.000000000000000000, 0.000000000000000000 ) ) ;
#46332 = CARTESIAN_POINT ( 'NONE',  ( -1.225600105435525000, 0.000000000000000000, -1.239880218767125175 ) ) ;
#46333 = VECTOR ( 'NONE', #19502, 39.37007874015748143 ) ;
#46334 = CARTESIAN_POINT ( 'NONE',  ( -1.636583440222563635, 3.346456692913386100, 0.1181102362204704270 ) ) ;
#46335 = CARTESIAN_POINT ( 'NONE',  ( 0.7423782071083087075, 3.346456692913386100, -0.9448818897637765168 ) ) ;
#46336 = CARTESIAN_POINT ( 'NONE',  ( -1.862188077367287642, 3.346456692913386100, -0.9842519685039344823 ) ) ;
#46337 = CARTESIAN_POINT ( 'NONE',  ( 0.000000000000000000, 1.585169487999011917, 0.000000000000000000 ) ) ;
#46338 = AXIS2_PLACEMENT_3D ( 'NONE', #24047, #37213, #41086 ) ;
#46339 = ORIENTED_EDGE ( 'NONE', *, *, #46347, .F. ) ;
#46340 = ORIENTED_EDGE ( 'NONE', *, *, #44447, .F. ) ;
#46341 = DIRECTION ( 'NONE',  ( -0.000000000000000000, 1.000000000000000000, -0.000000000000000000 ) ) ;
#46342 = LINE ( 'NONE', #30378, #31425 ) ;
#46343 = EDGE_LOOP ( 'NONE', ( #40860, #37690, #38826, #19808 ) ) ;
#46344 = CARTESIAN_POINT ( 'NONE',  ( 1.214590356376888280, 1.727355838235203667, 1.936932008856820930 ) ) ;
#46345 = ORIENTED_EDGE ( 'NONE', *, *, #9824, .F. ) ;
#46346 = ORIENTED_EDGE ( 'NONE', *, *, #5355, .F. ) ;
#46347 = EDGE_CURVE ( 'NONE', #695, #24400, #21422, .T. ) ;
#46348 = ADVANCED_FACE ( 'NONE', ( #33056 ), #16787, .F. ) ;
#46349 = EDGE_LOOP ( 'NONE', ( #3328, #22424, #5944, #14984 ) ) ;
#46350 = ORIENTED_EDGE ( 'NONE', *, *, #48322, .T. ) ;
#46351 = CARTESIAN_POINT ( 'NONE',  ( 0.000000000000000000, 3.267716535433071279, 0.4724409448818868706 ) ) ;
#46352 = EDGE_CURVE ( 'NONE', #42837, #7418, #17798, .T. ) ;
#46353 = EDGE_CURVE ( 'NONE', #33976, #8620, #9316, .T. ) ;
#46354 = LINE ( 'NONE', #47100, #22160 ) ;
#46355 = CARTESIAN_POINT ( 'NONE',  ( 5.361844333726674129E-17, 6.389997247649651107E-17, -0.7480314960629920185 ) ) ;
#46356 = VECTOR ( 'NONE', #16792, 39.37007874015748143 ) ;
#46357 = DIRECTION ( 'NONE',  ( 1.000000000000000000, 0.000000000000000000, 0.000000000000000000 ) ) ;
#46358 = VECTOR ( 'NONE', #45836, 39.37007874015748143 ) ;
#46359 = LINE ( 'NONE', #30901, #44286 ) ;
#46360 = DIRECTION ( 'NONE',  ( 0.000000000000000000, 0.000000000000000000, 1.000000000000000000 ) ) ;
#46361 = EDGE_LOOP ( 'NONE', ( #19381, #29477, #18159, #41397 ) ) ;
#46362 = FACE_OUTER_BOUND ( 'NONE', #6311, .T. ) ;
#46363 = CARTESIAN_POINT ( 'NONE',  ( 1.723687301221656476, 1.205361022782829114E-17, -1.311649477509800876 ) ) ;
#46364 = VECTOR ( 'NONE', #4632, 39.37007874015748143 ) ;
#46365 = CARTESIAN_POINT ( 'NONE',  ( -2.576863348864732117, 1.580667355030889620, 1.442554885838411849 ) ) ;
#46366 = FACE_OUTER_BOUND ( 'NONE', #14469, .T. ) ;
#46367 = VECTOR ( 'NONE', #48193, 39.37007874015748143 ) ;
#46368 = VECTOR ( 'NONE', #50027, 39.37007874015748143 ) ;
#46369 = ORIENTED_EDGE ( 'NONE', *, *, #42170, .F. ) ;
#46370 = LINE ( 'NONE', #19023, #8368 ) ;
#46371 = LINE ( 'NONE', #14909, #7144 ) ;
#46372 = ORIENTED_EDGE ( 'NONE', *, *, #33760, .T. ) ;
#46373 = CARTESIAN_POINT ( 'NONE',  ( 0.1968503937007872462, 3.267716535433071279, -1.141732283464564013 ) ) ;
#46374 = CARTESIAN_POINT ( 'NONE',  ( 1.292259323372447977, 1.002375609920205468, 2.258827622949058700 ) ) ;
#46375 = CARTESIAN_POINT ( 'NONE',  ( 0.002207914879453961535, -5.712274067634378313E-18, 0.04916304461325374242 ) ) ;
#46376 = VERTEX_POINT ( 'NONE', #28898 ) ;
#46377 = PLANE ( 'NONE',  #14078 ) ;
#46378 = PLANE ( 'NONE',  #11056 ) ;
#46379 = DIRECTION ( 'NONE',  ( -0.01601477604151182663, 0.9998717552508123996, -0.000000000000000000 ) ) ;
#46380 = CARTESIAN_POINT ( 'NONE',  ( 1.636583440222563857, 3.267716535433071279, -1.161035397307311917E-15 ) ) ;
#46381 = DIRECTION ( 'NONE',  ( 1.000000000000000000, 0.000000000000000000, 0.000000000000000000 ) ) ;
#46382 = VERTEX_POINT ( 'NONE', #21675 ) ;
#46383 = LINE ( 'NONE', #26788, #20572 ) ;
#46384 = EDGE_CURVE ( 'NONE', #48435, #3807, #12914, .T. ) ;
#46385 = VERTEX_POINT ( 'NONE', #44633 ) ;
#46386 = VERTEX_POINT ( 'NONE', #9033 ) ;
#46387 = EDGE_CURVE ( 'NONE', #11755, #9111, #33308, .T. ) ;
#46388 = DIRECTION ( 'NONE',  ( 1.000000000000000000, 0.000000000000000000, -3.469446951953613696E-16 ) ) ;
#46389 = ORIENTED_EDGE ( 'NONE', *, *, #41954, .T. ) ;
#46390 = DIRECTION ( 'NONE',  ( -0.000000000000000000, 1.000000000000000000, -0.000000000000000000 ) ) ;
#46391 = DIRECTION ( 'NONE',  ( 0.000000000000000000, 0.000000000000000000, 1.000000000000000000 ) ) ;
#46392 = ORIENTED_EDGE ( 'NONE', *, *, #2415, .T. ) ;
#46393 = ADVANCED_FACE ( 'NONE', ( #48993 ), #9288, .F. ) ;
#46394 = CARTESIAN_POINT ( 'NONE',  ( 0.4696143004045479352, 3.346456692913386100, 0.7874015748031454320 ) ) ;
#46395 = LINE ( 'NONE', #42548, #43052 ) ;
#46396 = AXIS2_PLACEMENT_3D ( 'NONE', #42922, #15573, #46279 ) ;
#46397 = CARTESIAN_POINT ( 'NONE',  ( -0.8013691390275965443, 1.531806867628318747, -2.841978980033345703 ) ) ;
#46398 = ORIENTED_EDGE ( 'NONE', *, *, #13481, .T. ) ;
#46399 = EDGE_LOOP ( 'NONE', ( #15298, #15394, #37620, #45980 ) ) ;
#46400 = DIRECTION ( 'NONE',  ( 1.734723475976806848E-16, 0.000000000000000000, 1.000000000000000000 ) ) ;
#46401 = FACE_BOUND ( 'NONE', #41528, .T. ) ;
#46402 = ORIENTED_EDGE ( 'NONE', *, *, #29197, .T. ) ;
#46403 = VECTOR ( 'NONE', #41820, 39.37007874015748143 ) ;
#46404 = VECTOR ( 'NONE', #44350, 39.37007874015748143 ) ;
#46405 = LINE ( 'NONE', #22690, #12179 ) ;
#46406 = EDGE_CURVE ( 'NONE', #44433, #31184, #5154, .T. ) ;
#46407 = ORIENTED_EDGE ( 'NONE', *, *, #37705, .F. ) ;
#46408 = ORIENTED_EDGE ( 'NONE', *, *, #43378, .T. ) ;
#46409 = FACE_OUTER_BOUND ( 'NONE', #45192, .T. ) ;
#46410 = CARTESIAN_POINT ( 'NONE',  ( 0.000000000000000000, 3.267716535433071279, 1.102362204724404160 ) ) ;
#46411 = ADVANCED_FACE ( 'NONE', ( #20906 ), #40788, .T. ) ;
#46412 = VERTEX_POINT ( 'NONE', #2053 ) ;
#46413 = CARTESIAN_POINT ( 'NONE',  ( 1.287906020515830141, 3.346456692913386100, -0.9448818897637765168 ) ) ;
#46414 = ORIENTED_EDGE ( 'NONE', *, *, #45485, .T. ) ;
#46415 = CARTESIAN_POINT ( 'NONE',  ( -1.439733046521776139, 0.000000000000000000, 0.6299212598425164567 ) ) ;
#46416 = CARTESIAN_POINT ( 'NONE',  ( -1.636583440222563635, 0.000000000000000000, 0.4330708661417290162 ) ) ;
#46417 = LINE ( 'NONE', #46170, #23908 ) ;
#46418 = VERTEX_POINT ( 'NONE', #24526 ) ;
#46419 = VERTEX_POINT ( 'NONE', #5414 ) ;
#46420 = CARTESIAN_POINT ( 'NONE',  ( 0.5110784536613244278, 1.503363781114207764, 2.908235870722285288 ) ) ;
#46421 = CARTESIAN_POINT ( 'NONE',  ( -1.985260859929297572, 3.346456692913386100, 0.9448818897637749625 ) ) ;
#46422 = CARTESIAN_POINT ( 'NONE',  ( 0.08139965876239094178, 1.610780518492231694, 0.000000000000000000 ) ) ;
#46423 = EDGE_CURVE ( 'NONE', #11518, #27975, #4902, .T. ) ;
#46424 = CARTESIAN_POINT ( 'NONE',  ( -1.195183497228115035E-16, 3.267716535433071279, -0.6299212598425177889 ) ) ;
#46425 = CARTESIAN_POINT ( 'NONE',  ( -2.165177485265404655, 1.574805878788816393, -0.03196544748097695371 ) ) ;
#46426 = DIRECTION ( 'NONE',  ( 1.000000000000000000, 1.288287287306305283E-16, -0.000000000000000000 ) ) ;
#46427 = DIRECTION ( 'NONE',  ( -1.000000000000000000, 0.000000000000000000, 0.000000000000000000 ) ) ;
#46428 = VECTOR ( 'NONE', #9864, 39.37007874015748143 ) ;
#46429 = ORIENTED_EDGE ( 'NONE', *, *, #39764, .F. ) ;
#46430 = DIRECTION ( 'NONE',  ( -0.000000000000000000, 1.000000000000000000, -0.000000000000000000 ) ) ;
#46431 = CARTESIAN_POINT ( 'NONE',  ( 2.491402175429653809, 1.458524810485662959, -1.585592796919505609 ) ) ;
#46432 = VECTOR ( 'NONE', #30603, 39.37007874015748143 ) ;
#46433 = ORIENTED_EDGE ( 'NONE', *, *, #12441, .F. ) ;
#46434 = VECTOR ( 'NONE', #23882, 39.37007874015748143 ) ;
#46435 = ORIENTED_EDGE ( 'NONE', *, *, #3340, .T. ) ;
#46436 = B_SPLINE_CURVE_WITH_KNOTS ( 'NONE', 3,
 ( #46041, #15584, #35206, #15079 ),
 .UNSPECIFIED., .F., .F.,
 ( 4, 4 ),
 ( 6.541964665659682645E-07, 0.004810142676841229654 ),
 .UNSPECIFIED. ) ;
#46438 = VECTOR ( 'NONE', #17633, 39.37007874015748143 ) ;
#46437 = CARTESIAN_POINT ( 'NONE',  ( 0.5469786881612729301, 0.03668053021573630668, -1.796948620166157307 ) ) ;
#46439 = B_SPLINE_CURVE_WITH_KNOTS ( 'NONE', 3,
 ( #38911, #46374, #50719, #3799 ),
 .UNSPECIFIED., .F., .F.,
 ( 4, 4 ),
 ( 3.948084238142846119E-07, 0.04530798946647138226 ),
 .UNSPECIFIED. ) ;
#46440 = DIRECTION ( 'NONE',  ( -0.3513748240813434620, 0.000000000000000000, 0.9362348706397368714 ) ) ;
#46441 = VERTEX_POINT ( 'NONE', #29156 ) ;
#46442 = VECTOR ( 'NONE', #24624, 39.37007874015748143 ) ;
#46443 = EDGE_CURVE ( 'NONE', #619, #42699, #1284, .T. ) ;
#46444 = VERTEX_POINT ( 'NONE', #41049 ) ;
#46445 = DIRECTION ( 'NONE',  ( -1.000000000000000000, -0.000000000000000000, -0.000000000000000000 ) ) ;
#46446 = ORIENTED_EDGE ( 'NONE', *, *, #33052, .F. ) ;
#46447 = EDGE_CURVE ( 'NONE', #13689, #25755, #24685, .T. ) ;
#46448 = FACE_OUTER_BOUND ( 'NONE', #40570, .T. ) ;
#46449 = CARTESIAN_POINT ( 'NONE',  ( -0.8182917201112818173, 3.267716535433071279, 1.419509857074483292E-16 ) ) ;
#46450 = EDGE_CURVE ( 'NONE', #782, #33984, #26552, .T. ) ;
#46451 = EDGE_CURVE ( 'NONE', #2129, #38287, #21933, .T. ) ;
#46452 = ORIENTED_EDGE ( 'NONE', *, *, #46252, .F. ) ;
#46453 = DIRECTION ( 'NONE',  ( -0.01601477604151182663, 0.9998717552508123996, -0.000000000000000000 ) ) ;
#46454 = ORIENTED_EDGE ( 'NONE', *, *, #29873, .T. ) ;
#46455 = ORIENTED_EDGE ( 'NONE', *, *, #41479, .T. ) ;
#46456 = CARTESIAN_POINT ( 'NONE',  ( -1.363819533518803473, 3.346456692913386100, 1.605145679676863057 ) ) ;
#46457 = DIRECTION ( 'NONE',  ( 0.8090169943749506709, 0.000000000000000000, -0.5877852522924684742 ) ) ;
#46458 = DIRECTION ( 'NONE',  ( 1.000000000000000000, -0.000000000000000000, 0.000000000000000000 ) ) ;
#46459 = ORIENTED_EDGE ( 'NONE', *, *, #46260, .F. ) ;
#46460 = DIRECTION ( 'NONE',  ( -1.000000000000000000, 0.000000000000000000, -0.000000000000000000 ) ) ;
#46461 = ADVANCED_FACE ( 'NONE', ( #14940 ), #42298, .T. ) ;
#46462 = FACE_OUTER_BOUND ( 'NONE', #20634, .T. ) ;
#46463 = VERTEX_POINT ( 'NONE', #22687 ) ;
#46464 = LINE ( 'NONE', #46957, #43826 ) ;
#46465 = AXIS2_PLACEMENT_3D ( 'NONE', #10311, #6184, #2566 ) ;
#46466 = CIRCLE ( 'NONE', #6115, 1.850107469027523432 ) ;
#46467 = EDGE_CURVE ( 'NONE', #48458, #2485, #2816, .T. ) ;
#46468 = ORIENTED_EDGE ( 'NONE', *, *, #4236, .F. ) ;
#46469 = VECTOR ( 'NONE', #21651, 39.37007874015748143 ) ;
#46470 = EDGE_LOOP ( 'NONE', ( #39005, #28521, #46844, #29925 ) ) ;
#46471 = VECTOR ( 'NONE', #43720, 39.37007874015748143 ) ;
#46472 = DIRECTION ( 'NONE',  ( -1.118904554427321068E-16, -1.000000000000000000, -3.087980359898530052E-17 ) ) ;
#46473 = VECTOR ( 'NONE', #34349, 39.37007874015748143 ) ;
#46474 = PLANE ( 'NONE',  #20026 ) ;
#46475 = EDGE_CURVE ( 'NONE', #29709, #43175, #38196, .T. ) ;
#46476 = CARTESIAN_POINT ( 'NONE',  ( 1.015142113812069757, 3.267716535433071279, -3.521981712565033375E-16 ) ) ;
#46477 = CARTESIAN_POINT ( 'NONE',  ( 0.000000000000000000, 2.755905511811024056, -1.181102362204723200 ) ) ;
#46478 = ORIENTED_EDGE ( 'NONE', *, *, #1847, .F. ) ;
#46479 = ORIENTED_EDGE ( 'NONE', *, *, #39354, .T. ) ;
#46480 = CARTESIAN_POINT ( 'NONE',  ( -1.166969139818015533, 3.267716535433071279, 0.1574803149606287811 ) ) ;
#46481 = CARTESIAN_POINT ( 'NONE',  ( 1.363819533518803251, 0.000000000000000000, 0.4724409448818871482 ) ) ;
#46482 = VERTEX_POINT ( 'NONE', #30687 ) ;
#46483 = DIRECTION ( 'NONE',  ( -0.000000000000000000, -1.000000000000000000, -0.000000000000000000 ) ) ;
#46484 = ADVANCED_FACE ( 'NONE', ( #6437 ), #18306, .F. ) ;
#46485 = CARTESIAN_POINT ( 'NONE',  ( -2.875074555560396483, 1.574099885360915829, -0.6730399204671311253 ) ) ;
#46486 = LINE ( 'NONE', #2900, #30812 ) ;
#46487 = CARTESIAN_POINT ( 'NONE',  ( 1.091055626815042645, 0.000000000000000000, 0.9448818897637746295 ) ) ;
#46488 = DIRECTION ( 'NONE',  ( -1.953992523340275196E-14, 0.000000000000000000, 1.000000000000000000 ) ) ;
#46489 = ORIENTED_EDGE ( 'NONE', *, *, #37710, .T. ) ;
#46490 = CARTESIAN_POINT ( 'NONE',  ( 0.7145799201508782339, 6.692913385826772199, 2.044048657746659448 ) ) ;
#46491 = CARTESIAN_POINT ( 'NONE',  ( -1.181102362204724088, 0.000000000000000000, 1.062992125984251635 ) ) ;
#46492 = EDGE_CURVE ( 'NONE', #49974, #23541, #34812, .T. ) ;
#46493 = CARTESIAN_POINT ( 'NONE',  ( -0.8942052331142552601, 3.346456692913386100, -1.141732283464563569 ) ) ;
#46494 = ORIENTED_EDGE ( 'NONE', *, *, #7190, .F. ) ;
#46495 = CARTESIAN_POINT ( 'NONE',  ( -1.166969139818015533, 0.000000000000000000, 0.1574803149606287811 ) ) ;
#46496 = CARTESIAN_POINT ( 'NONE',  ( -1.439733046521776139, 3.346456692913386100, 0.3149606299212578953 ) ) ;
#46497 = LINE ( 'NONE', #26651, #13945 ) ;
#46498 = ORIENTED_EDGE ( 'NONE', *, *, #27240, .F. ) ;
#46499 = CARTESIAN_POINT ( 'NONE',  ( -2.473328087642055362, 1.582272202671235473, -1.612973869535263338 ) ) ;
#46500 = B_SPLINE_CURVE_WITH_KNOTS ( 'NONE', 3,
 ( #44385, #9283, #24778, #40272 ),
 .UNSPECIFIED., .F., .F.,
 ( 4, 4 ),
 ( 5.909393220007465840E-06, 0.002506742884191285031 ),
 .UNSPECIFIED. ) ;
#46501 = VECTOR ( 'NONE', #6006, 39.37007874015748143 ) ;
#46502 = ORIENTED_EDGE ( 'NONE', *, *, #38718, .F. ) ;
#46503 = AXIS2_PLACEMENT_3D ( 'NONE', #28825, #32724, #44559 ) ;
#46504 = CARTESIAN_POINT ( 'NONE',  ( 0.000000000000000000, 5.905511811023623991, 0.000000000000000000 ) ) ;
#46505 = ORIENTED_EDGE ( 'NONE', *, *, #29716, .F. ) ;
#46506 = CARTESIAN_POINT ( 'NONE',  ( 0.5455278134075217666, 3.267716535433071279, 1.259842519685033357 ) ) ;
#46507 = VECTOR ( 'NONE', #36384, 39.37007874015748143 ) ;
#46508 = ORIENTED_EDGE ( 'NONE', *, *, #42151, .F. ) ;
#46509 = EDGE_CURVE ( 'NONE', #46515, #14938, #18817, .T. ) ;
#46510 = CIRCLE ( 'NONE', #16885, 1.181102362204723200 ) ;
#46511 = CARTESIAN_POINT ( 'NONE',  ( 1.174087487603957980, 6.692913385826772199, 1.869141625116387928 ) ) ;
#46512 = CARTESIAN_POINT ( 'NONE',  ( 2.164658444855302122, 5.905511811023623991, -0.04795272066889885720 ) ) ;
#46513 = DIRECTION ( 'NONE',  ( 0.000000000000000000, 0.000000000000000000, -1.000000000000000000 ) ) ;
#46514 = ADVANCED_FACE ( 'NONE', ( #34062 ), #34321, .F. ) ;
#46515 = VERTEX_POINT ( 'NONE', #50253 ) ;
#46516 = ORIENTED_EDGE ( 'NONE', *, *, #46571, .T. ) ;
#46517 = ORIENTED_EDGE ( 'NONE', *, *, #7563, .F. ) ;
#46518 = CARTESIAN_POINT ( 'NONE',  ( -1.062992125984250968, 0.4724409448818890911, 1.181102362204724088 ) ) ;
#46519 = DIRECTION ( 'NONE',  ( 0.000000000000000000, -0.9063077870366510469, -0.4226182617406972208 ) ) ;
#46520 = ORIENTED_EDGE ( 'NONE', *, *, #50818, .F. ) ;
#46521 = CARTESIAN_POINT ( 'NONE',  ( 0.2727639067037610499, 3.346456692913386100, 2.047244094488179567 ) ) ;
#46522 = CARTESIAN_POINT ( 'NONE',  ( -0.8182917201112819283, 3.346456692913386100, -2.244094488188968395 ) ) ;
#46523 = PLANE ( 'NONE',  #49962 ) ;
#46524 = ORIENTED_EDGE ( 'NONE', *, *, #41127, .F. ) ;
#46525 = EDGE_LOOP ( 'NONE', ( #2728, #39174, #7579, #40379 ) ) ;
#46526 = LINE ( 'NONE', #11947, #2394 ) ;
#46527 = DIRECTION ( 'NONE',  ( -0.000000000000000000, 1.000000000000000000, -0.000000000000000000 ) ) ;
#46528 = FACE_OUTER_BOUND ( 'NONE', #16984, .T. ) ;
#46529 = ORIENTED_EDGE ( 'NONE', *, *, #48842, .F. ) ;
#46530 =( NAMED_UNIT ( * ) SI_UNIT ( $, .STERADIAN. ) SOLID_ANGLE_UNIT ( ) );
#46531 = DIRECTION ( 'NONE',  ( -3.469446951953613696E-16, 0.000000000000000000, -1.000000000000000000 ) ) ;
#46532 = VERTEX_POINT ( 'NONE', #30440 ) ;
#46533 = CARTESIAN_POINT ( 'NONE',  ( -0.9494510123445516481, 1.031098797897046948, 2.389745905932011194 ) ) ;
#46534 = ORIENTED_EDGE ( 'NONE', *, *, #35532, .F. ) ;
#46535 = ORIENTED_EDGE ( 'NONE', *, *, #6058, .T. ) ;
#46536 = DIRECTION ( 'NONE',  ( -0.000000000000000000, 1.000000000000000000, -0.000000000000000000 ) ) ;
#46537 = DIRECTION ( 'NONE',  ( -0.000000000000000000, 1.000000000000000000, -0.000000000000000000 ) ) ;
#46538 = DIRECTION ( 'NONE',  ( -3.469446951953613696E-16, 0.000000000000000000, -1.000000000000000000 ) ) ;
#46539 = EDGE_CURVE ( 'NONE', #24400, #13689, #16081, .T. ) ;
#46540 = DIRECTION ( 'NONE',  ( 5.063291518728965670E-17, 1.000000000000000000, 1.184615939703122503E-16 ) ) ;
#46541 = CARTESIAN_POINT ( 'NONE',  ( 0.07982360342473591996, 1.709180471932028711, 0.000000000000000000 ) ) ;
#46542 = ORIENTED_EDGE ( 'NONE', *, *, #6158, .T. ) ;
#46543 = VECTOR ( 'NONE', #50332, 39.37007874015748143 ) ;
#46544 = AXIS2_PLACEMENT_3D ( 'NONE', #35911, #27379, #42631 ) ;
#46545 = ORIENTED_EDGE ( 'NONE', *, *, #1908, .F. ) ;
#46546 = LINE ( 'NONE', #26948, #43384 ) ;
#46547 = ADVANCED_FACE ( 'NONE', ( #7200 ), #10562, .F. ) ;
#46548 = DIRECTION ( 'NONE',  ( -0.7818314824680309139, 0.000000000000000000, 0.6234898018587318180 ) ) ;
#46549 = AXIS2_PLACEMENT_3D ( 'NONE', #32141, #8890, #23610 ) ;
#46550 = EDGE_CURVE ( 'NONE', #33305, #11733, #19056, .T. ) ;
#46551 = EDGE_CURVE ( 'NONE', #6600, #46139, #13932, .T. ) ;
#46552 = DIRECTION ( 'NONE',  ( -3.469446951953613696E-16, 0.000000000000000000, -1.000000000000000000 ) ) ;
#46553 = CARTESIAN_POINT ( 'NONE',  ( 2.100227814008711835, 1.653522055412836700, -2.076109931251913565 ) ) ;
#46554 = VECTOR ( 'NONE', #15429, 39.37007874015748143 ) ;
#46555 = ORIENTED_EDGE ( 'NONE', *, *, #9698, .F. ) ;
#46556 = CARTESIAN_POINT ( 'NONE',  ( -0.6214413264104945434, 3.346456692913386100, 1.850393700787391849 ) ) ;
#46557 = EDGE_CURVE ( 'NONE', #42496, #4027, #22438, .T. ) ;
#46558 = DIRECTION ( 'NONE',  ( 0.000000000000000000, 0.7071067811865466846, 0.7071067811865483499 ) ) ;
#46559 = ADVANCED_FACE ( 'NONE', ( #2305 ), #41548, .F. ) ;
#46560 = ORIENTED_EDGE ( 'NONE', *, *, #31613, .T. ) ;
#46561 = FACE_OUTER_BOUND ( 'NONE', #38988, .T. ) ;
#46562 = DIRECTION ( 'NONE',  ( -1.000000000000000000, 0.000000000000000000, 1.734723475976806848E-16 ) ) ;
#46563 = CYLINDRICAL_SURFACE ( 'NONE', #9000, 2.165354330708661568 ) ;
#46564 = DIRECTION ( 'NONE',  ( -0.000000000000000000, 1.000000000000000000, -0.000000000000000000 ) ) ;
#46565 = CARTESIAN_POINT ( 'NONE',  ( 1.181102362204724532, 0.000000000000000000, 1.062992125984251413 ) ) ;
#46566 = FACE_OUTER_BOUND ( 'NONE', #27365, .T. ) ;
#46567 = VERTEX_POINT ( 'NONE', #43044 ) ;
#46568 = LINE ( 'NONE', #30099, #32942 ) ;
#46569 = VERTEX_POINT ( 'NONE', #39187 ) ;
#46570 = CARTESIAN_POINT ( 'NONE',  ( 2.793030215715258446, 5.905511811023623991, 0.9592557174602684977 ) ) ;
#46571 = EDGE_CURVE ( 'NONE', #45040, #31775, #23183, .T. ) ;
#46572 = DIRECTION ( 'NONE',  ( -3.469446951953613696E-16, 0.000000000000000000, -1.000000000000000000 ) ) ;
#46573 = FACE_OUTER_BOUND ( 'NONE', #35977, .T. ) ;
#46574 = EDGE_CURVE ( 'NONE', #17100, #8967, #31449, .T. ) ;
#46575 = ORIENTED_EDGE ( 'NONE', *, *, #10574, .T. ) ;
#46576 = ORIENTED_EDGE ( 'NONE', *, *, #8696, .F. ) ;
#46577 = CARTESIAN_POINT ( 'NONE',  ( 2.152681973165668783, 1.676764294869834693, -0.8665810060396648140 ) ) ;
#46578 = CIRCLE ( 'NONE', #27646, 2.165354330708661568 ) ;
#46579 = ADVANCED_FACE ( 'NONE', ( #31194 ), #24056, .T. ) ;
#46580 = LINE ( 'NONE', #38369, #4040 ) ;
#46581 = VECTOR ( 'NONE', #10370, 39.37007874015748143 ) ;
#46582 = CARTESIAN_POINT ( 'NONE',  ( 2.298708793198899869, 5.118110236220475784, 1.181102362204724310 ) ) ;
#46583 = CARTESIAN_POINT ( 'NONE',  ( 1.772156216928421291, 1.703477877919150618, 1.476192699911957451 ) ) ;
#46584 = CARTESIAN_POINT ( 'NONE',  ( 0.1968503937007878568, 3.267716535433071279, 1.574803149606291974 ) ) ;
#46585 = AXIS2_PLACEMENT_3D ( 'NONE', #48, #12437, #31557 ) ;
#46586 = DIRECTION ( 'NONE',  ( 0.000000000000000000, 0.000000000000000000, 1.000000000000000000 ) ) ;
#46587 = VERTEX_POINT ( 'NONE', #35325 ) ;
#46588 = DIRECTION ( 'NONE',  ( -0.9998717552508121775, -0.01601477604151182663, 0.000000000000000000 ) ) ;
#46589 = CARTESIAN_POINT ( 'NONE',  ( 1.363819533518803251, 3.267716535433071279, 0.1574803149606283648 ) ) ;
#46590 = LINE ( 'NONE', #23371, #32281 ) ;
#46591 = VECTOR ( 'NONE', #8638, 39.37007874015748143 ) ;
#46592 = EDGE_LOOP ( 'NONE', ( #50481, #44525, #17500, #34632 ) ) ;
#46593 = CARTESIAN_POINT ( 'NONE',  ( -2.043634885149970160, 1.574803149606302854, 0.7157624142945940848 ) ) ;
#46594 = EDGE_LOOP ( 'NONE', ( #11297, #2355, #118, #10609 ) ) ;
#46595 = EDGE_LOOP ( 'NONE', ( #36486, #2642, #1045, #11121 ) ) ;
#46596 = EDGE_LOOP ( 'NONE', ( #18927, #10067, #15304, #45655 ) ) ;
#46597 = ORIENTED_EDGE ( 'NONE', *, *, #50257, .T. ) ;
#46598 = CARTESIAN_POINT ( 'NONE',  ( 0.5546681269544795345, 1.683977579361253696, -2.194778965963542383 ) ) ;
#46599 = B_SPLINE_CURVE_WITH_KNOTS ( 'NONE', 3,
 ( #37362, #33748, #36590, #9732 ),
 .UNSPECIFIED., .F., .F.,
 ( 4, 4 ),
 ( 0.0004380968183548472812, 0.002938328190805584474 ),
 .UNSPECIFIED. ) ;
#46600 = CARTESIAN_POINT ( 'NONE',  ( 0.8182917201112819283, 0.000000000000000000, -0.1574803149606301411 ) ) ;
#46601 = DIRECTION ( 'NONE',  ( 0.000000000000000000, 1.000000000000000000, 0.000000000000000000 ) ) ;
#46602 = CARTESIAN_POINT ( 'NONE',  ( -1.567214440306964107, 0.002817858044914879883, 0.7874684655159520652 ) ) ;
#46603 = EDGE_CURVE ( 'NONE', #37684, #4024, #38937, .T. ) ;
#46604 = B_SPLINE_CURVE_WITH_KNOTS ( 'NONE', 3,
 ( #25878, #41627, #6258, #22012 ),
 .UNSPECIFIED., .F., .F.,
 ( 4, 4 ),
 ( 0.0006403145629956773222, 0.003140563976786123635 ),
 .UNSPECIFIED. ) ;
#46605 = ADVANCED_FACE ( 'NONE', ( #7446 ), #27305, .F. ) ;
#46606 = CARTESIAN_POINT ( 'NONE',  ( -2.137971680030238186, 1.583472898301503173, 1.642030245039320713 ) ) ;
#46607 = EDGE_CURVE ( 'NONE', #18135, #448, #35069, .T. ) ;
#46608 = DIRECTION ( 'NONE',  ( -1.000000000000000000, 0.000000000000000000, -0.000000000000000000 ) ) ;
#46609 = DIRECTION ( 'NONE',  ( 0.000000000000000000, 0.000000000000000000, -1.000000000000000000 ) ) ;
#46610 = CONICAL_SURFACE ( 'NONE', #13669, 3.483074324928249421, 1.244861948955335196 ) ;
#46611 = ORIENTED_EDGE ( 'NONE', *, *, #4614, .F. ) ;
#46612 = CARTESIAN_POINT ( 'NONE',  ( 1.363819533518803251, 3.346456692913386100, 1.417322834645662777 ) ) ;
#46613 = CARTESIAN_POINT ( 'NONE',  ( 0.000000000000000000, 3.267716535433071279, -1.141732283464564013 ) ) ;
#46614 = AXIS2_PLACEMENT_3D ( 'NONE', #33981, #7363, #49664 ) ;
#46615 = LINE ( 'NONE', #27013, #3750 ) ;
#46616 = VECTOR ( 'NONE', #10493, 39.37007874015748143 ) ;
#46617 = CARTESIAN_POINT ( 'NONE',  ( 1.647640870277422342, 0.000000000000000000, 1.293031892269974170 ) ) ;
#46618 = ORIENTED_EDGE ( 'NONE', *, *, #4041, .F. ) ;
#46619 = FACE_OUTER_BOUND ( 'NONE', #2146, .T. ) ;
#46620 = CARTESIAN_POINT ( 'NONE',  ( 0.2727639067037603837, 3.267716535433071279, -4.731699523581606660E-17 ) ) ;
#46621 = EDGE_LOOP ( 'NONE', ( #31570, #40573, #30385, #15974 ) ) ;
#46622 = CARTESIAN_POINT ( 'NONE',  ( 1.287906020515829919, 0.000000000000000000, -1.259842519685035134 ) ) ;
#46623 = AXIS2_PLACEMENT_3D ( 'NONE', #32612, #847, #44962 ) ;
#46624 = CARTESIAN_POINT ( 'NONE',  ( 0.000000000000000000, 2.755905511811024056, 0.000000000000000000 ) ) ;
#46625 = PRODUCT_DEFINITION_SHAPE ( 'NONE', 'NONE',  #47367 ) ;
#46626 = LINE ( 'NONE', #34541, #4311 ) ;
#46627 = ADVANCED_FACE ( 'NONE', ( #11318 ), #47660, .F. ) ;
#46628 = ORIENTED_EDGE ( 'NONE', *, *, #5257, .T. ) ;
#46629 = CARTESIAN_POINT ( 'NONE',  ( -0.2727639067037611054, 3.346456692913386100, -2.244094488188968395 ) ) ;
#46630 = LINE ( 'NONE', #42781, #33366 ) ;
#46631 = DIRECTION ( 'NONE',  ( -0.01601477604151182663, 0.9998717552508123996, -0.000000000000000000 ) ) ;
#46632 = EDGE_CURVE ( 'NONE', #6627, #19810, #15448, .T. ) ;
#46633 = CARTESIAN_POINT ( 'NONE',  ( 2.734482843737263025, 1.761870738172414796, -1.115254632218672493 ) ) ;
#46634 = DIRECTION ( 'NONE',  ( -0.000000000000000000, 1.000000000000000000, -0.000000000000000000 ) ) ;
#46635 = ORIENTED_EDGE ( 'NONE', *, *, #49959, .F. ) ;
#46636 = ADVANCED_FACE ( 'NONE', ( #43813 ), #3568, .F. ) ;
#46637 = VERTEX_POINT ( 'NONE', #39700 ) ;
#46638 = ORIENTED_EDGE ( 'NONE', *, *, #48701, .F. ) ;
#46639 = LINE ( 'NONE', #3557, #3965 ) ;
#46640 = ADVANCED_FACE ( 'NONE', ( #4590 ), #35602, .T. ) ;
#46641 = EDGE_LOOP ( 'NONE', ( #47725, #31584, #21508, #9427 ) ) ;
#46642 = DIRECTION ( 'NONE',  ( -0.000000000000000000, -1.000000000000000000, -0.000000000000000000 ) ) ;
#46643 = CARTESIAN_POINT ( 'NONE',  ( 1.636583440222563857, 0.000000000000000000, 0.3149606299212576177 ) ) ;
#46644 = ORIENTED_EDGE ( 'NONE', *, *, #40909, .F. ) ;
#46645 = LINE ( 'NONE', #15685, #39616 ) ;
#46646 = DIRECTION ( 'NONE',  ( 1.042246309068005903E-16, 1.000000000000000000, -7.572362681945165783E-17 ) ) ;
#46647 = AXIS2_PLACEMENT_3D ( 'NONE', #11718, #4227, #3980 ) ;
#46648 = CIRCLE ( 'NONE', #31880, 2.165354330708661568 ) ;
#46649 = ORIENTED_EDGE ( 'NONE', *, *, #37125, .T. ) ;
#46650 = ORIENTED_EDGE ( 'NONE', *, *, #13060, .T. ) ;
#46651 = AXIS2_PLACEMENT_3D ( 'NONE', #32494, #20078, #20859 ) ;
#46652 = DIRECTION ( 'NONE',  ( -0.01601477604151182663, 0.9998717552508123996, -0.000000000000000000 ) ) ;
#46653 = FACE_BOUND ( 'NONE', #2929, .T. ) ;
#46654 = VERTEX_POINT ( 'NONE', #27562 ) ;
#46655 = VECTOR ( 'NONE', #14559, 39.37007874015748143 ) ;
#46656 = DIRECTION ( 'NONE',  ( 1.000000000000000000, 0.000000000000000000, 0.000000000000000000 ) ) ;
#46657 = VERTEX_POINT ( 'NONE', #12080 ) ;
#46658 = EDGE_LOOP ( 'NONE', ( #44702, #35089, #40116, #45235 ) ) ;
#46659 = CARTESIAN_POINT ( 'NONE',  ( 0.000000000000000000, 3.267716535433071279, 0.4724409448818868706 ) ) ;
#46660 = AXIS2_PLACEMENT_3D ( 'NONE', #125, #3756, #31126 ) ;
#46661 = DIRECTION ( 'NONE',  ( 0.9998717552508121775, 0.01601477604151182663, 0.000000000000000000 ) ) ;
#46662 = ORIENTED_EDGE ( 'NONE', *, *, #29830, .F. ) ;
#46663 = CARTESIAN_POINT ( 'NONE',  ( 1.441853549388196321, 3.346456692913386100, 1.535433070866133898 ) ) ;
#46664 = ORIENTED_EDGE ( 'NONE', *, *, #49482, .T. ) ;
#46665 = DIRECTION ( 'NONE',  ( 0.000000000000000000, -1.000000000000000000, 0.000000000000000000 ) ) ;
#46666 = CARTESIAN_POINT ( 'NONE',  ( -1.410501566226150194, 5.905511811023623991, 1.689247093817288325 ) ) ;
#46667 = CARTESIAN_POINT ( 'NONE',  ( -2.394586187573013003, 1.579445130333736458, 1.232696188189307929 ) ) ;
#46668 = ORIENTED_EDGE ( 'NONE', *, *, #22868, .T. ) ;
#46669 = VERTEX_POINT ( 'NONE', #23433 ) ;
#46670 = ADVANCED_FACE ( 'NONE', ( #4331 ), #14152, .T. ) ;
#46671 = DIRECTION ( 'NONE',  ( 1.734723475976806848E-16, -0.000000000000000000, 1.000000000000000000 ) ) ;
#46672 = CARTESIAN_POINT ( 'NONE',  ( 2.274988110810610031, 1.744340048923221920, -0.4687729985174870495 ) ) ;
#46673 = EDGE_CURVE ( 'NONE', #48909, #47245, #51002, .T. ) ;
#46674 = CARTESIAN_POINT ( 'NONE',  ( 1.599172890215260212, 5.905511811023623991, 1.460879300779193368 ) ) ;
#46675 = CARTESIAN_POINT ( 'NONE',  ( -0.5455278134075214336, 0.000000000000000000, -1.259842519685035134 ) ) ;
#46676 = EDGE_CURVE ( 'NONE', #37350, #2462, #20332, .T. ) ;
#46677 = DIRECTION ( 'NONE',  ( -3.469446951953613696E-16, 0.000000000000000000, -1.000000000000000000 ) ) ;
#46678 = PLANE ( 'NONE',  #39163 ) ;
#46679 = VECTOR ( 'NONE', #36572, 39.37007874015748143 ) ;
#46680 = DIRECTION ( 'NONE',  ( -0.000000000000000000, 0.000000000000000000, 1.000000000000000000 ) ) ;
#46681 = ORIENTED_EDGE ( 'NONE', *, *, #46327, .T. ) ;
#46682 = VECTOR ( 'NONE', #33262, 39.37007874015748143 ) ;
#46683 = FACE_OUTER_BOUND ( 'NONE', #44954, .T. ) ;
#46684 = VECTOR ( 'NONE', #864, 39.37007874015748143 ) ;
#46685 = ORIENTED_EDGE ( 'NONE', *, *, #43505, .T. ) ;
#46686 = VERTEX_POINT ( 'NONE', #43302 ) ;
#46687 = CARTESIAN_POINT ( 'NONE',  ( -1.794796351285541602, 3.267716535433071279, -1.102362204724405492 ) ) ;
#46688 = LINE ( 'NONE', #11358, #33614 ) ;
#46689 = EDGE_CURVE ( 'NONE', #29725, #9082, #15694, .T. ) ;
#46690 = VECTOR ( 'NONE', #18197, 39.37007874015748143 ) ;
#46691 = ORIENTED_EDGE ( 'NONE', *, *, #42157, .F. ) ;
#46692 = CIRCLE ( 'NONE', #34364, 2.106299212598425008 ) ;
#46693 = CARTESIAN_POINT ( 'NONE',  ( 0.7423782071083084855, 3.346456692913386100, -2.034117492951036166 ) ) ;
#46694 = EDGE_CURVE ( 'NONE', #19694, #35070, #195, .T. ) ;
#46695 = ORIENTED_EDGE ( 'NONE', *, *, #6385, .F. ) ;
#46696 = DIRECTION ( 'NONE',  ( 0.000000000000000000, 0.000000000000000000, 1.000000000000000000 ) ) ;
#46697 = ORIENTED_EDGE ( 'NONE', *, *, #2899, .T. ) ;
#46698 = DIRECTION ( 'NONE',  ( 1.734723475976806848E-16, -0.000000000000000000, 1.000000000000000000 ) ) ;
#46699 = CARTESIAN_POINT ( 'NONE',  ( -1.109524193798323788, 0.000000000000000000, 1.344750771968458380 ) ) ;
#46700 = ORIENTED_EDGE ( 'NONE', *, *, #21156, .T. ) ;
#46701 = CARTESIAN_POINT ( 'NONE',  ( -0.2727639067037607723, 0.000000000000000000, -1.417322834645664331 ) ) ;
#46702 = ORIENTED_EDGE ( 'NONE', *, *, #38464, .T. ) ;
#46703 = ORIENTED_EDGE ( 'NONE', *, *, #50115, .T. ) ;
#46704 = LINE ( 'NONE', #38748, #30109 ) ;
#46705 = FACE_OUTER_BOUND ( 'NONE', #14280, .T. ) ;
#46706 = CARTESIAN_POINT ( 'NONE',  ( -1.530693736245496872, 1.574803149606302854, -1.531579597454065800 ) ) ;
#46707 = ORIENTED_EDGE ( 'NONE', *, *, #46168, .F. ) ;
#46708 = CARTESIAN_POINT ( 'NONE',  ( -1.536664496436148184E-16, 3.346456692913386100, -0.8267716535433052849 ) ) ;
#46709 = DIRECTION ( 'NONE',  ( 0.000000000000000000, 1.160734090543304660E-16, -1.000000000000000000 ) ) ;
#46710 = CONICAL_SURFACE ( 'NONE', #20362, 3.483074324928249421, 1.244861948955335196 ) ;
#46711 = ORIENTED_EDGE ( 'NONE', *, *, #16053, .F. ) ;
#46712 = LINE ( 'NONE', #32033, #49623 ) ;
#46713 = AXIS2_PLACEMENT_3D ( 'NONE', #40180, #28287, #12813 ) ;
#46714 = ORIENTED_EDGE ( 'NONE', *, *, #46008, .T. ) ;
#46715 = ORIENTED_EDGE ( 'NONE', *, *, #35483, .F. ) ;
#46716 = B_SPLINE_CURVE_WITH_KNOTS ( 'NONE', 3,
 ( #49904, #49654, #2712, #17955 ),
 .UNSPECIFIED., .F., .F.,
 ( 4, 4 ),
 ( 2.656981594551095277E-07, 0.002500557877147534767 ),
 .UNSPECIFIED. ) ;
#46717 = DIRECTION ( 'NONE',  ( 0.5556468313118545499, 0.5997658974820547773, -0.5757929029352836237 ) ) ;
#46718 = EDGE_LOOP ( 'NONE', ( #44144, #36143, #25672, #5863 ) ) ;
#46719 = LINE ( 'NONE', #3898, #50612 ) ;
#46720 = CARTESIAN_POINT ( 'NONE',  ( -1.408960544533061299, 0.005352583808700523381, 1.060663264281380025 ) ) ;
#46721 = DIRECTION ( 'NONE',  ( 0.000000000000000000, -1.000000000000000000, 0.000000000000000000 ) ) ;
#46722 = DIRECTION ( 'NONE',  ( 5.063291518728965670E-17, 1.000000000000000000, 1.184615939703122503E-16 ) ) ;
#46723 = ORIENTED_EDGE ( 'NONE', *, *, #13070, .F. ) ;
#46724 = ORIENTED_EDGE ( 'NONE', *, *, #19647, .T. ) ;
#46725 = EDGE_CURVE ( 'NONE', #12822, #26233, #23694, .T. ) ;
#46726 = DIRECTION ( 'NONE',  ( 1.000000000000000000, 0.000000000000000000, -3.469446951953613696E-16 ) ) ;
#46727 = EDGE_CURVE ( 'NONE', #23227, #39081, #27327, .T. ) ;
#46728 = CARTESIAN_POINT ( 'NONE',  ( 0.08139965876239094178, 1.610780518492231694, 0.000000000000000000 ) ) ;
#46729 = VECTOR ( 'NONE', #30713, 39.37007874015748143 ) ;
#46730 = ORIENTED_EDGE ( 'NONE', *, *, #27044, .F. ) ;
#46731 = DIRECTION ( 'NONE',  ( -3.469446951953613696E-16, 0.000000000000000000, -1.000000000000000000 ) ) ;
#46732 = LINE ( 'NONE', #22774, #39161 ) ;
#46733 = EDGE_CURVE ( 'NONE', #39685, #23170, #20847, .T. ) ;
#46734 = ADVANCED_FACE ( 'NONE', ( #44577 ), #9487, .F. ) ;
#46735 = DIRECTION ( 'NONE',  ( 1.000000000000000000, 0.000000000000000000, 0.000000000000000000 ) ) ;
#46736 = DIRECTION ( 'NONE',  ( -0.7071067811865466846, -0.000000000000000000, -0.7071067811865483499 ) ) ;
#46737 = DIRECTION ( 'NONE',  ( 1.734723475976806848E-16, -0.000000000000000000, 1.000000000000000000 ) ) ;
#46738 = EDGE_LOOP ( 'NONE', ( #9547, #40479, #44714, #2391, #45898, #16873 ) ) ;
#46739 = DIRECTION ( 'NONE',  ( 1.000000000000000000, 0.000000000000000000, 0.000000000000000000 ) ) ;
#46740 = DIRECTION ( 'NONE',  ( 0.7818314824680309139, 7.233942271706491519E-17, -0.6234898018587318180 ) ) ;
#46741 = ORIENTED_EDGE ( 'NONE', *, *, #40733, .T. ) ;
#46742 = CARTESIAN_POINT ( 'NONE',  ( -2.043634885149970160, 1.574803149606302854, 0.7157624142945940848 ) ) ;
#46743 = PLANE ( 'NONE',  #27832 ) ;
#46744 = EDGE_CURVE ( 'NONE', #21187, #20924, #20375, .T. ) ;
#46745 = DIRECTION ( 'NONE',  ( 0.000000000000000000, 0.000000000000000000, -1.000000000000000000 ) ) ;
#46746 = AXIS2_PLACEMENT_3D ( 'NONE', #14568, #11196, #7328 ) ;
#46747 = VERTEX_POINT ( 'NONE', #25479 ) ;
#46748 = VECTOR ( 'NONE', #27597, 39.37007874015748143 ) ;
#46749 = ADVANCED_FACE ( 'NONE', ( #4850 ), #5862, .F. ) ;
#46750 = ORIENTED_EDGE ( 'NONE', *, *, #39545, .F. ) ;
#46751 = CARTESIAN_POINT ( 'NONE',  ( -1.636583440222563635, 0.000000000000000000, -0.1968503937007879123 ) ) ;
#46752 = ORIENTED_EDGE ( 'NONE', *, *, #627, .T. ) ;
#46753 = DIRECTION ( 'NONE',  ( 1.734723475976806848E-16, -0.000000000000000000, 1.000000000000000000 ) ) ;
#46754 = VERTEX_POINT ( 'NONE', #24472 ) ;
#46755 = CARTESIAN_POINT ( 'NONE',  ( 1.951645782807981178, 0.03882318759419040033, -0.4959286063371406983 ) ) ;
#46756 = PLANE ( 'NONE',  #4939 ) ;
#46757 = CARTESIAN_POINT ( 'NONE',  ( -1.363819533518803473, 0.000000000000000000, -1.929133858267710000 ) ) ;
#46758 = EDGE_CURVE ( 'NONE', #44234, #40389, #10866, .T. ) ;
#46759 = ORIENTED_EDGE ( 'NONE', *, *, #8261, .F. ) ;
#46760 = VERTEX_POINT ( 'NONE', #717 ) ;
#46761 = ORIENTED_EDGE ( 'NONE', *, *, #39947, .F. ) ;
#46762 = DIRECTION ( 'NONE',  ( -1.118904554427325505E-16, -1.000000000000000000, 3.087980359898369198E-17 ) ) ;
#46763 = CARTESIAN_POINT ( 'NONE',  ( -0.2727639067037611054, 3.267716535433071279, -2.148105963102950877 ) ) ;
#46764 = VERTEX_POINT ( 'NONE', #36859 ) ;
#46765 = ORIENTED_EDGE ( 'NONE', *, *, #29490, .T. ) ;
#46766 = DIRECTION ( 'NONE',  ( 0.9909497617679331460, 0.000000000000000000, 0.1342332658176667026 ) ) ;
#46767 = PLANE ( 'NONE',  #28549 ) ;
#46768 = DIRECTION ( 'NONE',  ( 1.000000000000000000, 0.000000000000000000, 0.000000000000000000 ) ) ;
#46769 = AXIS2_PLACEMENT_3D ( 'NONE', #19519, #11777, #36051 ) ;
#46770 = EDGE_CURVE ( 'NONE', #27061, #7202, #48749, .T. ) ;
#46771 = ORIENTED_EDGE ( 'NONE', *, *, #47765, .F. ) ;
#46772 = EDGE_LOOP ( 'NONE', ( #29126, #43674, #48672, #25580 ) ) ;
#46773 = DIRECTION ( 'NONE',  ( -1.000000000000000000, -0.000000000000000000, -0.000000000000000000 ) ) ;
#46774 = CARTESIAN_POINT ( 'NONE',  ( -2.074049943651441019, 1.574803149606302854, 0.6221544894623937116 ) ) ;
#46775 = CARTESIAN_POINT ( 'NONE',  ( -0.5455278134075214336, 3.267716535433071279, -0.5118110236220467790 ) ) ;
#46776 = VERTEX_POINT ( 'NONE', #47916 ) ;
#46777 = DIRECTION ( 'NONE',  ( 0.000000000000000000, 0.000000000000000000, -1.000000000000000000 ) ) ;
#46778 = LINE ( 'NONE', #27690, #3798 ) ;
#46779 = EDGE_LOOP ( 'NONE', ( #38021, #27051, #40729, #23368 ) ) ;
#46780 = DIRECTION ( 'NONE',  ( -0.000000000000000000, 1.000000000000000000, -0.000000000000000000 ) ) ;
#46781 = ORIENTED_EDGE ( 'NONE', *, *, #32040, .F. ) ;
#46782 = ORIENTED_EDGE ( 'NONE', *, *, #25453, .T. ) ;
#46783 = LINE ( 'NONE', #11456, #42733 ) ;
#46784 = CARTESIAN_POINT ( 'NONE',  ( -1.985260859929297794, 3.267716535433071279, 6.887757239314512246E-16 ) ) ;
#46785 = CARTESIAN_POINT ( 'NONE',  ( -1.088998432874330735, 5.905511811023623991, 1.918626195649137500 ) ) ;
#46786 = AXIS2_PLACEMENT_3D ( 'NONE', #47577, #12250, #34988 ) ;
#46787 = CIRCLE ( 'NONE', #22111, 2.165354330708661568 ) ;
#46788 = DIRECTION ( 'NONE',  ( -0.9998717552508122886, -0.01601477604151181275, 0.000000000000000000 ) ) ;
#46789 = LINE ( 'NONE', #23325, #32107 ) ;
#46790 = VERTEX_POINT ( 'NONE', #29090 ) ;
#46791 = VERTEX_POINT ( 'NONE', #12589 ) ;
#46792 = CONICAL_SURFACE ( 'NONE', #21260, 1.850107469027523210, 0.6386652850508578450 ) ;
#46793 = ORIENTED_EDGE ( 'NONE', *, *, #42582, .T. ) ;
#46794 = DIRECTION ( 'NONE',  ( -0.000000000000000000, 1.000000000000000000, -0.000000000000000000 ) ) ;
#46795 = CARTESIAN_POINT ( 'NONE',  ( -1.439733046521777027, 0.000000000000000000, -0.5118110236220466680 ) ) ;
#46796 = EDGE_CURVE ( 'NONE', #23287, #2346, #25316, .T. ) ;
#46797 = AXIS2_PLACEMENT_3D ( 'NONE', #14798, #10917, #19158 ) ;
#46798 = EDGE_CURVE ( 'NONE', #13419, #41040, #44831, .T. ) ;
#46799 = EDGE_CURVE ( 'NONE', #36331, #31704, #21108, .T. ) ;
#46800 = CIRCLE ( 'NONE', #27034, 2.165354330708661568 ) ;
#46801 = DIRECTION ( 'NONE',  ( -1.156482317317871478E-16, 0.000000000000000000, -1.000000000000000000 ) ) ;
#46802 = CARTESIAN_POINT ( 'NONE',  ( -1.521361932310741016, 3.346456692913386100, -1.456692913385822186 ) ) ;
#46803 = CARTESIAN_POINT ( 'NONE',  ( 1.909347346926324684, 0.000000000000000000, 0.2755905511810994302 ) ) ;
#46804 = ORIENTED_EDGE ( 'NONE', *, *, #9901, .T. ) ;
#46805 = DIRECTION ( 'NONE',  ( -0.000000000000000000, 1.000000000000000000, -0.000000000000000000 ) ) ;
#46806 = VECTOR ( 'NONE', #26393, 39.37007874015748854 ) ;
#46807 = CARTESIAN_POINT ( 'NONE',  ( 1.560669927219590525, 3.346456692913386100, 0.2755905511810996522 ) ) ;
#46808 = ORIENTED_EDGE ( 'NONE', *, *, #49180, .F. ) ;
#46809 = DIRECTION ( 'NONE',  ( 1.734723475976806848E-16, -0.000000000000000000, 1.000000000000000000 ) ) ;
#46810 = LINE ( 'NONE', #11482, #14629 ) ;
#46811 = CARTESIAN_POINT ( 'NONE',  ( 2.919426793319799707, 0.000000000000000000, 0.4451252810446820196 ) ) ;
#46812 = CARTESIAN_POINT ( 'NONE',  ( -1.915856643696823625, 1.586962021640019538, -1.899833043120999099 ) ) ;
#46813 = FACE_OUTER_BOUND ( 'NONE', #32293, .T. ) ;
#46814 = CARTESIAN_POINT ( 'NONE',  ( 0.7423782071083092626, 0.000000000000000000, 1.259842519685033357 ) ) ;
#46815 = ORIENTED_EDGE ( 'NONE', *, *, #7421, .F. ) ;
#46816 = DIRECTION ( 'NONE',  ( 2.866708903754509961E-17, 1.000000000000000000, -1.255987235303920130E-16 ) ) ;
#46817 = ORIENTED_EDGE ( 'NONE', *, *, #19083, .F. ) ;
#46818 = CARTESIAN_POINT ( 'NONE',  ( 2.949782676795221992, 0.000000000000000000, -0.1324748927672375898 ) ) ;
#46819 = CARTESIAN_POINT ( 'NONE',  ( -1.909347346926324906, 3.346456692913386100, -1.299212598425193210 ) ) ;
#46820 = DIRECTION ( 'NONE',  ( -3.469446951953613696E-16, 0.000000000000000000, -1.000000000000000000 ) ) ;
#46821 = AXIS2_PLACEMENT_3D ( 'NONE', #17530, #49486, #2293 ) ;
#46822 = EDGE_CURVE ( 'NONE', #5168, #28186, #9227, .T. ) ;
#46823 = EDGE_LOOP ( 'NONE', ( #19797, #35847, #8639, #13493 ) ) ;
#46824 = ORIENTED_EDGE ( 'NONE', *, *, #9620, .F. ) ;
#46825 = DIRECTION ( 'NONE',  ( -1.000000000000000000, -0.000000000000000000, -0.000000000000000000 ) ) ;
#46826 = DIRECTION ( 'NONE',  ( 0.000000000000000000, -1.000000000000000000, 0.000000000000000000 ) ) ;
#46827 = CARTESIAN_POINT ( 'NONE',  ( 1.560669927219590303, 3.346456692913386100, -1.417322834645665219 ) ) ;
#46828 = VECTOR ( 'NONE', #31847, 39.37007874015748143 ) ;
#46829 = DIRECTION ( 'NONE',  ( 1.000000000000000000, 0.000000000000000000, 0.000000000000000000 ) ) ;
#46830 = LINE ( 'NONE', #35757, #45031 ) ;
#46831 = EDGE_CURVE ( 'NONE', #49170, #12597, #25232, .T. ) ;
#46832 = DIRECTION ( 'NONE',  ( 1.734723475976806848E-16, 0.000000000000000000, 1.000000000000000000 ) ) ;
#46833 = VECTOR ( 'NONE', #43036, 39.37007874015748143 ) ;
#46834 = VERTEX_POINT ( 'NONE', #17486 ) ;
#46835 = CARTESIAN_POINT ( 'NONE',  ( -0.7381027496704858359, 1.609316782724114825, -2.859439394060923512 ) ) ;
#46836 = CARTESIAN_POINT ( 'NONE',  ( 0.1071992566810385378, 0.000000000000000000, -1.740088185897661788 ) ) ;
#46837 = ADVANCED_FACE ( 'NONE', ( #32998 ), #48677, .F. ) ;
#46838 = VECTOR ( 'NONE', #980, 39.37007874015748143 ) ;
#46839 = DIRECTION ( 'NONE',  ( 1.734723475976806848E-16, -0.000000000000000000, 1.000000000000000000 ) ) ;
#46840 = VERTEX_POINT ( 'NONE', #28585 ) ;
#46841 = EDGE_CURVE ( 'NONE', #19826, #33327, #40477, .T. ) ;
#46842 = CARTESIAN_POINT ( 'NONE',  ( 1.636583440222563635, 3.267716535433071279, -1.325930245594399537 ) ) ;
#46843 = ORIENTED_EDGE ( 'NONE', *, *, #18618, .F. ) ;
#46844 = ORIENTED_EDGE ( 'NONE', *, *, #29697, .T. ) ;
#46845 = VECTOR ( 'NONE', #25450, 39.37007874015748143 ) ;
#46846 = DIRECTION ( 'NONE',  ( -0.000000000000000000, 0.000000000000000000, 1.000000000000000000 ) ) ;
#46847 = ADVANCED_FACE ( 'NONE', ( #37115 ), #5099, .F. ) ;
#46848 = VECTOR ( 'NONE', #27580, 39.37007874015748143 ) ;
#46849 = ORIENTED_EDGE ( 'NONE', *, *, #14401, .F. ) ;
#46850 = ORIENTED_EDGE ( 'NONE', *, *, #38272, .F. ) ;
#46851 = CARTESIAN_POINT ( 'NONE',  ( -1.363819533518803473, 3.267716535433071279, -0.4724409448818886470 ) ) ;
#46852 = VERTEX_POINT ( 'NONE', #6378 ) ;
#46853 = DIRECTION ( 'NONE',  ( -3.469446951953613696E-16, 0.000000000000000000, -1.000000000000000000 ) ) ;
#46854 = LINE ( 'NONE', #35276, #1317 ) ;
#46855 = PLANE ( 'NONE',  #6927 ) ;
#46856 = EDGE_CURVE ( 'NONE', #32877, #19533, #30380, .T. ) ;
#46857 = LINE ( 'NONE', #14645, #4149 ) ;
#46858 = EDGE_CURVE ( 'NONE', #43954, #37379, #30630, .T. ) ;
#46859 = EDGE_CURVE ( 'NONE', #26933, #36182, #1991, .T. ) ;
#46860 = LINE ( 'NONE', #11528, #16272 ) ;
#46861 = CARTESIAN_POINT ( 'NONE',  ( 1.560669927219591413, 3.267716535433071279, 1.732283464566921172 ) ) ;
#46862 = ORIENTED_EDGE ( 'NONE', *, *, #45173, .T. ) ;
#46863 = CARTESIAN_POINT ( 'NONE',  ( -2.162130742952123263, 3.346456692913386100, 0.1181102362204704270 ) ) ;
#46864 = CARTESIAN_POINT ( 'NONE',  ( -1.936750629140493007, 1.578456148182591168, 0.9863243683714766341 ) ) ;
#46865 = DIRECTION ( 'NONE',  ( -0.000000000000000000, 1.000000000000000000, -0.000000000000000000 ) ) ;
#46866 = DIRECTION ( 'NONE',  ( -0.000000000000000000, 0.000000000000000000, 1.000000000000000000 ) ) ;
#46867 = VECTOR ( 'NONE', #6522, 39.37007874015748143 ) ;
#46868 = ORIENTED_EDGE ( 'NONE', *, *, #12108, .F. ) ;
#46869 = DIRECTION ( 'NONE',  ( 0.000000000000000000, 1.000000000000000000, -0.000000000000000000 ) ) ;
#46870 = CARTESIAN_POINT ( 'NONE',  ( 1.560669927219590747, 3.346456692913386100, 1.102362204724403938 ) ) ;
#46871 = EDGE_LOOP ( 'NONE', ( #39113, #6930, #14876, #31604 ) ) ;
#46872 = DIRECTION ( 'NONE',  ( -0.000000000000000000, -1.000000000000000000, -0.000000000000000000 ) ) ;
#46873 = DIRECTION ( 'NONE',  ( 8.741157232058247392E-17, -1.000000000000000000, -7.636919086868415696E-17 ) ) ;
#46874 = ORIENTED_EDGE ( 'NONE', *, *, #29670, .T. ) ;
#46875 = DIRECTION ( 'NONE',  ( -1.000000000000000000, 0.000000000000000000, 0.000000000000000000 ) ) ;
#46876 = CARTESIAN_POINT ( 'NONE',  ( 1.228106025299609216, 1.734763879243638396, -2.436764970734814906 ) ) ;
#46877 = CARTESIAN_POINT ( 'NONE',  ( 0.5455278134075208785, 3.346456692913386100, -2.034427629037600660 ) ) ;
#46878 = CARTESIAN_POINT ( 'NONE',  ( 2.182111253630085290, 3.267716535433071279, -3.785359618865289765E-16 ) ) ;
#46879 = ORIENTED_EDGE ( 'NONE', *, *, #39250, .T. ) ;
#46880 = ADVANCED_FACE ( 'NONE', ( #2508 ), #37624, .T. ) ;
#46881 = ORIENTED_EDGE ( 'NONE', *, *, #10895, .T. ) ;
#46882 = ORIENTED_EDGE ( 'NONE', *, *, #462, .F. ) ;
#46883 = FACE_OUTER_BOUND ( 'NONE', #12271, .T. ) ;
#46884 = ORIENTED_EDGE ( 'NONE', *, *, #390, .F. ) ;
#46885 = LINE ( 'NONE', #3814, #46833 ) ;
#46886 = CARTESIAN_POINT ( 'NONE',  ( -2.411201994581868568, 1.049302529728235234, 0.8351922078364127922 ) ) ;
#46887 = ORIENTED_EDGE ( 'NONE', *, *, #24287, .F. ) ;
#46888 = EDGE_CURVE ( 'NONE', #25127, #2869, #11008, .T. ) ;
#46889 = CARTESIAN_POINT ( 'NONE',  ( 2.100403847690402337, 3.346456692913386100, 0.1574803149606280872 ) ) ;
#46890 = EDGE_CURVE ( 'NONE', #30424, #42646, #45840, .T. ) ;
#46891 = VECTOR ( 'NONE', #20448, 39.37007874015748143 ) ;
#46892 = ORIENTED_EDGE ( 'NONE', *, *, #20236, .F. ) ;
#46893 = DIRECTION ( 'NONE',  ( 1.000000000000000000, 0.000000000000000000, 0.000000000000000000 ) ) ;
#46894 = EDGE_CURVE ( 'NONE', #23660, #49387, #27131, .T. ) ;
#46895 = EDGE_LOOP ( 'NONE', ( #30908, #40075, #3153, #45147 ) ) ;
#46896 = ORIENTED_EDGE ( 'NONE', *, *, #11352, .F. ) ;
#46897 = DIRECTION ( 'NONE',  ( -0.000000000000000000, 1.000000000000000000, -0.000000000000000000 ) ) ;
#46898 = ORIENTED_EDGE ( 'NONE', *, *, #38319, .T. ) ;
#46899 = VECTOR ( 'NONE', #17917, 39.37007874015748143 ) ;
#46900 = LINE ( 'NONE', #11573, #50850 ) ;
#46901 = EDGE_LOOP ( 'NONE', ( #49590, #1861, #36410, #27440 ) ) ;
#46902 = VERTEX_POINT ( 'NONE', #10752 ) ;
#46903 = ADVANCED_FACE ( 'NONE', ( #6631 ), #9994, .F. ) ;
#46904 = AXIS2_PLACEMENT_3D ( 'NONE', #13337, #33225, #17718 ) ;
#46905 = CARTESIAN_POINT ( 'NONE',  ( -0.9794755770252102645, 0.5070346321433213399, -1.025452293874513643 ) ) ;
#46906 = CARTESIAN_POINT ( 'NONE',  ( 0.9948011493083114276, 0.4042499682059490507, -1.112911385528784658 ) ) ;
#46907 = ORIENTED_EDGE ( 'NONE', *, *, #39204, .T. ) ;
#46908 = EDGE_CURVE ( 'NONE', #10269, #7688, #26246, .T. ) ;
#46909 = VECTOR ( 'NONE', #47579, 39.37007874015748143 ) ;
#46910 = CARTESIAN_POINT ( 'NONE',  ( 2.106197740627111958, 3.267716535433071279, -0.6692913385826764205 ) ) ;
#46911 = ORIENTED_EDGE ( 'NONE', *, *, #11858, .T. ) ;
#46912 = DIRECTION ( 'NONE',  ( 1.000000000000000000, -0.000000000000000000, 0.000000000000000000 ) ) ;
#46913 = DIRECTION ( 'NONE',  ( -0.000000000000000000, 1.000000000000000000, -0.000000000000000000 ) ) ;
#46915 = EDGE_CURVE ( 'NONE', #11581, #36186, #37884, .T. ) ;
#46914 = LINE ( 'NONE', #11584, #26376 ) ;
#46916 = EDGE_CURVE ( 'NONE', #33610, #45880, #17740, .T. ) ;
#46917 = VERTEX_POINT ( 'NONE', #18505 ) ;
#46918 = ORIENTED_EDGE ( 'NONE', *, *, #5325, .F. ) ;
#46919 = CARTESIAN_POINT ( 'NONE',  ( 0.2727639067037610499, 3.346456692913386100, 2.362204724409437961 ) ) ;
#46920 = CARTESIAN_POINT ( 'NONE',  ( 0.000000000000000000, 3.267716535433071279, 1.259842519685033357 ) ) ;
#46921 = EDGE_CURVE ( 'NONE', #30631, #48480, #33762, .T. ) ;
#46922 = CARTESIAN_POINT ( 'NONE',  ( -1.738757879605812073, 7.027592017269983715E-05, -0.1273499085982673085 ) ) ;
#46923 = CARTESIAN_POINT ( 'NONE',  ( -0.2727639067037608278, 3.346456692913386100, -1.614173228346451605 ) ) ;
#46924 = DIRECTION ( 'NONE',  ( 1.000000000000000000, 0.000000000000000000, -3.469446951953613696E-16 ) ) ;
#46925 = CARTESIAN_POINT ( 'NONE',  ( -0.2810210260108632063, 1.714875720633193934, -2.939398529262501558 ) ) ;
#46926 = AXIS2_PLACEMENT_3D ( 'NONE', #29475, #13983, #8258 ) ;
#46927 = VERTEX_POINT ( 'NONE', #41996 ) ;
#46928 = CARTESIAN_POINT ( 'NONE',  ( 0.7423782071083087075, 3.267716535433071279, -0.3149606299212593941 ) ) ;
#46929 = ORIENTED_EDGE ( 'NONE', *, *, #17766, .T. ) ;
#46930 = DIRECTION ( 'NONE',  ( 1.734723475976806848E-16, -0.000000000000000000, 1.000000000000000000 ) ) ;
#46931 = ORIENTED_EDGE ( 'NONE', *, *, #35558, .F. ) ;
#46932 = VERTEX_POINT ( 'NONE', #2751 ) ;
#46933 = CARTESIAN_POINT ( 'NONE',  ( -1.536664496436148184E-16, 3.346456692913386100, 0.1181102362204701633 ) ) ;
#46934 = VECTOR ( 'NONE', #36422, 39.37007874015748854 ) ;
#46935 = DIRECTION ( 'NONE',  ( -0.000000000000000000, 1.000000000000000000, -0.000000000000000000 ) ) ;
#46936 = ORIENTED_EDGE ( 'NONE', *, *, #33978, .F. ) ;
#46937 = DIRECTION ( 'NONE',  ( 0.000000000000000000, 0.000000000000000000, -1.000000000000000000 ) ) ;
#46938 = EDGE_LOOP ( 'NONE', ( #5745, #37713, #30482, #45035, #30381, #12463, #39890, #29500, #14648, #25979, #10039 ) ) ;
#46939 = CARTESIAN_POINT ( 'NONE',  ( -1.363819533518803029, 0.000000000000000000, 0.9055118110236167750 ) ) ;
#46940 = AXIS2_PLACEMENT_3D ( 'NONE', #2670, #23049, #18419 ) ;
#46941 = VERTEX_POINT ( 'NONE', #49692 ) ;
#46942 = CARTESIAN_POINT ( 'NONE',  ( 0.08139965876239094178, 1.610780518492231694, 0.000000000000000000 ) ) ;
#46943 = LINE ( 'NONE', #39494, #11571 ) ;
#46944 = ADVANCED_FACE ( 'NONE', ( #30124 ), #6781, .T. ) ;
#46945 = ORIENTED_EDGE ( 'NONE', *, *, #35014, .F. ) ;
#46946 = EDGE_CURVE ( 'NONE', #35716, #42223, #6879, .T. ) ;
#46947 = FACE_OUTER_BOUND ( 'NONE', #39011, .T. ) ;
#46948 = ORIENTED_EDGE ( 'NONE', *, *, #22719, .F. ) ;
#46949 = EDGE_LOOP ( 'NONE', ( #36039, #26027, #12086, #14259 ) ) ;
#46950 = CARTESIAN_POINT ( 'NONE',  ( -2.122900408388392002, 1.686164691611804489, -2.052396256679426489 ) ) ;
#46951 = DIRECTION ( 'NONE',  ( -0.7071067811865483499, -0.000000000000000000, 0.7071067811865466846 ) ) ;
#46952 = DIRECTION ( 'NONE',  ( 0.000000000000000000, 1.000000000000000000, 0.000000000000000000 ) ) ;
#46953 = VERTEX_POINT ( 'NONE', #22626 ) ;
#46954 = DIRECTION ( 'NONE',  ( -3.469446951953613696E-16, 0.000000000000000000, -1.000000000000000000 ) ) ;
#46955 = CARTESIAN_POINT ( 'NONE',  ( -1.556712866041156440, 1.694999912340861004, 2.509548638715847435 ) ) ;
#46956 = ORIENTED_EDGE ( 'NONE', *, *, #1036, .T. ) ;
#46957 = CARTESIAN_POINT ( 'NONE',  ( -0.6214413264104942103, 3.267716535433071279, 2.156057715732900040E-16 ) ) ;
#46958 = ORIENTED_EDGE ( 'NONE', *, *, #2955, .T. ) ;
#46959 = ORIENTED_EDGE ( 'NONE', *, *, #5854, .T. ) ;
#46960 = EDGE_CURVE ( 'NONE', #16522, #32449, #33391, .T. ) ;
#46961 = SHAPE_REPRESENTATION_RELATIONSHIP ( 'NONE' , 'NONE' ,  #5020, #37253 ) ;
#46962 = VERTEX_POINT ( 'NONE', #33505 ) ;
#46963 = DIRECTION ( 'NONE',  ( 0.000000000000000000, 0.000000000000000000, 1.000000000000000000 ) ) ;
#46964 = DIRECTION ( 'NONE',  ( 1.734723475976806848E-16, -0.000000000000000000, 1.000000000000000000 ) ) ;
#46965 = EDGE_CURVE ( 'NONE', #41036, #26643, #13872, .T. ) ;
#46966 = VECTOR ( 'NONE', #19944, 39.37007874015748143 ) ;
#46967 = LINE ( 'NONE', #791, #50562 ) ;
#46968 = CARTESIAN_POINT ( 'NONE',  ( -1.712496953225537633, 3.346456692913386100, -1.102362204724405492 ) ) ;
#46969 = ORIENTED_EDGE ( 'NONE', *, *, #24999, .T. ) ;
#46970 = VERTEX_POINT ( 'NONE', #46842 ) ;
#46971 = DIRECTION ( 'NONE',  ( -3.469446951953613696E-16, 0.000000000000000000, -1.000000000000000000 ) ) ;
#46972 = EDGE_CURVE ( 'NONE', #50795, #48962, #23373, .T. ) ;
#46973 = CARTESIAN_POINT ( 'NONE',  ( -1.025452293874513199, 0.4610579152940180170, 1.025452293874513199 ) ) ;
#46974 = VECTOR ( 'NONE', #27604, 39.37007874015748143 ) ;
#46975 = ORIENTED_EDGE ( 'NONE', *, *, #45169, .T. ) ;
#46976 = EDGE_CURVE ( 'NONE', #2834, #46309, #9868, .T. ) ;
#46977 = DIRECTION ( 'NONE',  ( -0.000000000000000000, 1.000000000000000000, -0.000000000000000000 ) ) ;
#46978 = DIRECTION ( 'NONE',  ( -0.000000000000000000, 1.000000000000000000, -0.000000000000000000 ) ) ;
#46979 = PLANE ( 'NONE',  #15987 ) ;
#46980 = CARTESIAN_POINT ( 'NONE',  ( 1.091055626815042423, 3.267716535433071279, -1.574803149606294417 ) ) ;
#46981 = DIRECTION ( 'NONE',  ( -0.000000000000000000, 1.000000000000000000, -0.000000000000000000 ) ) ;
#46982 = ORIENTED_EDGE ( 'NONE', *, *, #24846, .F. ) ;
#46983 = LINE ( 'NONE', #19895, #21757 ) ;
#46984 = DIRECTION ( 'NONE',  ( -0.01601477604151182663, 0.9998717552508123996, -0.000000000000000000 ) ) ;
#46985 = VERTEX_POINT ( 'NONE', #8154 ) ;
#46986 = VERTEX_POINT ( 'NONE', #23895 ) ;
#46987 = CARTESIAN_POINT ( 'NONE',  ( 2.043634885149959501, 1.574803149606302854, 0.7157624142946232837 ) ) ;
#46988 = LINE ( 'NONE', #7041, #41822 ) ;
#46989 = DIRECTION ( 'NONE',  ( -0.000000000000000000, 1.000000000000000000, -0.000000000000000000 ) ) ;
#46990 = EDGE_LOOP ( 'NONE', ( #16994, #18072, #21369, #48629 ) ) ;
#46991 = EDGE_LOOP ( 'NONE', ( #4178, #4624, #43372, #18893 ) ) ;
#46992 = PLANE ( 'NONE',  #30373 ) ;
#46993 = VERTEX_POINT ( 'NONE', #7639 ) ;
#46994 = CARTESIAN_POINT ( 'NONE',  ( 1.558105373646060388, 3.346456692913386100, 1.417322834645662777 ) ) ;
#46995 = ORIENTED_EDGE ( 'NONE', *, *, #443, .T. ) ;
#46996 = VECTOR ( 'NONE', #26, 39.37007874015748143 ) ;
#46997 = PLANE ( 'NONE',  #49038 ) ;
#46998 = PLANE ( 'NONE',  #13206 ) ;
#46999 = PLANE ( 'NONE',  #29341 ) ;
#47000 = VECTOR ( 'NONE', #7673, 39.37007874015748143 ) ;
#47001 = ORIENTED_EDGE ( 'NONE', *, *, #21983, .F. ) ;
#47002 = EDGE_CURVE ( 'NONE', #23113, #15497, #39131, .T. ) ;
#47003 = ORIENTED_EDGE ( 'NONE', *, *, #33865, .F. ) ;
#47004 = VERTEX_POINT ( 'NONE', #28018 ) ;
#47005 = LINE ( 'NONE', #43161, #21598 ) ;
#47006 = PLANE ( 'NONE',  #44457 ) ;
#47007 = EDGE_CURVE ( 'NONE', #47418, #15669, #27758, .T. ) ;
#47008 = VERTEX_POINT ( 'NONE', #43499 ) ;
#47009 = EDGE_LOOP ( 'NONE', ( #35489, #42342, #4660, #18074 ) ) ;
#47010 = FACE_OUTER_BOUND ( 'NONE', #34577, .T. ) ;
#47011 = LINE ( 'NONE', #46522, #25243 ) ;
#47012 = AXIS2_PLACEMENT_3D ( 'NONE', #11563, #19802, #4080 ) ;
#47013 = DIRECTION ( 'NONE',  ( 0.000000000000000000, 0.000000000000000000, 1.000000000000000000 ) ) ;
#47014 = EDGE_CURVE ( 'NONE', #7604, #47727, #4273, .T. ) ;
#47015 = EDGE_LOOP ( 'NONE', ( #36036, #8576, #4238, #45885 ) ) ;
#47016 = ORIENTED_EDGE ( 'NONE', *, *, #44605, .F. ) ;
#47017 = LINE ( 'NONE', #18940, #30444 ) ;
#47018 = DIRECTION ( 'NONE',  ( 0.000000000000000000, 0.000000000000000000, 1.000000000000000000 ) ) ;
#47019 = DIRECTION ( 'NONE',  ( 0.000000000000000000, 0.000000000000000000, 1.000000000000000000 ) ) ;
#47020 = EDGE_CURVE ( 'NONE', #18896, #14924, #2468, .T. ) ;
#47021 = ORIENTED_EDGE ( 'NONE', *, *, #1922, .F. ) ;
#47022 = CARTESIAN_POINT ( 'NONE',  ( -2.362204724409447731, 1.172985819482486924, -4.133858267716536083 ) ) ;
#47023 = FACE_OUTER_BOUND ( 'NONE', #34801, .T. ) ;
#47024 = ORIENTED_EDGE ( 'NONE', *, *, #40607, .F. ) ;
#47025 = B_SPLINE_CURVE_WITH_KNOTS ( 'NONE', 3,
 ( #44531, #37066, #17946, #1685 ),
 .UNSPECIFIED., .F., .F.,
 ( 4, 4 ),
 ( 2.767205287773147393E-07, 0.002500421603420419601 ),
 .UNSPECIFIED. ) ;
#47026 = CARTESIAN_POINT ( 'NONE',  ( 1.636583440222563857, 3.267716535433071279, 0.4330708661417290162 ) ) ;
#47027 = ORIENTED_EDGE ( 'NONE', *, *, #26886, .F. ) ;
#47028 = VERTEX_POINT ( 'NONE', #3258 ) ;
#47029 = DIRECTION ( 'NONE',  ( 0.000000000000000000, -1.000000000000000000, 0.000000000000000000 ) ) ;
#47030 = LINE ( 'NONE', #14580, #4440 ) ;
#47031 = PLANE ( 'NONE',  #40439 ) ;
#47032 = EDGE_CURVE ( 'NONE', #34103, #36731, #42504, .T. ) ;
#47033 = LINE ( 'NONE', #7836, #41797 ) ;
#47034 = DIRECTION ( 'NONE',  ( -0.000000000000000000, 1.000000000000000000, -0.000000000000000000 ) ) ;
#47035 = ORIENTED_EDGE ( 'NONE', *, *, #1440, .T. ) ;
#47036 = ORIENTED_EDGE ( 'NONE', *, *, #18043, .T. ) ;
#47037 = EDGE_CURVE ( 'NONE', #22325, #42444, #31644, .T. ) ;
#47038 = ORIENTED_EDGE ( 'NONE', *, *, #37437, .T. ) ;
#47039 = DIRECTION ( 'NONE',  ( 1.000000000000000000, 0.000000000000000000, 0.000000000000000000 ) ) ;
#47040 = FACE_OUTER_BOUND ( 'NONE', #34373, .T. ) ;
#47041 = CIRCLE ( 'NONE', #49512, 2.246510896728926010 ) ;
#47042 = VECTOR ( 'NONE', #29088, 39.37007874015748143 ) ;
#47043 = CARTESIAN_POINT ( 'NONE',  ( 0.000000000000000000, 3.267716535433071279, -6.146657985744592735E-16 ) ) ;
#47044 = CARTESIAN_POINT ( 'NONE',  ( 2.061875708210571201, 1.740926663775191674, 1.053657044629532802 ) ) ;
#47045 = ORIENTED_EDGE ( 'NONE', *, *, #41357, .F. ) ;
#47046 = LINE ( 'NONE', #6601, #6056 ) ;
#47047 = CIRCLE ( 'NONE', #41355, 2.106299212598425008 ) ;
#47048 = EDGE_CURVE ( 'NONE', #5596, #13971, #12280, .T. ) ;
#47049 = CARTESIAN_POINT ( 'NONE',  ( -0.5455278134075214336, 3.346456692913386100, -0.8267716535433049518 ) ) ;
#47050 = ORIENTED_EDGE ( 'NONE', *, *, #13430, .F. ) ;
#47051 = VECTOR ( 'NONE', #36570, 39.37007874015748143 ) ;
#47052 = CARTESIAN_POINT ( 'NONE',  ( 0.7423782071083092626, 3.346456692913386100, 1.259842519685033357 ) ) ;
#47053 = CARTESIAN_POINT ( 'NONE',  ( -1.181102362204724310, 0.4724409448818890911, -1.181102362204724754 ) ) ;
#47054 = DIRECTION ( 'NONE',  ( 1.734723475976806848E-16, -0.000000000000000000, 1.000000000000000000 ) ) ;
#47055 = ORIENTED_EDGE ( 'NONE', *, *, #33689, .T. ) ;
#47056 = CARTESIAN_POINT ( 'NONE',  ( -0.07591351300297333182, 3.267716535433071279, -1.417322834645664331 ) ) ;
#47057 = DIRECTION ( 'NONE',  ( -1.000000000000000000, 0.000000000000000000, 1.734723475976806848E-16 ) ) ;
#47058 = LINE ( 'NONE', #35736, #48931 ) ;
#47059 = ORIENTED_EDGE ( 'NONE', *, *, #15377, .F. ) ;
#47060 = DIRECTION ( 'NONE',  ( -1.000000000000000000, 0.000000000000000000, -0.000000000000000000 ) ) ;
#47061 = VERTEX_POINT ( 'NONE', #15131 ) ;
#47062 = PLANE ( 'NONE',  #46786 ) ;
#47063 = B_SPLINE_CURVE_WITH_KNOTS ( 'NONE', 3,
 ( #11294, #15917, #27277, #19784 ),
 .UNSPECIFIED., .F., .F.,
 ( 4, 4 ),
 ( 0.0004412629834327503188, 0.04923299811573771112 ),
 .UNSPECIFIED. ) ;
#47064 = DIRECTION ( 'NONE',  ( 0.9998717552508121775, 0.01601477604151182663, 0.000000000000000000 ) ) ;
#47065 = LINE ( 'NONE', #34490, #18590 ) ;
#47066 = ORIENTED_EDGE ( 'NONE', *, *, #7215, .T. ) ;
#47067 = ORIENTED_EDGE ( 'NONE', *, *, #29643, .F. ) ;
#47068 = CARTESIAN_POINT ( 'NONE',  ( -1.363819533518803251, 3.267716535433071279, 2.365849761790805487E-16 ) ) ;
#47069 = CARTESIAN_POINT ( 'NONE',  ( 0.3136974817028393425, 1.625700591256411531, -2.936457595020219635 ) ) ;
#47070 = EDGE_CURVE ( 'NONE', #15612, #38883, #35515, .T. ) ;
#47071 = ORIENTED_EDGE ( 'NONE', *, *, #17303, .F. ) ;
#47072 = CARTESIAN_POINT ( 'NONE',  ( 1.015142113812069313, 0.000000000000000000, -0.4724409448818889246 ) ) ;
#47073 = CARTESIAN_POINT ( 'NONE',  ( 1.091055626815042645, 0.000000000000000000, 0.6299212598425161236 ) ) ;
#47074 = DIRECTION ( 'NONE',  ( -1.000000000000000000, 0.000000000000000000, -0.000000000000000000 ) ) ;
#47075 = B_SPLINE_CURVE_WITH_KNOTS ( 'NONE', 3,
 ( #9762, #14136, #2773, #41010 ),
 .UNSPECIFIED., .F., .F.,
 ( 4, 4 ),
 ( 0.0004868636330354340533, 0.002987072310269779825 ),
 .UNSPECIFIED. ) ;
#47076 = ADVANCED_FACE ( 'NONE', ( #7139 ), #22882, .F. ) ;
#47077 = AXIS2_PLACEMENT_3D ( 'NONE', #3032, #7164, #15662 ) ;
#47078 = LINE ( 'NONE', #9418, #49490 ) ;
#47079 = VECTOR ( 'NONE', #12277, 39.37007874015748143 ) ;
#47080 = ORIENTED_EDGE ( 'NONE', *, *, #46673, .F. ) ;
#47081 = ADVANCED_FACE ( 'NONE', ( #38880 ), #44680, .T. ) ;
#47082 = ORIENTED_EDGE ( 'NONE', *, *, #17127, .F. ) ;
#47083 = DIRECTION ( 'NONE',  ( 3.586865599282426309E-17, -1.000000000000000000, -1.103923720497134591E-16 ) ) ;
#47084 = EDGE_CURVE ( 'NONE', #27696, #3507, #49232, .T. ) ;
#47085 = DIRECTION ( 'NONE',  ( -0.000000000000000000, 1.000000000000000000, -0.000000000000000000 ) ) ;
#47086 = VECTOR ( 'NONE', #39881, 39.37007874015748143 ) ;
#47087 = ORIENTED_EDGE ( 'NONE', *, *, #39086, .F. ) ;
#47088 = DIRECTION ( 'NONE',  ( -3.469446951953613696E-16, 0.000000000000000000, -1.000000000000000000 ) ) ;
#47089 = ORIENTED_EDGE ( 'NONE', *, *, #46196, .T. ) ;
#47090 = VECTOR ( 'NONE', #13675, 39.37007874015748143 ) ;
#47091 = VERTEX_POINT ( 'NONE', #15388 ) ;
#47092 = DIRECTION ( 'NONE',  ( -0.01601477604151182663, 0.9998717552508123996, -0.000000000000000000 ) ) ;
#47093 = CONICAL_SURFACE ( 'NONE', #28996, 2.165354330708661568, 0.2617993877991570129 ) ;
#47094 = EDGE_CURVE ( 'NONE', #43110, #41248, #19000, .T. ) ;
#47095 = VERTEX_POINT ( 'NONE', #31136 ) ;
#47096 = ORIENTED_EDGE ( 'NONE', *, *, #37095, .F. ) ;
#47097 = CARTESIAN_POINT ( 'NONE',  ( 2.165460538733997353, 5.905511811023623991, 0.04798874274655766381 ) ) ;
#47098 = ORIENTED_EDGE ( 'NONE', *, *, #42269, .T. ) ;
#47099 = ADVANCED_FACE ( 'NONE', ( #50440 ), #30887, .T. ) ;
#47100 = CARTESIAN_POINT ( 'NONE',  ( 0.000000000000000000, 3.267716535433071279, -8.878505979408855953E-16 ) ) ;
#47101 = CARTESIAN_POINT ( 'NONE',  ( 0.000000000000000000, 3.267716535433071279, -1.889763779527552368 ) ) ;
#47102 = CARTESIAN_POINT ( 'NONE',  ( -0.2198976605848039223, 1.205361022782829114E-17, -1.894256224240784103 ) ) ;
#47103 = EDGE_CURVE ( 'NONE', #14452, #695, #32649, .T. ) ;
#47104 = PLANE ( 'NONE',  #12402 ) ;
#47105 = DIRECTION ( 'NONE',  ( 1.000000000000000000, -0.000000000000000000, 0.000000000000000000 ) ) ;
#47106 = CARTESIAN_POINT ( 'NONE',  ( -1.636583440222564301, 3.346456692913386100, -1.574803149606293307 ) ) ;
#47107 = VERTEX_POINT ( 'NONE', #17427 ) ;
#47108 = CARTESIAN_POINT ( 'NONE',  ( 0.000000000000000000, 3.267716535433071279, -2.106299212598425008 ) ) ;
#47109 = DIRECTION ( 'NONE',  ( 1.000000000000000000, 0.000000000000000000, 0.000000000000000000 ) ) ;
#47110 = EDGE_CURVE ( 'NONE', #3878, #18162, #27669, .T. ) ;
#47111 = CARTESIAN_POINT ( 'NONE',  ( 0.04921259842519689481, 0.009569417371913045700, 1.905847912026497948 ) ) ;
#47112 = VERTEX_POINT ( 'NONE', #28788 ) ;
#47113 = CARTESIAN_POINT ( 'NONE',  ( -0.1450362469327511061, 1.574803149606302854, -2.160491579385214411 ) ) ;
#47114 = LINE ( 'NONE', #23153, #45043 ) ;
#47115 = ORIENTED_EDGE ( 'NONE', *, *, #25513, .T. ) ;
#47116 = CARTESIAN_POINT ( 'NONE',  ( 0.000000000000000000, 3.267716535433071279, -1.102362204724405492 ) ) ;
#47117 = CARTESIAN_POINT ( 'NONE',  ( -1.628069513120385503, 0.001843152681973240061, -0.6423508795876955446 ) ) ;
#47118 = LINE ( 'NONE', #24445, #39162 ) ;
#47119 = EDGE_CURVE ( 'NONE', #23450, #660, #4788, .T. ) ;
#47120 = AXIS2_PLACEMENT_3D ( 'NONE', #13814, #41431, #6578 ) ;
#47121 = DIRECTION ( 'NONE',  ( -0.000000000000000000, 1.000000000000000000, -0.000000000000000000 ) ) ;
#47122 = ORIENTED_EDGE ( 'NONE', *, *, #22379, .T. ) ;
#47123 = CARTESIAN_POINT ( 'NONE',  ( -0.2727639067037607723, 3.346456692913386100, -1.417322834645664331 ) ) ;
#47124 = EDGE_CURVE ( 'NONE', #1491, #21615, #16673, .T. ) ;
#47125 = DIRECTION ( 'NONE',  ( -3.981026654148627524E-17, 1.000000000000000000, 1.225234019452863932E-16 ) ) ;
#47126 = VECTOR ( 'NONE', #27150, 39.37007874015748143 ) ;
#47127 = DIRECTION ( 'NONE',  ( -3.986037398843765983E-20, -1.000000000000000000, -1.160734090543304660E-16 ) ) ;
#47128 = LINE ( 'NONE', #46878, #24327 ) ;
#47129 = ORIENTED_EDGE ( 'NONE', *, *, #32175, .F. ) ;
#47130 = VERTEX_POINT ( 'NONE', #24411 ) ;
#47131 = EDGE_LOOP ( 'NONE', ( #7062, #34818, #34572, #20517 ) ) ;
#47132 = CARTESIAN_POINT ( 'NONE',  ( 1.871031489114177715, 0.000000000000000000, 0.9882585515110396956 ) ) ;
#47133 = EDGE_LOOP ( 'NONE', ( #48291, #13158, #963, #22902, #31842, #35192, #14487, #23663, #13118, #12197, #14294 ) ) ;
#47134 = CARTESIAN_POINT ( 'NONE',  ( -0.2727639067037608278, 0.000000000000000000, -0.03937007874015908959 ) ) ;
#47135 = PLANE ( 'NONE',  #28560 ) ;
#47136 = ORIENTED_EDGE ( 'NONE', *, *, #45823, .F. ) ;
#47137 = EDGE_CURVE ( 'NONE', #46760, #29688, #17508, .T. ) ;
#47138 = CARTESIAN_POINT ( 'NONE',  ( -0.3486774197067341041, 3.267716535433071279, 1.209717811016579571E-16 ) ) ;
#47139 = ORIENTED_EDGE ( 'NONE', *, *, #4953, .T. ) ;
#47140 = PLANE ( 'NONE',  #29033 ) ;
#47141 = EDGE_CURVE ( 'NONE', #40640, #12444, #33191, .T. ) ;
#47142 = CARTESIAN_POINT ( 'NONE',  ( -0.8942052331142547050, 0.000000000000000000, 0.1181102362204705658 ) ) ;
#47143 = ORIENTED_EDGE ( 'NONE', *, *, #25323, .T. ) ;
#47144 = ORIENTED_EDGE ( 'NONE', *, *, #2147, .F. ) ;
#47145 = CARTESIAN_POINT ( 'NONE',  ( -2.182111253630085290, 3.267716535433071279, 3.785359618865288779E-16 ) ) ;
#47146 = ORIENTED_EDGE ( 'NONE', *, *, #34091, .F. ) ;
#47147 = AXIS2_PLACEMENT_3D ( 'NONE', #34880, #34387, #42616 ) ;
#47148 = DIRECTION ( 'NONE',  ( -0.000000000000000000, 0.000000000000000000, 1.000000000000000000 ) ) ;
#47149 = VERTEX_POINT ( 'NONE', #1424 ) ;
#47150 = ORIENTED_EDGE ( 'NONE', *, *, #13139, .T. ) ;
#47151 = PLANE ( 'NONE',  #33099 ) ;
#47152 = VECTOR ( 'NONE', #3007, 39.37007874015748143 ) ;
#47153 = DIRECTION ( 'NONE',  ( -1.000000000000000000, 0.000000000000000000, -0.000000000000000000 ) ) ;
#47154 = ORIENTED_EDGE ( 'NONE', *, *, #43477, .T. ) ;
#47155 = VECTOR ( 'NONE', #34048, 39.37007874015748143 ) ;
#47156 = DIRECTION ( 'NONE',  ( -0.000000000000000000, 1.000000000000000000, -0.000000000000000000 ) ) ;
#47157 = ORIENTED_EDGE ( 'NONE', *, *, #34639, .T. ) ;
#47158 = LINE ( 'NONE', #27573, #22732 ) ;
#47159 = VECTOR ( 'NONE', #48822, 39.37007874015748143 ) ;
#47160 = VECTOR ( 'NONE', #21525, 39.37007874015748143 ) ;
#47161 = DIRECTION ( 'NONE',  ( -0.000000000000000000, 1.000000000000000000, -0.000000000000000000 ) ) ;
#47162 = EDGE_CURVE ( 'NONE', #33914, #25208, #20535, .T. ) ;
#47163 = DIRECTION ( 'NONE',  ( 0.8090169943749506709, 6.819399030548774257E-17, -0.5877852522924684742 ) ) ;
#47164 = EDGE_LOOP ( 'NONE', ( #16730, #46750, #4064, #20642 ) ) ;
#47165 = EDGE_LOOP ( 'NONE', ( #43491, #39438, #11565, #15106, #38886 ) ) ;
#47166 = CARTESIAN_POINT ( 'NONE',  ( 0.000000000000000000, 3.346456692913386100, 0.000000000000000000 ) ) ;
#47167 = DIRECTION ( 'NONE',  ( -1.000000000000000000, -0.000000000000000000, -0.000000000000000000 ) ) ;
#47168 = CARTESIAN_POINT ( 'NONE',  ( -0.8182917201112814842, 3.267716535433071279, 1.535433070866133898 ) ) ;
#47169 = FACE_OUTER_BOUND ( 'NONE', #29755, .T. ) ;
#47170 = ADVANCED_FACE ( 'NONE', ( #48873 ), #44526, .T. ) ;
#47171 = DIRECTION ( 'NONE',  ( 1.000000000000000000, 0.000000000000000000, 0.000000000000000000 ) ) ;
#47172 = EDGE_CURVE ( 'NONE', #5108, #12139, #48367, .T. ) ;
#47173 = CARTESIAN_POINT ( 'NONE',  ( 0.000000000000000000, 3.346456692913386100, 0.000000000000000000 ) ) ;
#47174 = ORIENTED_EDGE ( 'NONE', *, *, #9479, .T. ) ;
#47175 = ADVANCED_FACE ( 'NONE', ( #911 ), #7591, .T. ) ;
#47176 = B_SPLINE_CURVE_WITH_KNOTS ( 'NONE', 3,
 ( #30557, #31316, #49870, #42421 ),
 .UNSPECIFIED., .F., .F.,
 ( 4, 4 ),
 ( 0.0001501286205249034299, 0.002650226654156385194 ),
 .UNSPECIFIED. ) ;
#47177 = LINE ( 'NONE', #27845, #20102 ) ;
#47178 = DIMENSIONAL_EXPONENTS ( 1.000000000000000000, 0.000000000000000000, 0.000000000000000000, 0.000000000000000000, 0.000000000000000000, 0.000000000000000000, 0.000000000000000000 ) ;
#47179 = ORIENTED_EDGE ( 'NONE', *, *, #734, .T. ) ;
#47180 = FACE_OUTER_BOUND ( 'NONE', #41450, .T. ) ;
#47181 = EDGE_CURVE ( 'NONE', #40865, #7678, #16925, .T. ) ;
#47182 = VERTEX_POINT ( 'NONE', #43751 ) ;
#47183 = FACE_OUTER_BOUND ( 'NONE', #19031, .T. ) ;
#47184 = DIRECTION ( 'NONE',  ( -1.000000000000000000, 0.000000000000000000, 1.734723475976806848E-16 ) ) ;
#47185 = ORIENTED_EDGE ( 'NONE', *, *, #30868, .T. ) ;
#47186 = VECTOR ( 'NONE', #16916, 39.37007874015748143 ) ;
#47187 = DIRECTION ( 'NONE',  ( 1.000000000000000000, -0.000000000000000000, 0.000000000000000000 ) ) ;
#47188 = VERTEX_POINT ( 'NONE', #4532 ) ;
#47189 = CARTESIAN_POINT ( 'NONE',  ( -1.363819533518803029, 3.267716535433071279, 0.5905511811023582691 ) ) ;
#47190 = EDGE_LOOP ( 'NONE', ( #9493, #34268, #11325, #2222 ) ) ;
#47191 = CIRCLE ( 'NONE', #41498, 2.165354330708661568 ) ;
#47192 = EDGE_CURVE ( 'NONE', #13480, #43159, #28526, .T. ) ;
#47193 = AXIS2_PLACEMENT_3D ( 'NONE', #36111, #47683, #21132 ) ;
#47194 = FACE_OUTER_BOUND ( 'NONE', #47945, .T. ) ;
#47195 = CARTESIAN_POINT ( 'NONE',  ( 1.892591856222374469, 0.05823298773025239322, -0.4824499329568616157 ) ) ;
#47196 = EDGE_CURVE ( 'NONE', #37961, #14632, #15033, .T. ) ;
#47197 = VERTEX_POINT ( 'NONE', #32687 ) ;
#47198 = AXIS2_PLACEMENT_3D ( 'NONE', #678, #16433, #32187 ) ;
#47199 = CARTESIAN_POINT ( 'NONE',  ( 2.260029193386923652, 0.5219248566477788787, 0.3558038071150583792 ) ) ;
#47200 = VERTEX_POINT ( 'NONE', #13054 ) ;
#47201 = ORIENTED_EDGE ( 'NONE', *, *, #24228, .F. ) ;
#47202 = CARTESIAN_POINT ( 'NONE',  ( 0.2727639067037604392, 3.267716535433071279, -0.03937007874015908959 ) ) ;
#47203 = CARTESIAN_POINT ( 'NONE',  ( 2.112319093887386146, 0.000000000000000000, 0.3357951146312926904 ) ) ;
#47204 = CARTESIAN_POINT ( 'NONE',  ( 0.8182917201112817063, 3.346456692913386100, -1.732283464566923614 ) ) ;
#47205 = ORIENTED_EDGE ( 'NONE', *, *, #29168, .T. ) ;
#47206 = CARTESIAN_POINT ( 'NONE',  ( 1.062992125984252079, 0.000000000000000000, -1.181102362204724754 ) ) ;
#47207 = PLANE ( 'NONE',  #12632 ) ;
#47208 = ORIENTED_EDGE ( 'NONE', *, *, #36697, .F. ) ;
#47209 = DIRECTION ( 'NONE',  ( 0.000000000000000000, 0.000000000000000000, -1.000000000000000000 ) ) ;
#47210 = ORIENTED_EDGE ( 'NONE', *, *, #25731, .F. ) ;
#47211 = ORIENTED_EDGE ( 'NONE', *, *, #27070, .T. ) ;
#47212 = APPLICATION_PROTOCOL_DEFINITION ( 'draft international standard', 'automotive_design', 1998, #2865 ) ;
#47213 = ORIENTED_EDGE ( 'NONE', *, *, #26216, .F. ) ;
#47214 = CARTESIAN_POINT ( 'NONE',  ( 0.2727639067037604947, 3.267716535433071279, -0.7874015748031473194 ) ) ;
#47215 = FACE_OUTER_BOUND ( 'NONE', #1106, .T. ) ;
#47216 = FACE_OUTER_BOUND ( 'NONE', #24514, .T. ) ;
#47217 = CARTESIAN_POINT ( 'NONE',  ( 0.9319704666822036243, 0.04284687812831378811, 1.655805649632502430 ) ) ;
#47218 = ORIENTED_EDGE ( 'NONE', *, *, #34482, .T. ) ;
#47219 = VERTEX_POINT ( 'NONE', #5296 ) ;
#47220 = CIRCLE ( 'NONE', #34893, 1.743387098533651480 ) ;
#47221 = DIRECTION ( 'NONE',  ( -0.2225209339563184452, 1.288287287306305283E-16, 0.9749279121818227312 ) ) ;
#47222 = LINE ( 'NONE', #27895, #50641 ) ;
#47223 = AXIS2_PLACEMENT_3D ( 'NONE', #11107, #22727, #40890 ) ;
#47224 = ORIENTED_EDGE ( 'NONE', *, *, #14933, .F. ) ;
#47225 = DIRECTION ( 'NONE',  ( 0.000000000000000000, -1.000000000000000000, 0.000000000000000000 ) ) ;
#47226 = AXIS2_PLACEMENT_3D ( 'NONE', #47930, #24229, #44341 ) ;
#47227 = FACE_BOUND ( 'NONE', #22700, .T. ) ;
#47228 = VECTOR ( 'NONE', #28154, 39.37007874015748143 ) ;
#47229 = EDGE_CURVE ( 'NONE', #10448, #3033, #36801, .T. ) ;
#47230 = EDGE_CURVE ( 'NONE', #14792, #48519, #28215, .T. ) ;
#47231 = LINE ( 'NONE', #27387, #44837 ) ;
#47232 = EDGE_CURVE ( 'NONE', #21120, #7866, #51033, .T. ) ;
#47233 = FACE_OUTER_BOUND ( 'NONE', #4795, .T. ) ;
#47234 = CARTESIAN_POINT ( 'NONE',  ( 1.909347346926324684, 3.346456692913386100, -0.1574803149606304187 ) ) ;
#47235 = AXIS2_PLACEMENT_3D ( 'NONE', #19211, #34223, #26457 ) ;
#47236 = ORIENTED_EDGE ( 'NONE', *, *, #13447, .T. ) ;
#47237 = CARTESIAN_POINT ( 'NONE',  ( -0.9794755770252101534, 0.5905511811023621549, 1.097585813245683051 ) ) ;
#47238 = CARTESIAN_POINT ( 'NONE',  ( -1.712496953225537188, 3.346456692913386100, 0.1574803149606286423 ) ) ;
#47239 = ORIENTED_EDGE ( 'NONE', *, *, #11383, .T. ) ;
#47240 = VERTEX_POINT ( 'NONE', #25176 ) ;
#47241 = CARTESIAN_POINT ( 'NONE',  ( 0.000000000000000000, 3.346456692913386100, 0.000000000000000000 ) ) ;
#47242 = PLANE ( 'NONE',  #6410 ) ;
#47243 = DIRECTION ( 'NONE',  ( -0.000000000000000000, -1.000000000000000000, -0.000000000000000000 ) ) ;
#47244 = ORIENTED_EDGE ( 'NONE', *, *, #13694, .T. ) ;
#47245 = VERTEX_POINT ( 'NONE', #29296 ) ;
#47246 = CARTESIAN_POINT ( 'NONE',  ( 1.514466370292996800, 0.000000000000000000, 2.534789744887420149 ) ) ;
#47247 = B_SPLINE_CURVE_WITH_KNOTS ( 'NONE', 3,
 ( #35159, #34155, #49838, #6776 ),
 .UNSPECIFIED., .F., .F.,
 ( 4, 4 ),
 ( 0.1211873102087489551, 0.1625992483279400380 ),
 .UNSPECIFIED. ) ;
#47249 = ORIENTED_EDGE ( 'NONE', *, *, #25790, .F. ) ;
#47248 = EDGE_CURVE ( 'NONE', #17684, #45462, #25937, .T. ) ;
#47250 = CARTESIAN_POINT ( 'NONE',  ( 0.1968503937007873017, 3.346456692913386100, 0.3149606299212576177 ) ) ;
#47251 = ORIENTED_EDGE ( 'NONE', *, *, #11384, .T. ) ;
#47252 = FACE_OUTER_BOUND ( 'NONE', #22000, .T. ) ;
#47253 = EDGE_CURVE ( 'NONE', #29709, #12695, #12565, .T. ) ;
#47254 = DIRECTION ( 'NONE',  ( 1.160706738777435820E-16, 1.000000000000000000, 5.589669052740852391E-17 ) ) ;
#47255 = DIRECTION ( 'NONE',  ( 1.000000000000000000, 0.000000000000000000, 0.000000000000000000 ) ) ;
#47256 = EDGE_CURVE ( 'NONE', #32019, #4450, #34199, .T. ) ;
#47257 = ORIENTED_EDGE ( 'NONE', *, *, #16485, .T. ) ;
#47258 = ORIENTED_EDGE ( 'NONE', *, *, #33623, .T. ) ;
#47259 = VERTEX_POINT ( 'NONE', #6821 ) ;
#47260 = CARTESIAN_POINT ( 'NONE',  ( -0.5455278134075208785, 3.346456692913386100, 1.889763779527550369 ) ) ;
#47261 = DIRECTION ( 'NONE',  ( -3.469446951953613696E-16, 0.000000000000000000, -1.000000000000000000 ) ) ;
#47262 = VECTOR ( 'NONE', #25437, 39.37007874015748143 ) ;
#47264 = EDGE_LOOP ( 'NONE', ( #43697, #6067, #30412, #33250 ) ) ;
#47263 = EDGE_CURVE ( 'NONE', #22597, #44259, #34450, .T. ) ;
#47265 = ORIENTED_EDGE ( 'NONE', *, *, #28916, .F. ) ;
#47266 = AXIS2_PLACEMENT_3D ( 'NONE', #44612, #36901, #48715 ) ;
#47267 = CARTESIAN_POINT ( 'NONE',  ( 1.775400203342704986, 1.648464234653929106, -2.359903268218703332 ) ) ;
#47268 = DIRECTION ( 'NONE',  ( 1.734723475976806848E-16, -0.000000000000000000, 1.000000000000000000 ) ) ;
#47269 = DIRECTION ( 'NONE',  ( -0.9998717552508121775, -0.01601477604151182316, 0.000000000000000000 ) ) ;
#47270 = EDGE_CURVE ( 'NONE', #36033, #26276, #50137, .T. ) ;
#47271 = VECTOR ( 'NONE', #48588, 39.37007874015748143 ) ;
#47272 = VECTOR ( 'NONE', #1053, 39.37007874015748143 ) ;
#47273 = ORIENTED_EDGE ( 'NONE', *, *, #33370, .F. ) ;
#47274 = ORIENTED_EDGE ( 'NONE', *, *, #25455, .T. ) ;
#47275 = DIRECTION ( 'NONE',  ( -0.9998717552508122886, -0.01601477604151182316, 0.000000000000000000 ) ) ;
#47276 = DIRECTION ( 'NONE',  ( -0.6631698831091616952, 0.000000000000000000, 0.7484689079293679326 ) ) ;
#47277 = DIRECTION ( 'NONE',  ( 1.734723475976806848E-16, -0.000000000000000000, 1.000000000000000000 ) ) ;
#47278 = ORIENTED_EDGE ( 'NONE', *, *, #36510, .T. ) ;
#47279 = DIRECTION ( 'NONE',  ( -6.394449067488487880E-17, -1.000000000000000000, -9.687176266499690201E-17 ) ) ;
#47280 = PLANE ( 'NONE',  #2994 ) ;
#47281 = VECTOR ( 'NONE', #47498, 39.37007874015748143 ) ;
#47282 = VERTEX_POINT ( 'NONE', #38074 ) ;
#47283 = DIRECTION ( 'NONE',  ( -0.000000000000000000, 1.000000000000000000, -0.000000000000000000 ) ) ;
#47284 = VERTEX_POINT ( 'NONE', #5806 ) ;
#47285 = ORIENTED_EDGE ( 'NONE', *, *, #30719, .F. ) ;
#47286 = CARTESIAN_POINT ( 'NONE',  ( -0.8942052331142545940, 3.267716535433071279, 3.102397620449221495E-16 ) ) ;
#47287 = PLANE ( 'NONE',  #48158 ) ;
#47288 = CARTESIAN_POINT ( 'NONE',  ( 0.7423782071083092626, 0.000000000000000000, 1.574803149606291974 ) ) ;
#47289 = CARTESIAN_POINT ( 'NONE',  ( -1.883797214242443951, 0.5252390421956055766, -0.03533922825790704325 ) ) ;
#47290 = DIRECTION ( 'NONE',  ( -0.9998717552508122886, -0.01601477604151180928, 0.000000000000000000 ) ) ;
#47291 = ORIENTED_EDGE ( 'NONE', *, *, #8343, .T. ) ;
#47292 = ORIENTED_EDGE ( 'NONE', *, *, #605, .T. ) ;
#47293 = ORIENTED_EDGE ( 'NONE', *, *, #49744, .T. ) ;
#47294 = CARTESIAN_POINT ( 'NONE',  ( 2.947574761915768171, 1.765190094501404072, -0.1816379373804911379 ) ) ;
#47295 = FACE_OUTER_BOUND ( 'NONE', #50511, .T. ) ;
#47296 = EDGE_CURVE ( 'NONE', #23981, #22477, #42181, .T. ) ;
#47297 = PLANE ( 'NONE',  #30212 ) ;
#47298 = CARTESIAN_POINT ( 'NONE',  ( 1.909347346926324684, 0.000000000000000000, -0.6692913385826764205 ) ) ;
#47299 = ORIENTED_EDGE ( 'NONE', *, *, #18231, .T. ) ;
#47300 = VECTOR ( 'NONE', #8422, 39.37007874015748143 ) ;
#47301 = EDGE_CURVE ( 'NONE', #7706, #33786, #18702, .T. ) ;
#47302 = CARTESIAN_POINT ( 'NONE',  ( -0.07591351300297340121, 3.267716535433071279, 2.165354330708650465 ) ) ;
#47303 = VECTOR ( 'NONE', #2895, 39.37007874015748143 ) ;
#47304 = DIRECTION ( 'NONE',  ( 0.000000000000000000, 0.000000000000000000, 1.000000000000000000 ) ) ;
#47305 = EDGE_CURVE ( 'NONE', #29676, #20090, #9940, .T. ) ;
#47306 = AXIS2_PLACEMENT_3D ( 'NONE', #33037, #18796, #50477 ) ;
#47307 = AXIS2_PLACEMENT_3D ( 'NONE', #46624, #3286, #23406 ) ;
#47308 = VERTEX_POINT ( 'NONE', #14313 ) ;
#47309 = CARTESIAN_POINT ( 'NONE',  ( 0.000000000000000000, 1.574803149606302854, 0.000000000000000000 ) ) ;
#47310 = CARTESIAN_POINT ( 'NONE',  ( -1.312248418042854858, 1.574803149606302854, -1.722429524498108711 ) ) ;
#47311 = DIRECTION ( 'NONE',  ( 1.000000000000000000, 0.000000000000000000, 0.000000000000000000 ) ) ;
#47312 = VERTEX_POINT ( 'NONE', #2693 ) ;
#47313 = DIRECTION ( 'NONE',  ( -0.000000000000000000, 0.000000000000000000, 1.000000000000000000 ) ) ;
#47314 = DIRECTION ( 'NONE',  ( 1.734723475976806848E-16, -0.000000000000000000, 1.000000000000000000 ) ) ;
#47315 = CARTESIAN_POINT ( 'NONE',  ( -2.454875160333845674, 3.232777166330581320, -0.1574803149606298636 ) ) ;
#47316 = VECTOR ( 'NONE', #24757, 39.37007874015748854 ) ;
#47317 = EDGE_LOOP ( 'NONE', ( #32493, #11778, #30843, #22827 ) ) ;
#47318 = CARTESIAN_POINT ( 'NONE',  ( 0.000000000000000000, 3.267716535433071279, 1.417322834645662777 ) ) ;
#47319 = ORIENTED_EDGE ( 'NONE', *, *, #10183, .F. ) ;
#47320 = CARTESIAN_POINT ( 'NONE',  ( -0.8182917201112814842, 3.346456692913386100, 0.2755905511810998187 ) ) ;
#47321 = CARTESIAN_POINT ( 'NONE',  ( 1.174087487603957980, 5.905511811023623991, 1.869141625116387706 ) ) ;
#47322 = EDGE_CURVE ( 'NONE', #3406, #7692, #26187, .T. ) ;
#47323 = DIRECTION ( 'NONE',  ( -0.000000000000000000, 0.000000000000000000, 1.000000000000000000 ) ) ;
#47324 = DIRECTION ( 'NONE',  ( 1.734723475976806848E-16, -0.000000000000000000, 1.000000000000000000 ) ) ;
#47325 = ORIENTED_EDGE ( 'NONE', *, *, #22543, .T. ) ;
#47326 = ORIENTED_EDGE ( 'NONE', *, *, #40971, .T. ) ;
#47327 = CARTESIAN_POINT ( 'NONE',  ( 0.5455278134075208785, 3.346456692913386100, -1.889763779527552812 ) ) ;
#47328 = CARTESIAN_POINT ( 'NONE',  ( 2.182111253630085290, 0.000000000000000000, -1.161035397307311917E-15 ) ) ;
#47329 = EDGE_CURVE ( 'NONE', #22772, #24416, #6059, .T. ) ;
#47330 = ORIENTED_EDGE ( 'NONE', *, *, #31042, .F. ) ;
#47331 = CARTESIAN_POINT ( 'NONE',  ( -0.8942052331142552601, 0.000000000000000000, -1.259842519685034690 ) ) ;
#47332 = DIRECTION ( 'NONE',  ( 0.8090169943749422332, 0.000000000000000000, 0.5877852522924802425 ) ) ;
#47333 = LINE ( 'NONE', #26981, #25249 ) ;
#47334 = CARTESIAN_POINT ( 'NONE',  ( 0.000000000000000000, 3.267716535433071279, -0.1968503937007880511 ) ) ;
#47335 = VERTEX_POINT ( 'NONE', #14576 ) ;
#47336 = ORIENTED_EDGE ( 'NONE', *, *, #29661, .F. ) ;
#47337 = ORIENTED_EDGE ( 'NONE', *, *, #35788, .T. ) ;
#47338 = LINE ( 'NONE', #24404, #16736 ) ;
#47339 = LINE ( 'NONE', #12524, #23860 ) ;
#47340 = CARTESIAN_POINT ( 'NONE',  ( -1.363819533518803029, 3.346456692913386100, 0.7874015748031456541 ) ) ;
#47341 = VECTOR ( 'NONE', #42942, 39.37007874015748143 ) ;
#47342 = VERTEX_POINT ( 'NONE', #21813 ) ;
#47343 = CARTESIAN_POINT ( 'NONE',  ( -1.968719161901109960, 1.044049570087769885, 1.632946417767990654 ) ) ;
#47344 = AXIS2_PLACEMENT_3D ( 'NONE', #32569, #24301, #24036 ) ;
#47345 = VERTEX_POINT ( 'NONE', #22567 ) ;
#47346 = ORIENTED_EDGE ( 'NONE', *, *, #48201, .F. ) ;
#47347 = CARTESIAN_POINT ( 'NONE',  ( -1.439733046521776139, 3.346456692913386100, 0.6299212598425164567 ) ) ;
#47348 = AXIS2_PLACEMENT_3D ( 'NONE', #37799, #6031, #29012 ) ;
#47349 = VERTEX_POINT ( 'NONE', #45781 ) ;
#47350 = ORIENTED_EDGE ( 'NONE', *, *, #3808, .F. ) ;
#47351 = FACE_OUTER_BOUND ( 'NONE', #45800, .T. ) ;
#47352 = ORIENTED_EDGE ( 'NONE', *, *, #48546, .F. ) ;
#47353 = AXIS2_PLACEMENT_3D ( 'NONE', #268, #30511, #26624 ) ;
#47354 = DIRECTION ( 'NONE',  ( 1.000000000000000000, 0.000000000000000000, 0.000000000000000000 ) ) ;
#47355 = CARTESIAN_POINT ( 'NONE',  ( 0.000000000000000000, 0.5905511811023621549, 0.000000000000000000 ) ) ;
#47356 = CARTESIAN_POINT ( 'NONE',  ( 0.5455278134075208785, 3.346456692913386100, -1.889763779527552812 ) ) ;
#47357 = DIRECTION ( 'NONE',  ( -0.000000000000000000, 0.000000000000000000, 1.000000000000000000 ) ) ;
#47358 = EDGE_CURVE ( 'NONE', #33927, #20401, #46036, .T. ) ;
#47359 = FACE_OUTER_BOUND ( 'NONE', #14302, .T. ) ;
#47360 = LINE ( 'NONE', #153, #2373 ) ;
#47361 = ORIENTED_EDGE ( 'NONE', *, *, #12810, .F. ) ;
#47362 = EDGE_CURVE ( 'NONE', #15712, #42475, #10446, .T. ) ;
#47363 = DIRECTION ( 'NONE',  ( 0.000000000000000000, 1.160734090543304660E-16, -1.000000000000000000 ) ) ;
#47364 = LINE ( 'NONE', #35540, #13634 ) ;
#47365 = DIRECTION ( 'NONE',  ( -0.01601477604151182663, 0.9998717552508123996, -0.000000000000000000 ) ) ;
#47366 = EDGE_CURVE ( 'NONE', #9706, #25737, #6322, .T. ) ;
#47367 = PRODUCT_DEFINITION ( 'UNKNOWN', '', #39941, #36089 ) ;
#47368 = VERTEX_POINT ( 'NONE', #25677 ) ;
#47369 = CARTESIAN_POINT ( 'NONE',  ( 1.163887619842433718, 0.04656145577143805392, -1.518228404148327160 ) ) ;
#47370 = EDGE_CURVE ( 'NONE', #27692, #41895, #25758, .T. ) ;
#47371 = CARTESIAN_POINT ( 'NONE',  ( -0.8151651997737653366, 0.000000000000000000, -1.654713224395694571 ) ) ;
#47372 = ORIENTED_EDGE ( 'NONE', *, *, #21361, .T. ) ;
#47373 = LINE ( 'NONE', #50717, #6502 ) ;
#47374 = EDGE_CURVE ( 'NONE', #15116, #40070, #37317, .T. ) ;
#47375 = CARTESIAN_POINT ( 'NONE',  ( 2.079244330788078798, 1.744638041679277496, -1.431464546258592430 ) ) ;
#47376 = PLANE ( 'NONE',  #10351 ) ;
#47377 = AXIS2_PLACEMENT_3D ( 'NONE', #25062, #10084, #29182 ) ;
#47378 = AXIS2_PLACEMENT_3D ( 'NONE', #7922, #31676, #12312 ) ;
#47379 = VECTOR ( 'NONE', #13643, 39.37007874015748143 ) ;
#47380 = CARTESIAN_POINT ( 'NONE',  ( -1.091055626815042645, 3.267716535433071279, 1.892679809432644389E-16 ) ) ;
#47381 = ORIENTED_EDGE ( 'NONE', *, *, #21250, .F. ) ;
#47382 = CARTESIAN_POINT ( 'NONE',  ( -1.909347346926324462, 0.000000000000000000, -0.03937007874015881204 ) ) ;
#47383 = VECTOR ( 'NONE', #19162, 39.37007874015748143 ) ;
#47384 = CARTESIAN_POINT ( 'NONE',  ( 0.1067246931122726866, 0.02962905676920215767, 0.000000000000000000 ) ) ;
#47385 = CARTESIAN_POINT ( 'NONE',  ( -1.363819533518803473, 3.267716535433071279, -0.9842519685039344823 ) ) ;
#47386 = EDGE_CURVE ( 'NONE', #48433, #37126, #25863, .T. ) ;
#47387 = LINE ( 'NONE', #7177, #25957 ) ;
#47388 = ORIENTED_EDGE ( 'NONE', *, *, #16731, .T. ) ;
#47389 = VECTOR ( 'NONE', #16648, 39.37007874015748143 ) ;
#47390 = ORIENTED_EDGE ( 'NONE', *, *, #46181, .F. ) ;
#47391 = ORIENTED_EDGE ( 'NONE', *, *, #11007, .F. ) ;
#47392 = LINE ( 'NONE', #12065, #33694 ) ;
#47393 = VERTEX_POINT ( 'NONE', #1935 ) ;
#47394 = EDGE_CURVE ( 'NONE', #46268, #47393, #49134, .T. ) ;
#47395 = CARTESIAN_POINT ( 'NONE',  ( 0.2727639067037602172, 3.346456692913386100, -2.244094488188969727 ) ) ;
#47396 = FACE_OUTER_BOUND ( 'NONE', #39449, .T. ) ;
#47397 = ORIENTED_EDGE ( 'NONE', *, *, #21647, .T. ) ;
#47398 = DIRECTION ( 'NONE',  ( -3.469446951953613696E-16, 0.000000000000000000, -1.000000000000000000 ) ) ;
#47399 = ORIENTED_EDGE ( 'NONE', *, *, #12931, .T. ) ;
#47400 = ADVANCED_FACE ( 'NONE', ( #39072 ), #29857, .T. ) ;
#47401 = CARTESIAN_POINT ( 'NONE',  ( -1.152568299495734250, 1.574803149606302854, 1.833124570921536467 ) ) ;
#47402 = CARTESIAN_POINT ( 'NONE',  ( 1.540582001147990487, 3.213852389688475863, -1.929133858267710666 ) ) ;
#47403 = EDGE_LOOP ( 'NONE', ( #19423, #18826, #15812, #41698 ) ) ;
#47404 = ORIENTED_EDGE ( 'NONE', *, *, #48108, .T. ) ;
#47405 = CARTESIAN_POINT ( 'NONE',  ( -0.2727639067037607723, 3.346456692913386100, 0.4724409448818869817 ) ) ;
#47406 = ORIENTED_EDGE ( 'NONE', *, *, #37240, .F. ) ;
#47407 = ADVANCED_FACE ( 'NONE', ( #3199 ), #43438, .T. ) ;
#47408 = FACE_OUTER_BOUND ( 'NONE', #32642, .T. ) ;
#47409 = ORIENTED_EDGE ( 'NONE', *, *, #9130, .T. ) ;
#47410 = EDGE_LOOP ( 'NONE', ( #31382, #45942, #43145, #20005 ) ) ;
#47411 = DIRECTION ( 'NONE',  ( -0.000000000000000000, 1.000000000000000000, -0.000000000000000000 ) ) ;
#47412 = AXIS2_PLACEMENT_3D ( 'NONE', #27328, #39472, #19832 ) ;
#47413 = DIRECTION ( 'NONE',  ( -3.469446951953613696E-16, 0.000000000000000000, -1.000000000000000000 ) ) ;
#47414 = VECTOR ( 'NONE', #25556, 39.37007874015748143 ) ;
#47415 = VERTEX_POINT ( 'NONE', #4209 ) ;
#47416 = CARTESIAN_POINT ( 'NONE',  ( 2.889674983507178219, 0.000000000000000000, -0.6090712660037610471 ) ) ;
#47417 = AXIS2_PLACEMENT_3D ( 'NONE', #36785, #37300, #13800 ) ;
#47418 = VERTEX_POINT ( 'NONE', #19188 ) ;
#47419 = LINE ( 'NONE', #23708, #35149 ) ;
#47420 = PLANE ( 'NONE',  #36608 ) ;
#47421 = VECTOR ( 'NONE', #11374, 39.37007874015748143 ) ;
#47422 = DIRECTION ( 'NONE',  ( -3.469446951953613696E-16, 0.000000000000000000, -1.000000000000000000 ) ) ;
#47423 = ORIENTED_EDGE ( 'NONE', *, *, #8769, .T. ) ;
#47424 = ORIENTED_EDGE ( 'NONE', *, *, #527, .F. ) ;
#47425 = AXIS2_PLACEMENT_3D ( 'NONE', #23294, #11932, #19164 ) ;
#47426 = DIRECTION ( 'NONE',  ( 1.000000000000000000, 0.000000000000000000, -3.469446951953613696E-16 ) ) ;
#47427 = LINE ( 'NONE', #31219, #50950 ) ;
#47428 = DIRECTION ( 'NONE',  ( -0.000000000000000000, 0.000000000000000000, 1.000000000000000000 ) ) ;
#47429 = CARTESIAN_POINT ( 'NONE',  ( 2.889674983507178219, 1.665813060096536402, -0.6090712660037608250 ) ) ;
#47430 = CARTESIAN_POINT ( 'NONE',  ( -0.7855418668307149188, 0.000000000000000000, -2.846347029613745416 ) ) ;
#47431 = EDGE_CURVE ( 'NONE', #14934, #15242, #49635, .T. ) ;
#47432 = CARTESIAN_POINT ( 'NONE',  ( -0.9914495361339011881, 1.605369965488712136, 2.781765111341808705 ) ) ;
#47433 = VERTEX_POINT ( 'NONE', #23568 ) ;
#47434 = EDGE_CURVE ( 'NONE', #20959, #31365, #11954, .T. ) ;
#47435 = DIRECTION ( 'NONE',  ( 1.000000000000000000, 0.000000000000000000, -3.469446951953613696E-16 ) ) ;
#47436 = VERTEX_POINT ( 'NONE', #8083 ) ;
#47437 = CARTESIAN_POINT ( 'NONE',  ( -1.636583440222564301, 3.346456692913386100, -0.6299212598425177889 ) ) ;
#47438 = ORIENTED_EDGE ( 'NONE', *, *, #37952, .F. ) ;
#47439 = DIRECTION ( 'NONE',  ( 2.126200446592111359E-16, 0.6427876096865404731, -0.7660444431189771253 ) ) ;
#47440 = LINE ( 'NONE', #27853, #17171 ) ;
#47441 = LINE ( 'NONE', #39742, #19331 ) ;
#47442 = ORIENTED_EDGE ( 'NONE', *, *, #47103, .F. ) ;
#47443 = VECTOR ( 'NONE', #39025, 39.37007874015748143 ) ;
#47444 = VECTOR ( 'NONE', #48264, 39.37007874015748143 ) ;
#47445 = CARTESIAN_POINT ( 'NONE',  ( -0.8182917201112819283, 0.000000000000000000, -0.1574803149606301411 ) ) ;
#47446 = AXIS2_PLACEMENT_3D ( 'NONE', #21121, #26006, #5367 ) ;
#47447 = EDGE_LOOP ( 'NONE', ( #20674, #35625, #4170, #30214 ) ) ;
#47448 = PLANE ( 'NONE',  #29600 ) ;
#47449 = VECTOR ( 'NONE', #20522, 39.37007874015748143 ) ;
#47450 = ORIENTED_EDGE ( 'NONE', *, *, #49803, .T. ) ;
#47451 = CARTESIAN_POINT ( 'NONE',  ( -1.636583440222564301, 0.000000000000000000, -1.574803149606293307 ) ) ;
#47452 = CARTESIAN_POINT ( 'NONE',  ( -1.166969139818015977, 3.267716535433071279, 4.048737525165546155E-16 ) ) ;
#47453 = VECTOR ( 'NONE', #16601, 39.37007874015748143 ) ;
#47454 = EDGE_CURVE ( 'NONE', #5052, #351, #35706, .T. ) ;
#47455 = ORIENTED_EDGE ( 'NONE', *, *, #13217, .T. ) ;
#47456 = VECTOR ( 'NONE', #38929, 39.37007874015748854 ) ;
#47457 = CARTESIAN_POINT ( 'NONE',  ( -0.8182917201112814842, 3.267716535433071279, 1.417322834645662777 ) ) ;
#47458 = ORIENTED_EDGE ( 'NONE', *, *, #19122, .F. ) ;
#47459 = VERTEX_POINT ( 'NONE', #3959 ) ;
#47460 = CARTESIAN_POINT ( 'NONE',  ( 0.000000000000000000, 3.267716535433071279, 2.165354330708650910 ) ) ;
#47461 = LINE ( 'NONE', #47974, #16590 ) ;
#47462 = DIRECTION ( 'NONE',  ( 0.000000000000000000, 0.000000000000000000, -1.000000000000000000 ) ) ;
#47463 = EDGE_CURVE ( 'NONE', #50445, #12429, #15976, .T. ) ;
#47464 = ORIENTED_EDGE ( 'NONE', *, *, #36655, .T. ) ;
#47465 = CARTESIAN_POINT ( 'NONE',  ( 0.000000000000000000, 3.267716535433071279, 1.377952755905504256 ) ) ;
#47466 = LINE ( 'NONE', #23758, #13488 ) ;
#47467 = EDGE_CURVE ( 'NONE', #13332, #42385, #15325, .T. ) ;
#47468 = ORIENTED_EDGE ( 'NONE', *, *, #26603, .F. ) ;
#47469 = DIRECTION ( 'NONE',  ( 1.000000000000000000, 0.000000000000000000, 0.000000000000000000 ) ) ;
#47470 = EDGE_CURVE ( 'NONE', #34071, #35542, #31078, .T. ) ;
#47471 = ORIENTED_EDGE ( 'NONE', *, *, #1118, .T. ) ;
#47472 = ORIENTED_EDGE ( 'NONE', *, *, #45059, .T. ) ;
#47473 = APPLICATION_PROTOCOL_DEFINITION ( 'draft international standard', 'automotive_design', 1998, #5505 ) ;
#47475 = EDGE_CURVE ( 'NONE', #50554, #39301, #49861, .T. ) ;
#47474 = VERTEX_POINT ( 'NONE', #50383 ) ;
#47476 = DIRECTION ( 'NONE',  ( 1.734723475976806848E-16, -0.000000000000000000, 1.000000000000000000 ) ) ;
#47477 = CYLINDRICAL_SURFACE ( 'NONE', #13457, 2.165354330708661568 ) ;
#47479 = LINE ( 'NONE', #8279, #36634 ) ;
#47478 = VECTOR ( 'NONE', #29323, 39.37007874015748143 ) ;
#47480 = CARTESIAN_POINT ( 'NONE',  ( 2.712427995346972320, 1.659614058134468495, 0.4170853886664333543 ) ) ;
#47481 = ORIENTED_EDGE ( 'NONE', *, *, #14249, .T. ) ;
#47482 = EDGE_LOOP ( 'NONE', ( #27637, #12155, #44036, #33208, #37020, #21749, #11427 ) ) ;
#47483 = AXIS2_PLACEMENT_3D ( 'NONE', #26252, #35271, #45847 ) ;
#47484 = CARTESIAN_POINT ( 'NONE',  ( 0.7090793742677682365, 0.03927686936677046714, 1.749277966691849429 ) ) ;
#47485 = VECTOR ( 'NONE', #26698, 39.37007874015748143 ) ;
#47486 = DIRECTION ( 'NONE',  ( -1.000000000000000000, -0.000000000000000000, -0.000000000000000000 ) ) ;
#47487 = VERTEX_POINT ( 'NONE', #43180 ) ;
#47488 = DIRECTION ( 'NONE',  ( 1.000000000000000000, 0.000000000000000000, 0.000000000000000000 ) ) ;
#47489 = CARTESIAN_POINT ( 'NONE',  ( 2.088343298084792021, -7.108564423737583947E-17, 0.6267986818430602014 ) ) ;
#47490 = EDGE_CURVE ( 'NONE', #14000, #12695, #11453, .T. ) ;
#47491 = VECTOR ( 'NONE', #31650, 39.37007874015748143 ) ;
#47492 = ADVANCED_FACE ( 'NONE', ( #11203 ), #50881, .F. ) ;
#47493 = LINE ( 'NONE', #12163, #5269 ) ;
#47494 = LINE ( 'NONE', #12164, #12928 ) ;
#47495 = AXIS2_PLACEMENT_3D ( 'NONE', #35444, #63, #47269 ) ;
#47496 = VERTEX_POINT ( 'NONE', #3450 ) ;
#47497 = EDGE_CURVE ( 'NONE', #8443, #47240, #42684, .T. ) ;
#47498 = DIRECTION ( 'NONE',  ( -3.469446951953613696E-16, 0.000000000000000000, -1.000000000000000000 ) ) ;
#47499 = EDGE_LOOP ( 'NONE', ( #23958, #3497, #34684, #18102 ) ) ;
#47500 = VERTEX_POINT ( 'NONE', #7079 ) ;
#47501 = CARTESIAN_POINT ( 'NONE',  ( 1.287906020515829919, 3.346456692913386100, -1.666671669919371102 ) ) ;
#47502 = CARTESIAN_POINT ( 'NONE',  ( -1.091055626815042645, 3.346456692913386100, 2.204724409448808764 ) ) ;
#47503 = LINE ( 'NONE', #294, #37092 ) ;
#47504 = VERTEX_POINT ( 'NONE', #47026 ) ;
#47505 = VERTEX_POINT ( 'NONE', #42929 ) ;
#47506 = CARTESIAN_POINT ( 'NONE',  ( 0.5762653268100312864, 0.000000000000000000, -1.903066372058335620 ) ) ;
#47507 = ORIENTED_EDGE ( 'NONE', *, *, #7752, .F. ) ;
#47508 = CARTESIAN_POINT ( 'NONE',  ( -1.636583440222564301, 3.346456692913386100, -1.259842519685034468 ) ) ;
#47509 = ORIENTED_EDGE ( 'NONE', *, *, #7384, .F. ) ;
#47510 = CARTESIAN_POINT ( 'NONE',  ( 1.642191404871903071, 0.000000000000000000, 0.5853255206279913692 ) ) ;
#47511 = CARTESIAN_POINT ( 'NONE',  ( 1.905671854841463952, 1.472358791367697650, 2.256015092822682089 ) ) ;
#47512 = FACE_OUTER_BOUND ( 'NONE', #46594, .T. ) ;
#47513 = AXIS2_PLACEMENT_3D ( 'NONE', #25385, #21516, #33911 ) ;
#47514 = EDGE_CURVE ( 'NONE', #12624, #45538, #9287, .T. ) ;
#47515 = VERTEX_POINT ( 'NONE', #27694 ) ;
#47516 = VERTEX_POINT ( 'NONE', #23828 ) ;
#47517 = VERTEX_POINT ( 'NONE', #7830 ) ;
#47518 = CARTESIAN_POINT ( 'NONE',  ( 1.363819533518803251, 0.000000000000000000, 0.4724409448818871482 ) ) ;
#47519 = AXIS2_PLACEMENT_3D ( 'NONE', #6136, #41758, #2520 ) ;
#47520 = FACE_OUTER_BOUND ( 'NONE', #24714, .T. ) ;
#47521 = ORIENTED_EDGE ( 'NONE', *, *, #27007, .T. ) ;
#47522 = ORIENTED_EDGE ( 'NONE', *, *, #15522, .T. ) ;
#47523 = LINE ( 'NONE', #16847, #16543 ) ;
#47524 = CARTESIAN_POINT ( 'NONE',  ( 1.363819533518803251, 3.346456692913386100, 0.9055118110236164419 ) ) ;
#47525 = CARTESIAN_POINT ( 'NONE',  ( 0.4350747367505088947, 1.205361022782829114E-17, -2.121846421795415161 ) ) ;
#47526 = ORIENTED_EDGE ( 'NONE', *, *, #42723, .F. ) ;
#47527 = ORIENTED_EDGE ( 'NONE', *, *, #21093, .F. ) ;
#47528 = EDGE_CURVE ( 'NONE', #25746, #29370, #75, .T. ) ;
#47529 = FACE_OUTER_BOUND ( 'NONE', #35523, .T. ) ;
#47530 = DIRECTION ( 'NONE',  ( -0.000000000000000000, 1.000000000000000000, -0.000000000000000000 ) ) ;
#47531 = VECTOR ( 'NONE', #8857, 39.37007874015748143 ) ;
#47532 = CARTESIAN_POINT ( 'NONE',  ( -1.363819533518803473, 0.000000000000000000, -0.9842519685039344823 ) ) ;
#47533 = ADVANCED_FACE ( 'NONE', ( #31582 ), #4724, .F. ) ;
#47534 = EDGE_LOOP ( 'NONE', ( #45023, #25073, #38203, #28768 ) ) ;
#47535 = CARTESIAN_POINT ( 'NONE',  ( 0.000000000000000000, 3.267716535433071279, -2.047244094488181343 ) ) ;
#47536 = EDGE_CURVE ( 'NONE', #26618, #19754, #20463, .T. ) ;
#47537 = CARTESIAN_POINT ( 'NONE',  ( -1.091055626815042645, 3.244425644700272393, 2.198663907112657689 ) ) ;
#47538 = ORIENTED_EDGE ( 'NONE', *, *, #29273, .T. ) ;
#47539 = DIRECTION ( 'NONE',  ( -0.000000000000000000, -1.000000000000000000, -0.000000000000000000 ) ) ;
#47540 = VERTEX_POINT ( 'NONE', #9100 ) ;
#47541 = ORIENTED_EDGE ( 'NONE', *, *, #20344, .F. ) ;
#47542 = DIRECTION ( 'NONE',  ( 1.000000000000000000, 0.000000000000000000, 0.000000000000000000 ) ) ;
#47543 = DIRECTION ( 'NONE',  ( -0.000000000000000000, 0.000000000000000000, 1.000000000000000000 ) ) ;
#47544 = DIRECTION ( 'NONE',  ( 1.000000000000000000, -0.000000000000000000, 0.000000000000000000 ) ) ;
#47545 = CARTESIAN_POINT ( 'NONE',  ( -0.7874015748031498729, 0.000000000000000000, -1.138269997360109921E-16 ) ) ;
#47546 = CARTESIAN_POINT ( 'NONE',  ( 0.4600188520506054979, 0.02342673975412612117, -1.851825020600145644 ) ) ;
#47547 = ORIENTED_EDGE ( 'NONE', *, *, #26200, .F. ) ;
#47548 = ORIENTED_EDGE ( 'NONE', *, *, #32469, .T. ) ;
#47549 = EDGE_CURVE ( 'NONE', #5669, #6147, #24600, .T. ) ;
#47550 = ORIENTED_EDGE ( 'NONE', *, *, #32233, .F. ) ;
#47551 = DIRECTION ( 'NONE',  ( -3.469446951953613696E-16, 0.000000000000000000, -1.000000000000000000 ) ) ;
#47552 = CARTESIAN_POINT ( 'NONE',  ( 0.1155636338427008941, -0.5222242541845523167, 0.000000000000000000 ) ) ;
#47553 = EDGE_CURVE ( 'NONE', #11040, #42606, #17113, .T. ) ;
#47554 = VECTOR ( 'NONE', #30504, 39.37007874015748143 ) ;
#47555 = VECTOR ( 'NONE', #3922, 39.37007874015748143 ) ;
#47556 = EDGE_CURVE ( 'NONE', #37702, #22113, #5153, .T. ) ;
#47557 = DIRECTION ( 'NONE',  ( -0.000000000000000000, 0.000000000000000000, 1.000000000000000000 ) ) ;
#47558 = LINE ( 'NONE', #8361, #9747 ) ;
#47559 = VECTOR ( 'NONE', #14590, 39.37007874015748143 ) ;
#47560 = ORIENTED_EDGE ( 'NONE', *, *, #39318, .F. ) ;
#47561 = FACE_OUTER_BOUND ( 'NONE', #1710, .T. ) ;
#47562 = EDGE_CURVE ( 'NONE', #14593, #7604, #24854, .T. ) ;
#47563 = FACE_OUTER_BOUND ( 'NONE', #28072, .T. ) ;
#47564 = ORIENTED_EDGE ( 'NONE', *, *, #34828, .T. ) ;
#47565 = CARTESIAN_POINT ( 'NONE',  ( -1.731276487347650050, 1.684260316500282517, -1.723356343879357100 ) ) ;
#47566 = LINE ( 'NONE', #32644, #5559 ) ;
#47567 = CARTESIAN_POINT ( 'NONE',  ( -0.5150676061901260372, 0.000000000000000000, -1.804318609754868019 ) ) ;
#47568 = ORIENTED_EDGE ( 'NONE', *, *, #11208, .T. ) ;
#47569 = DIRECTION ( 'NONE',  ( -3.469446951953613696E-16, 0.000000000000000000, -1.000000000000000000 ) ) ;
#47570 = CARTESIAN_POINT ( 'NONE',  ( -1.453832412804729302, 0.000000000000000000, -1.018633753700964428 ) ) ;
#47571 = CARTESIAN_POINT ( 'NONE',  ( -0.1730139111830206189, 1.610516408500926477, -2.471348888976017122 ) ) ;
#47572 = EDGE_LOOP ( 'NONE', ( #4085, #16914 ) ) ;
#47573 = CARTESIAN_POINT ( 'NONE',  ( 2.151809081513405442, 5.118110236220475784, 0.2418202932658665705 ) ) ;
#47574 = CARTESIAN_POINT ( 'NONE',  ( 1.363819533518803029, 3.346456692913386100, -1.732283464566923170 ) ) ;
#47575 = VERTEX_POINT ( 'NONE', #24344 ) ;
#47576 = AXIS2_PLACEMENT_3D ( 'NONE', #50703, #11529, #27265 ) ;
#47577 = CARTESIAN_POINT ( 'NONE',  ( 0.2727639067037602172, 0.000000000000000000, -2.047244094488182231 ) ) ;
#47578 = DIRECTION ( 'NONE',  ( -3.469446951953613696E-16, 0.000000000000000000, -1.000000000000000000 ) ) ;
#47579 = DIRECTION ( 'NONE',  ( 1.734723475976806848E-16, -0.000000000000000000, 1.000000000000000000 ) ) ;
#47580 = DIRECTION ( 'NONE',  ( -1.000000000000000000, 0.000000000000000000, 1.734723475976806848E-16 ) ) ;
#47581 = ORIENTED_EDGE ( 'NONE', *, *, #17080, .T. ) ;
#47582 = VERTEX_POINT ( 'NONE', #36225 ) ;
#47583 = LINE ( 'NONE', #12260, #29822 ) ;
#47584 = CARTESIAN_POINT ( 'NONE',  ( 1.686111637834603938, 0.05492582915004715072, 0.9632209503012270080 ) ) ;
#47585 = ORIENTED_EDGE ( 'NONE', *, *, #44012, .F. ) ;
#47586 = CARTESIAN_POINT ( 'NONE',  ( -0.2198976605848039223, 1.205361022782829114E-17, -1.894256224240784103 ) ) ;
#47587 = CARTESIAN_POINT ( 'NONE',  ( 2.926032761125787029, 0.000000000000000000, 0.3963580683592521914 ) ) ;
#47588 = FACE_OUTER_BOUND ( 'NONE', #31741, .T. ) ;
#47589 = DIRECTION ( 'NONE',  ( -0.000000000000000000, 1.000000000000000000, -0.000000000000000000 ) ) ;
#47590 = ORIENTED_EDGE ( 'NONE', *, *, #3518, .T. ) ;
#47591 = ORIENTED_EDGE ( 'NONE', *, *, #44616, .T. ) ;
#47592 = EDGE_CURVE ( 'NONE', #37038, #3878, #6112, .T. ) ;
#47593 = DIRECTION ( 'NONE',  ( -3.469446951953613696E-16, 0.000000000000000000, -1.000000000000000000 ) ) ;
#47594 = LINE ( 'NONE', #36284, #17577 ) ;
#47595 = AXIS2_PLACEMENT_3D ( 'NONE', #50852, #19160, #27158 ) ;
#47596 = VECTOR ( 'NONE', #32137, 39.37007874015748143 ) ;
#47597 = DIRECTION ( 'NONE',  ( 1.734723475976806848E-16, -0.000000000000000000, 1.000000000000000000 ) ) ;
#47598 = CARTESIAN_POINT ( 'NONE',  ( 0.8182917201112819283, 0.000000000000000000, 0.7874015748031454320 ) ) ;
#47599 = ADVANCED_FACE ( 'NONE', ( #8849 ), #25111, .F. ) ;
#47600 = FACE_BOUND ( 'NONE', #13943, .T. ) ;
#47601 = VERTEX_POINT ( 'NONE', #36477 ) ;
#47602 = EDGE_CURVE ( 'NONE', #945, #11586, #12983, .T. ) ;
#47603 = CARTESIAN_POINT ( 'NONE',  ( 0.2483335008317506531, 0.5236491086109019699, -2.210204286096038473 ) ) ;
#47604 = ORIENTED_EDGE ( 'NONE', *, *, #33603, .T. ) ;
#47606 = ORIENTED_EDGE ( 'NONE', *, *, #1623, .T. ) ;
#47605 = AXIS2_PLACEMENT_3D ( 'NONE', #23003, #35386, #46460 ) ;
#47607 = FACE_OUTER_BOUND ( 'NONE', #4104, .T. ) ;
#47608 = EDGE_CURVE ( 'NONE', #12011, #49793, #24014, .T. ) ;
#47609 = VECTOR ( 'NONE', #30865, 39.37007874015748143 ) ;
#47610 = VERTEX_POINT ( 'NONE', #40093 ) ;
#47611 = ORIENTED_EDGE ( 'NONE', *, *, #13864, .F. ) ;
#47612 = DIRECTION ( 'NONE',  ( -0.000000000000000000, 0.000000000000000000, 1.000000000000000000 ) ) ;
#47613 = AXIS2_PLACEMENT_3D ( 'NONE', #25044, #25299, #33827 ) ;
#47614 = VERTEX_POINT ( 'NONE', #20202 ) ;
#47615 = ADVANCED_FACE ( 'NONE', ( #20980 ), #1094, .F. ) ;
#47617 = PLANE ( 'NONE',  #13095 ) ;
#47616 = VECTOR ( 'NONE', #43393, 39.37007874015748143 ) ;
#47618 = LINE ( 'NONE', #671, #15362 ) ;
#47619 = DIRECTION ( 'NONE',  ( -3.469446951953613696E-16, 0.000000000000000000, -1.000000000000000000 ) ) ;
#47620 = ADVANCED_FACE ( 'NONE', ( #32875 ), #1355, .T. ) ;
#47621 = DIRECTION ( 'NONE',  ( -0.000000000000000000, 1.000000000000000000, -0.000000000000000000 ) ) ;
#47622 = PLANE ( 'NONE',  #9695 ) ;
#47623 = FACE_OUTER_BOUND ( 'NONE', #32890, .T. ) ;
#47624 = VERTEX_POINT ( 'NONE', #13240 ) ;
#47625 = CARTESIAN_POINT ( 'NONE',  ( 1.266359212274407620, 1.486365060966521323, -2.667465348741127951 ) ) ;
#47626 = EDGE_CURVE ( 'NONE', #15234, #10014, #44705, .T. ) ;
#47627 = DIRECTION ( 'NONE',  ( -0.000000000000000000, -1.000000000000000000, -0.000000000000000000 ) ) ;
#47628 = CARTESIAN_POINT ( 'NONE',  ( 1.636583440222563857, 3.267716535433071279, -2.839019714148966584E-16 ) ) ;
#47629 = ORIENTED_EDGE ( 'NONE', *, *, #9180, .F. ) ;
#47630 = DIRECTION ( 'NONE',  ( -1.000000000000000000, 0.000000000000000000, -0.000000000000000000 ) ) ;
#47631 = DIRECTION ( 'NONE',  ( -0.000000000000000000, -1.000000000000000000, -0.000000000000000000 ) ) ;
#47632 = VERTEX_POINT ( 'NONE', #24084 ) ;
#47633 = CARTESIAN_POINT ( 'NONE',  ( 2.928234411561841277, 1.447231713130496367, 0.3801048321602038538 ) ) ;
#47634 = VECTOR ( 'NONE', #16055, 39.37007874015748143 ) ;
#47635 = CARTESIAN_POINT ( 'NONE',  ( 1.810607833951273227, 0.05691986357332023266, -0.7203715021987137090 ) ) ;
#47636 = LINE ( 'NONE', #43783, #49033 ) ;
#47637 = AXIS2_PLACEMENT_3D ( 'NONE', #2455, #29812, #30575 ) ;
#47638 = CARTESIAN_POINT ( 'NONE',  ( -1.497193542162873259, 0.002659885201759431498, -0.9293214240255518455 ) ) ;
#47639 = ORIENTED_EDGE ( 'NONE', *, *, #10751, .T. ) ;
#47640 = LINE ( 'NONE', #23931, #875 ) ;
#47641 = DIRECTION ( 'NONE',  ( -3.469446951953613696E-16, 0.000000000000000000, -1.000000000000000000 ) ) ;
#47642 = VECTOR ( 'NONE', #24567, 39.37007874015748143 ) ;
#47643 = DIRECTION ( 'NONE',  ( -0.000000000000000000, 1.000000000000000000, -0.000000000000000000 ) ) ;
#47644 = CARTESIAN_POINT ( 'NONE',  ( 1.427293369312940152, 0.000000000000000000, -1.001115484471646111 ) ) ;
#47645 = VECTOR ( 'NONE', #35529, 39.37007874015748143 ) ;
#47646 = ORIENTED_EDGE ( 'NONE', *, *, #47659, .F. ) ;
#47647 = EDGE_LOOP ( 'NONE', ( #15738, #16071, #39992, #14404 ) ) ;
#47648 = DIRECTION ( 'NONE',  ( -0.000000000000000000, 1.000000000000000000, -0.000000000000000000 ) ) ;
#47649 = ORIENTED_EDGE ( 'NONE', *, *, #4290, .T. ) ;
#47650 = VECTOR ( 'NONE', #31674, 39.37007874015748143 ) ;
#47651 = DIRECTION ( 'NONE',  ( -0.000000000000000000, -1.000000000000000000, -0.000000000000000000 ) ) ;
#47652 = ORIENTED_EDGE ( 'NONE', *, *, #41310, .T. ) ;
#47653 = DIRECTION ( 'NONE',  ( 1.000000000000000000, 0.000000000000000000, 0.000000000000000000 ) ) ;
#47654 = VERTEX_POINT ( 'NONE', #16085 ) ;
#47655 = LINE ( 'NONE', #32478, #17538 ) ;
#47656 = PLANE ( 'NONE',  #6707 ) ;
#47657 = EDGE_CURVE ( 'NONE', #16142, #46986, #12461, .T. ) ;
#47658 = VERTEX_POINT ( 'NONE', #27952 ) ;
#47659 = EDGE_CURVE ( 'NONE', #15209, #43842, #22219, .T. ) ;
#47660 = PLANE ( 'NONE',  #33148 ) ;
#47661 = VERTEX_POINT ( 'NONE', #28202 ) ;
#47662 = EDGE_CURVE ( 'NONE', #36186, #47487, #14245, .T. ) ;
#47663 = LINE ( 'NONE', #20334, #30369 ) ;
#47664 = AXIS2_PLACEMENT_3D ( 'NONE', #5340, #13349, #17225 ) ;
#47666 = ORIENTED_EDGE ( 'NONE', *, *, #25653, .T. ) ;
#47665 = ADVANCED_FACE ( 'NONE', ( #33885 ), #6251, .F. ) ;
#47667 = EDGE_LOOP ( 'NONE', ( #26730, #28951, #26469, #13156 ) ) ;
#47668 = DIRECTION ( 'NONE',  ( 0.000000000000000000, 0.000000000000000000, 1.000000000000000000 ) ) ;
#47669 = FACE_OUTER_BOUND ( 'NONE', #33759, .T. ) ;
#47670 = ORIENTED_EDGE ( 'NONE', *, *, #29168, .F. ) ;
#47671 = CARTESIAN_POINT ( 'NONE',  ( -1.901721518280075296, 3.346456692913386100, 0.9055118110236167750 ) ) ;
#47672 = EDGE_LOOP ( 'NONE', ( #6975, #32750, #3727, #28134, #50975, #34406 ) ) ;
#47673 = CARTESIAN_POINT ( 'NONE',  ( 2.607957125084112704, 1.661418195339335213, 1.384772967396189491 ) ) ;
#47674 = DIRECTION ( 'NONE',  ( 0.000000000000000000, 0.000000000000000000, -1.000000000000000000 ) ) ;
#47675 = VECTOR ( 'NONE', #21409, 39.37007874015748143 ) ;
#47676 = EDGE_CURVE ( 'NONE', #16462, #28931, #41366, .T. ) ;
#47677 = CARTESIAN_POINT ( 'NONE',  ( -2.734482843737247038, 1.205361022782829114E-17, -1.115254632218711794 ) ) ;
#47678 = COLOUR_RGB ( '',0.7921568627450980005, 0.8196078431372548767, 0.9333333333333333481 ) ;
#47679 = VERTEX_POINT ( 'NONE', #36992 ) ;
#47680 = ORIENTED_EDGE ( 'NONE', *, *, #48007, .F. ) ;
#47681 = CARTESIAN_POINT ( 'NONE',  ( -0.3929865681273516098, 1.607031701558540915, 2.441147462936593460 ) ) ;
#47682 = DIRECTION ( 'NONE',  ( 0.000000000000000000, 0.000000000000000000, -1.000000000000000000 ) ) ;
#47683 = DIRECTION ( 'NONE',  ( -0.01601477604151182663, 0.9998717552508123996, -0.000000000000000000 ) ) ;
#47684 = EDGE_CURVE ( 'NONE', #50578, #42803, #26123, .T. ) ;
#47685 = VECTOR ( 'NONE', #5771, 39.37007874015748143 ) ;
#47686 = DIRECTION ( 'NONE',  ( 0.9909497617679331460, 0.000000000000000000, 0.1342332658176667026 ) ) ;
#47687 = CARTESIAN_POINT ( 'NONE',  ( 0.000000000000000000, 3.267716535433071279, 0.9448818897637746295 ) ) ;
#47688 = LINE ( 'NONE', #16236, #20215 ) ;
#47689 = ORIENTED_EDGE ( 'NONE', *, *, #16987, .T. ) ;
#47690 = CARTESIAN_POINT ( 'NONE',  ( -1.636583440222564301, 0.000000000000000000, 1.377952755905504256 ) ) ;
#47691 = VERTEX_POINT ( 'NONE', #49322 ) ;
#47692 = LINE ( 'NONE', #20095, #18515 ) ;
#47693 = ORIENTED_EDGE ( 'NONE', *, *, #35506, .F. ) ;
#47694 = EDGE_CURVE ( 'NONE', #26125, #50486, #1864, .T. ) ;
#47695 = DIRECTION ( 'NONE',  ( -0.9749279121818259508, 0.000000000000000000, 0.2225209339563041788 ) ) ;
#47696 = CARTESIAN_POINT ( 'NONE',  ( 0.1155636338427008941, -0.5222242541845523167, 0.000000000000000000 ) ) ;
#47697 = CARTESIAN_POINT ( 'NONE',  ( 1.287906020515830141, 0.000000000000000000, 1.062992125984246083 ) ) ;
#47698 = CIRCLE ( 'NONE', #18088, 2.165354330708661568 ) ;
#47699 = VERTEX_POINT ( 'NONE', #49567 ) ;
#47700 = LINE ( 'NONE', #24512, #14221 ) ;
#47701 = CARTESIAN_POINT ( 'NONE',  ( -2.932638728931780125, 0.000000000000000000, 0.3475908556737795085 ) ) ;
#47702 = ORIENTED_EDGE ( 'NONE', *, *, #28917, .T. ) ;
#47703 = CARTESIAN_POINT ( 'NONE',  ( 0.8182917201112819283, 0.000000000000000000, 1.102362204724403938 ) ) ;
#47704 = ORIENTED_EDGE ( 'NONE', *, *, #27524, .F. ) ;
#47705 = VECTOR ( 'NONE', #14007, 39.37007874015748143 ) ;
#47706 = CARTESIAN_POINT ( 'NONE',  ( -2.074656761898998170, 0.000000000000000000, -0.6223516566630912239 ) ) ;
#47707 = CARTESIAN_POINT ( 'NONE',  ( 2.542761396444682465, 0.9856902423583451256, -0.6308468877598402136 ) ) ;
#47708 = VECTOR ( 'NONE', #41908, 39.37007874015748143 ) ;
#47709 = FACE_OUTER_BOUND ( 'NONE', #11519, .T. ) ;
#47710 = ORIENTED_EDGE ( 'NONE', *, *, #38571, .T. ) ;
#47712 = ORIENTED_EDGE ( 'NONE', *, *, #38554, .F. ) ;
#47711 = ADVANCED_FACE ( 'NONE', ( #33126 ), #25359, .F. ) ;
#47713 = DIRECTION ( 'NONE',  ( 1.000000000000000000, 0.000000000000000000, -3.469446951953613696E-16 ) ) ;
#47714 = DIRECTION ( 'NONE',  ( -0.000000000000000000, 1.000000000000000000, -0.000000000000000000 ) ) ;
#47715 = FACE_BOUND ( 'NONE', #42951, .T. ) ;
#47716 = CIRCLE ( 'NONE', #7379, 2.443628662382284489 ) ;
#47717 = ADVANCED_FACE ( 'NONE', ( #41118 ), #10122, .F. ) ;
#47718 = DIRECTION ( 'NONE',  ( 0.000000000000000000, 0.000000000000000000, -1.000000000000000000 ) ) ;
#47719 = LINE ( 'NONE', #12141, #5223 ) ;
#47720 = EDGE_CURVE ( 'NONE', #50839, #25457, #29489, .T. ) ;
#47721 = ADVANCED_FACE ( 'NONE', ( #37249 ), #17613, .F. ) ;
#47722 = ORIENTED_EDGE ( 'NONE', *, *, #6860, .F. ) ;
#47723 = LINE ( 'NONE', #16271, #39783 ) ;
#47724 = EDGE_LOOP ( 'NONE', ( #3275, #35793, #13378, #7391 ) ) ;
#47725 = ORIENTED_EDGE ( 'NONE', *, *, #21414, .T. ) ;
#47726 = PRODUCT_CONTEXT ( 'NONE', #5505, 'mechanical' ) ;
#47727 = VERTEX_POINT ( 'NONE', #22257 ) ;
#47728 = CARTESIAN_POINT ( 'NONE',  ( 0.000000000000000000, 0.000000000000000000, 0.000000000000000000 ) ) ;
#47729 = DIRECTION ( 'NONE',  ( 1.000000000000000000, 0.000000000000000000, 0.000000000000000000 ) ) ;
#47730 = ADVANCED_FACE ( 'NONE', ( #38010 ), #45209, .F. ) ;
#47731 = AXIS2_PLACEMENT_3D ( 'NONE', #2813, #42294, #10304 ) ;
#47732 = PLANE ( 'NONE',  #30844 ) ;
#47733 = DIRECTION ( 'NONE',  ( 0.000000000000000000, 0.000000000000000000, 1.000000000000000000 ) ) ;
#47734 = ORIENTED_EDGE ( 'NONE', *, *, #10542, .F. ) ;
#47735 = ORIENTED_EDGE ( 'NONE', *, *, #19328, .F. ) ;
#47736 = PLANE ( 'NONE',  #27401 ) ;
#47737 = DIRECTION ( 'NONE',  ( 2.866708903754509961E-17, 1.000000000000000000, -1.255987235303920130E-16 ) ) ;
#47738 = FACE_OUTER_BOUND ( 'NONE', #43618, .T. ) ;
#47739 = EDGE_CURVE ( 'NONE', #13466, #24511, #33383, .T. ) ;
#47740 = ORIENTED_EDGE ( 'NONE', *, *, #35215, .F. ) ;
#47741 = DIRECTION ( 'NONE',  ( -0.000000000000000000, 0.000000000000000000, 1.000000000000000000 ) ) ;
#47742 = LINE ( 'NONE', #36950, #25601 ) ;
#47743 = VECTOR ( 'NONE', #22509, 39.37007874015748143 ) ;
#47744 = CARTESIAN_POINT ( 'NONE',  ( 0.6872259521622784417, 0.000000000000000000, 1.878032350763792158 ) ) ;
#47745 = EDGE_CURVE ( 'NONE', #21072, #9746, #13749, .T. ) ;
#47746 = DIRECTION ( 'NONE',  ( -3.469446951953613696E-16, 0.000000000000000000, -1.000000000000000000 ) ) ;
#47747 = DIRECTION ( 'NONE',  ( 0.000000000000000000, -1.000000000000000000, 0.000000000000000000 ) ) ;
#47748 = ORIENTED_EDGE ( 'NONE', *, *, #50803, .T. ) ;
#47749 = DIRECTION ( 'NONE',  ( -0.000000000000000000, 1.000000000000000000, -0.000000000000000000 ) ) ;
#47750 = CARTESIAN_POINT ( 'NONE',  ( -1.263630850544466666, 0.000000000000000000, -1.276241334172347530 ) ) ;
#47751 = AXIS2_PLACEMENT_3D ( 'NONE', #14484, #30232, #42603 ) ;
#47752 = VERTEX_POINT ( 'NONE', #37504 ) ;
#47753 = EDGE_CURVE ( 'NONE', #31865, #8302, #50401, .T. ) ;
#47754 = VERTEX_POINT ( 'NONE', #33632 ) ;
#47755 = CARTESIAN_POINT ( 'NONE',  ( -0.6214413264104945434, 3.346456692913386100, -1.929133858267710000 ) ) ;
#47756 = CARTESIAN_POINT ( 'NONE',  ( 3.927031490892378253E-16, 3.346456692913386100, 1.377952755905504256 ) ) ;
#47757 = CARTESIAN_POINT ( 'NONE',  ( 2.019856298626497626, 1.049866565067837820, -0.1399740531529398979 ) ) ;
#47758 = ORIENTED_EDGE ( 'NONE', *, *, #43085, .T. ) ;
#47759 = EDGE_CURVE ( 'NONE', #23582, #16989, #28371, .T. ) ;
#47760 = ORIENTED_EDGE ( 'NONE', *, *, #1822, .T. ) ;
#47761 = CARTESIAN_POINT ( 'NONE',  ( 0.5469786881612729301, 0.03668053021573630668, -1.796948620166157307 ) ) ;
#47762 = EDGE_LOOP ( 'NONE', ( #33700, #50050, #27621, #46635 ) ) ;
#47763 = CARTESIAN_POINT ( 'NONE',  ( 2.695799277629594037, 1.453624836071520265, -1.205759334241453651 ) ) ;
#47764 = EDGE_LOOP ( 'NONE', ( #8180, #42913, #44141, #48417 ) ) ;
#47765 = EDGE_CURVE ( 'NONE', #21917, #34623, #17028, .T. ) ;
#47766 = CARTESIAN_POINT ( 'NONE',  ( -0.9149808212874269708, 1.594821661612501940, -2.013400720915880626 ) ) ;
#47767 = LINE ( 'NONE', #7555, #29681 ) ;
#47768 = FACE_OUTER_BOUND ( 'NONE', #41102, .T. ) ;
#47769 = AXIS2_PLACEMENT_3D ( 'NONE', #44521, #29552, #13808 ) ;
#47770 = ORIENTED_EDGE ( 'NONE', *, *, #13621, .T. ) ;
#47771 = ORIENTED_EDGE ( 'NONE', *, *, #6894, .T. ) ;
#47772 = EDGE_LOOP ( 'NONE', ( #21956, #13623, #48880, #46948 ) ) ;
#47773 = CARTESIAN_POINT ( 'NONE',  ( -0.5455278134075214336, 3.346456692913386100, -1.889763779527552146 ) ) ;
#47774 = VERTEX_POINT ( 'NONE', #32527 ) ;
#47775 = VERTEX_POINT ( 'NONE', #17283 ) ;
#47776 = CARTESIAN_POINT ( 'NONE',  ( -2.491402175429631605, 1.567214198537667302, -1.585592796919542025 ) ) ;
#47777 = FACE_OUTER_BOUND ( 'NONE', #31181, .T. ) ;
#47778 = DIRECTION ( 'NONE',  ( -1.000000000000000000, -0.000000000000000000, -0.000000000000000000 ) ) ;
#47779 = EDGE_CURVE ( 'NONE', #46840, #9567, #48820, .T. ) ;
#47780 = CIRCLE ( 'NONE', #37934, 2.165354330708661568 ) ;
#47781 = ORIENTED_EDGE ( 'NONE', *, *, #22337, .T. ) ;
#47782 = CIRCLE ( 'NONE', #1653, 2.164630168518208109 ) ;
#47783 = B_SPLINE_CURVE_WITH_KNOTS ( 'NONE', 3,
 ( #36559, #13577, #29829, #21323 ),
 .UNSPECIFIED., .F., .F.,
 ( 4, 4 ),
 ( 2.103951477127680371E-07, 0.01599021799251365214 ),
 .UNSPECIFIED. ) ;
#47784 = CARTESIAN_POINT ( 'NONE',  ( -0.07591351300297284610, 0.000000000000000000, 0.5905511811023582691 ) ) ;
#47785 = CARTESIAN_POINT ( 'NONE',  ( -0.7078551079828497850, 0.5249316497054297148, 1.746015920841205382 ) ) ;
#47786 = DIRECTION ( 'NONE',  ( -1.000000000000000000, 0.000000000000000000, 1.734723475976806848E-16 ) ) ;
#47787 = EDGE_CURVE ( 'NONE', #16143, #45509, #28885, .T. ) ;
#47788 = ORIENTED_EDGE ( 'NONE', *, *, #14983, .T. ) ;
#47789 = CYLINDRICAL_SURFACE ( 'NONE', #6773, 2.165354330708661568 ) ;
#47790 = DIRECTION ( 'NONE',  ( 1.734723475976806848E-16, -0.000000000000000000, 1.000000000000000000 ) ) ;
#47791 = EDGE_LOOP ( 'NONE', ( #16795, #13888, #39753, #37885 ) ) ;
#47792 = CARTESIAN_POINT ( 'NONE',  ( 0.000000000000000000, 3.346456692913386100, 0.000000000000000000 ) ) ;
#47793 = VERTEX_POINT ( 'NONE', #5658 ) ;
#47794 = ORIENTED_EDGE ( 'NONE', *, *, #47602, .T. ) ;
#47795 = VECTOR ( 'NONE', #47398, 39.37007874015748143 ) ;
#47796 = CARTESIAN_POINT ( 'NONE',  ( -1.439733046521776139, 0.000000000000000000, 0.9448818897637749625 ) ) ;
#47797 = DIRECTION ( 'NONE',  ( 1.241861098869884156E-16, 1.000000000000000000, 3.427318860986280993E-17 ) ) ;
#47798 = CARTESIAN_POINT ( 'NONE',  ( 1.833433833923351575, 3.267716535433071279, -6.361001426714000452E-16 ) ) ;
#47799 = CARTESIAN_POINT ( 'NONE',  ( -1.743268982565497449, 0.0004610889948519912205, -0.02902809809614041725 ) ) ;
#47800 = DIRECTION ( 'NONE',  ( 1.734723475976806848E-16, -0.000000000000000000, 1.000000000000000000 ) ) ;
#47801 = ORIENTED_EDGE ( 'NONE', *, *, #44598, .F. ) ;
#47802 = ORIENTED_EDGE ( 'NONE', *, *, #13961, .T. ) ;
#47803 = VERTEX_POINT ( 'NONE', #20886 ) ;
#47804 = DIRECTION ( 'NONE',  ( 0.000000000000000000, -1.000000000000000000, 0.000000000000000000 ) ) ;
#47805 = CARTESIAN_POINT ( 'NONE',  ( 1.363819533518803251, 0.000000000000000000, -0.4724409448818889246 ) ) ;
#47806 = B_SPLINE_CURVE_WITH_KNOTS ( 'NONE', 3,
 ( #41383, #24618, #24873, #20737 ),
 .UNSPECIFIED., .F., .F.,
 ( 4, 4 ),
 ( 0.01485121745614547892, 0.03075156861365398869 ),
 .UNSPECIFIED. ) ;
#47807 = EDGE_CURVE ( 'NONE', #39165, #47661, #33835, .T. ) ;
#47808 = CARTESIAN_POINT ( 'NONE',  ( -2.138597145901436125, 6.692913385826772199, 0.3393547186366932533 ) ) ;
#47809 = CARTESIAN_POINT ( 'NONE',  ( 2.928234753086226938, 1.764879838232207732, 0.3801023109259407673 ) ) ;
#47810 = DIRECTION ( 'NONE',  ( -0.7530714660036099684, 0.000000000000000000, -0.6579387259397138088 ) ) ;
#47811 = VERTEX_POINT ( 'NONE', #47958 ) ;
#47812 = CARTESIAN_POINT ( 'NONE',  ( 1.091055626815042645, 0.000000000000000000, -8.878505979408855953E-16 ) ) ;
#47813 = DIRECTION ( 'NONE',  ( -1.000000000000000000, 0.000000000000000000, 1.734723475976806848E-16 ) ) ;
#47814 = EDGE_CURVE ( 'NONE', #39003, #13966, #39940, .T. ) ;
#47815 = VECTOR ( 'NONE', #28152, 39.37007874015748143 ) ;
#47816 = ORIENTED_EDGE ( 'NONE', *, *, #17015, .F. ) ;
#47817 = CARTESIAN_POINT ( 'NONE',  ( 0.9794755770252105975, 0.5070346321433210068, 1.025452293874513199 ) ) ;
#47818 = VECTOR ( 'NONE', #38916, 39.37007874015748143 ) ;
#47819 = ADVANCED_FACE ( 'NONE', ( #37161 ), #1526, .F. ) ;
#47820 = CARTESIAN_POINT ( 'NONE',  ( -1.503492009532958695, 1.205361022782829114E-17, -0.9334790059352082725 ) ) ;
#47821 = CARTESIAN_POINT ( 'NONE',  ( 2.889674983507178219, 0.000000000000000000, -0.6090712660037610471 ) ) ;
#47823 = EDGE_CURVE ( 'NONE', #36525, #47095, #36647, .T. ) ;
#47822 = ORIENTED_EDGE ( 'NONE', *, *, #24811, .F. ) ;
#47824 = FACE_OUTER_BOUND ( 'NONE', #29845, .T. ) ;
#47825 = FACE_OUTER_BOUND ( 'NONE', #17775, .T. ) ;
#47826 = DIRECTION ( 'NONE',  ( 0.9998717552508121775, 0.01601477604151182663, 0.000000000000000000 ) ) ;
#47827 = ORIENTED_EDGE ( 'NONE', *, *, #17489, .F. ) ;
#47828 = DIRECTION ( 'NONE',  ( -0.000000000000000000, 0.000000000000000000, 1.000000000000000000 ) ) ;
#47829 = AXIS2_PLACEMENT_3D ( 'NONE', #11809, #43296, #11313 ) ;
#47830 = CARTESIAN_POINT ( 'NONE',  ( 0.2727639067037604947, 3.346456692913386100, 0.4724409448818868706 ) ) ;
#47831 = ORIENTED_EDGE ( 'NONE', *, *, #17337, .F. ) ;
#47832 = CARTESIAN_POINT ( 'NONE',  ( 1.091055626815042867, 3.267716535433071279, -1.892679809432645129E-16 ) ) ;
#47833 = DIRECTION ( 'NONE',  ( -1.000000000000000000, -0.000000000000000000, -0.000000000000000000 ) ) ;
#47834 = CARTESIAN_POINT ( 'NONE',  ( 0.000000000000000000, 3.267716535433071279, 2.007874015748021268 ) ) ;
#47835 = DIRECTION ( 'NONE',  ( -0.000000000000000000, 1.000000000000000000, -0.000000000000000000 ) ) ;
#47836 = ADVANCED_FACE ( 'NONE', ( #32785 ), #12631, .T. ) ;
#47837 = ORIENTED_EDGE ( 'NONE', *, *, #47094, .F. ) ;
#47838 = ORIENTED_EDGE ( 'NONE', *, *, #32950, .F. ) ;
#47839 = LINE ( 'NONE', #47068, #12481 ) ;
#47840 = CARTESIAN_POINT ( 'NONE',  ( 0.000000000000000000, 6.692913385826772199, 0.000000000000000000 ) ) ;
#47841 = EDGE_LOOP ( 'NONE', ( #39640, #2037, #22126, #8570 ) ) ;
#47842 = DIRECTION ( 'NONE',  ( 1.000000000000000000, 0.000000000000000000, -3.469446951953613696E-16 ) ) ;
#47843 = CARTESIAN_POINT ( 'NONE',  ( -0.9146000759343694275, 1.693252956796532871, -2.012610095043610769 ) ) ;
#47844 = CARTESIAN_POINT ( 'NONE',  ( -1.712496953225537188, 3.346456692913386100, 0.5905511811023582691 ) ) ;
#47845 = EDGE_CURVE ( 'NONE', #15979, #20171, #9527, .T. ) ;
#47846 = LINE ( 'NONE', #29024, #15756 ) ;
#47847 = EDGE_LOOP ( 'NONE', ( #25422, #45435, #28742, #42543 ) ) ;
#47848 = EDGE_LOOP ( 'NONE', ( #21821, #14520, #22994, #1281 ) ) ;
#47849 = FACE_OUTER_BOUND ( 'NONE', #1614, .T. ) ;
#47850 = DIRECTION ( 'NONE',  ( -0.9998717552508122886, -0.01601477604151182316, 0.000000000000000000 ) ) ;
#47851 = CARTESIAN_POINT ( 'NONE',  ( -1.062992125984251413, 0.5905511811023621549, 1.181102362204724088 ) ) ;
#47852 = EDGE_CURVE ( 'NONE', #23167, #8443, #24256, .T. ) ;
#47853 = B_SPLINE_CURVE_WITH_KNOTS ( 'NONE', 3,
 ( #20250, #32149, #35750, #40148 ),
 .UNSPECIFIED., .F., .F.,
 ( 4, 4 ),
 ( 2.103237516471686094E-07, 0.002500256604276755550 ),
 .UNSPECIFIED. ) ;
#47854 = EDGE_CURVE ( 'NONE', #22927, #13274, #47700, .T. ) ;
#47855 = DIRECTION ( 'NONE',  ( -1.000000000000000000, 0.000000000000000000, 1.734723475976806848E-16 ) ) ;
#47856 = FACE_BOUND ( 'NONE', #45910, .T. ) ;
#47857 = EDGE_LOOP ( 'NONE', ( #37874, #27272, #31320, #45324 ) ) ;
#47858 = CARTESIAN_POINT ( 'NONE',  ( -2.122503961981847542, 1.608289367666104752, -0.4339694865994201955 ) ) ;
#47859 = ORIENTED_EDGE ( 'NONE', *, *, #1032, .F. ) ;
#47860 = ORIENTED_EDGE ( 'NONE', *, *, #30120, .T. ) ;
#47861 = CARTESIAN_POINT ( 'NONE',  ( 0.8182917201112819283, 0.000000000000000000, -0.9842519685039348154 ) ) ;
#47862 = VECTOR ( 'NONE', #33270, 39.37007874015748143 ) ;
#47863 = VERTEX_POINT ( 'NONE', #24768 ) ;
#47864 = ORIENTED_EDGE ( 'NONE', *, *, #1120, .F. ) ;
#47865 = DIRECTION ( 'NONE',  ( 0.01601477604151182663, -0.9998717552508123996, 0.000000000000000000 ) ) ;
#47866 = ORIENTED_EDGE ( 'NONE', *, *, #14896, .F. ) ;
#47867 = VECTOR ( 'NONE', #27807, 39.37007874015748143 ) ;
#47868 = DIRECTION ( 'NONE',  ( -0.7227948638273978821, 0.000000000000000000, 0.6910626489868580968 ) ) ;
#47869 = LINE ( 'NONE', #47101, #3825 ) ;
#47870 = CARTESIAN_POINT ( 'NONE',  ( -1.999177773607318409, 1.049866565067837820, 0.3204690814597923043 ) ) ;
#47871 = VECTOR ( 'NONE', #2779, 39.37007874015748143 ) ;
#47872 = DIRECTION ( 'NONE',  ( -1.000000000000000000, 0.000000000000000000, 1.734723475976806848E-16 ) ) ;
#47873 = DIRECTION ( 'NONE',  ( -0.01601477604151182663, 0.9998717552508123996, -0.000000000000000000 ) ) ;
#47874 = LINE ( 'NONE', #8677, #48425 ) ;
#47875 = EDGE_LOOP ( 'NONE', ( #23359, #4366, #43280, #8251 ) ) ;
#47876 = CARTESIAN_POINT ( 'NONE',  ( -0.07591351300297362326, 3.346456692913386100, -2.104930761696520491 ) ) ;
#47877 = DIRECTION ( 'NONE',  ( 9.964307797194585150E-17, -1.000000000000000000, 5.953396763000637613E-17 ) ) ;
#47878 = DIRECTION ( 'NONE',  ( -0.7071067811865483499, -2.200518442539857142E-16, 0.7071067811865465735 ) ) ;
#47879 = ORIENTED_EDGE ( 'NONE', *, *, #22853, .F. ) ;
#47880 = CARTESIAN_POINT ( 'NONE',  ( -1.181102362204724310, 0.5905511811023621549, -1.062992125984252079 ) ) ;
#47881 = EDGE_CURVE ( 'NONE', #36096, #32442, #12372, .T. ) ;
#47882 = CARTESIAN_POINT ( 'NONE',  ( 1.909347346926324684, 3.346456692913386100, -0.4724409448818889246 ) ) ;
#47883 = ORIENTED_EDGE ( 'NONE', *, *, #24329, .F. ) ;
#47884 = DIRECTION ( 'NONE',  ( 0.000000000000000000, 0.000000000000000000, -1.000000000000000000 ) ) ;
#47885 = DIRECTION ( 'NONE',  ( 1.000000000000000000, 0.000000000000000000, 0.000000000000000000 ) ) ;
#47886 = EDGE_CURVE ( 'NONE', #35873, #39853, #43853, .T. ) ;
#47887 = CARTESIAN_POINT ( 'NONE',  ( -1.722315009966508548, 1.593974433676846880, -2.398471918813898984 ) ) ;
#47888 = VERTEX_POINT ( 'NONE', #20376 ) ;
#47889 = CARTESIAN_POINT ( 'NONE',  ( 2.021817418930639931, 3.346456692913386100, 0.5905511811023582691 ) ) ;
#47890 = VERTEX_POINT ( 'NONE', #4888 ) ;
#47891 = CARTESIAN_POINT ( 'NONE',  ( 0.07982360342473591996, 1.709180471932028711, 0.000000000000000000 ) ) ;
#47892 = CARTESIAN_POINT ( 'NONE',  ( 1.367759369798452695, 0.5227967160397331003, -1.798833794882606085 ) ) ;
#47893 = AXIS2_PLACEMENT_3D ( 'NONE', #46311, #46558, #11225 ) ;
#47894 = EDGE_CURVE ( 'NONE', #15197, #10377, #36132, .T. ) ;
#47895 = AXIS2_PLACEMENT_3D ( 'NONE', #36797, #47855, #40667 ) ;
#47896 = CARTESIAN_POINT ( 'NONE',  ( -0.9794755770252102645, 0.5070346321433212289, 1.132746185074374460E-16 ) ) ;
#47897 = LINE ( 'NONE', #42220, #44140 ) ;
#47898 = VECTOR ( 'NONE', #14292, 39.37007874015748143 ) ;
#47899 = ORIENTED_EDGE ( 'NONE', *, *, #16782, .F. ) ;
#47900 = ORIENTED_EDGE ( 'NONE', *, *, #44280, .T. ) ;
#47901 = LINE ( 'NONE', #8197, #50092 ) ;
#47902 = ORIENTED_EDGE ( 'NONE', *, *, #35809, .T. ) ;
#47903 = AXIS2_PLACEMENT_3D ( 'NONE', #32931, #48612, #48103 ) ;
#47904 = EDGE_CURVE ( 'NONE', #47658, #13697, #20632, .T. ) ;
#47905 = DIRECTION ( 'NONE',  ( -0.01601477604151182663, 0.9998717552508123996, -0.000000000000000000 ) ) ;
#47906 = EDGE_LOOP ( 'NONE', ( #43065, #30704, #34699, #34946 ) ) ;
#47907 = DIRECTION ( 'NONE',  ( -0.000000000000000000, 1.000000000000000000, -0.000000000000000000 ) ) ;
#47908 = VECTOR ( 'NONE', #30347, 39.37007874015748143 ) ;
#47909 = EDGE_CURVE ( 'NONE', #8496, #23557, #21916, .T. ) ;
#47910 = ORIENTED_EDGE ( 'NONE', *, *, #36603, .T. ) ;
#47911 = DIRECTION ( 'NONE',  ( -0.7530714660036099684, 0.000000000000000000, -0.6579387259397138088 ) ) ;
#47912 = ADVANCED_FACE ( 'NONE', ( #26291 ), #37673, .F. ) ;
#47913 = CARTESIAN_POINT ( 'NONE',  ( 0.9794755770252103755, 0.4349011127721511549, -1.097585813245683495 ) ) ;
#47914 = ORIENTED_EDGE ( 'NONE', *, *, #41888, .F. ) ;
#47915 = EDGE_CURVE ( 'NONE', #33190, #40666, #29399, .T. ) ;
#47916 = CARTESIAN_POINT ( 'NONE',  ( -1.166969139818015977, 3.267716535433071279, -1.753476375576570323 ) ) ;
#47917 = EDGE_LOOP ( 'NONE', ( #41674, #23470, #38057, #27018 ) ) ;
#47918 = EDGE_CURVE ( 'NONE', #29725, #20465, #37415, .T. ) ;
#47919 = CARTESIAN_POINT ( 'NONE',  ( 1.287906020515830141, 3.267716535433071279, -1.141732283464564013 ) ) ;
#47920 = ORIENTED_EDGE ( 'NONE', *, *, #32632, .F. ) ;
#47921 = EDGE_LOOP ( 'NONE', ( #9645, #957, #522, #7039 ) ) ;
#47922 = B_SPLINE_CURVE_WITH_KNOTS ( 'NONE', 3,
 ( #30038, #34921, #46755, #45757 ),
 .UNSPECIFIED., .F., .F.,
 ( 4, 4 ),
 ( 6.553284148700209415E-07, 0.004847467262264384957 ),
 .UNSPECIFIED. ) ;
#47923 = LINE ( 'NONE', #40228, #5996 ) ;
#47924 = CARTESIAN_POINT ( 'NONE',  ( 0.4696143004045484903, 0.000000000000000000, 1.732283464566921172 ) ) ;
#47925 = VERTEX_POINT ( 'NONE', #42281 ) ;
#47926 = DIRECTION ( 'NONE',  ( 1.000000000000000000, 0.000000000000000000, 0.000000000000000000 ) ) ;
#47927 = ORIENTED_EDGE ( 'NONE', *, *, #11287, .T. ) ;
#47928 = LINE ( 'NONE', #729, #39266 ) ;
#47929 = AXIS2_PLACEMENT_3D ( 'NONE', #11160, #25892, #10662 ) ;
#47930 = CARTESIAN_POINT ( 'NONE',  ( -1.909347346926324462, 0.000000000000000000, 0.1574803149606286423 ) ) ;
#47931 = AXIS2_PLACEMENT_3D ( 'NONE', #22502, #10378, #25608 ) ;
#47932 = FACE_OUTER_BOUND ( 'NONE', #48891, .T. ) ;
#47933 = ORIENTED_EDGE ( 'NONE', *, *, #4174, .F. ) ;
#47934 = ORIENTED_EDGE ( 'NONE', *, *, #38236, .F. ) ;
#47935 = VECTOR ( 'NONE', #33302, 39.37007874015748143 ) ;
#47936 = CARTESIAN_POINT ( 'NONE',  ( -1.387661672111457634, 5.905511811023623991, -1.663104731517941470 ) ) ;
#47937 = LINE ( 'NONE', #16490, #32789 ) ;
#47938 = DIRECTION ( 'NONE',  ( -0.000000000000000000, 1.000000000000000000, -0.000000000000000000 ) ) ;
#47939 = CARTESIAN_POINT ( 'NONE',  ( 1.909347346926324684, 3.267716535433071279, 0.7874015748031456541 ) ) ;
#47940 = AXIS2_PLACEMENT_3D ( 'NONE', #28643, #44389, #24782 ) ;
#47941 = CARTESIAN_POINT ( 'NONE',  ( -0.6214413264104945434, 0.000000000000000000, 0.1574803149606285035 ) ) ;
#47942 = CARTESIAN_POINT ( 'NONE',  ( -1.636583440222564301, 3.346456692913386100, -0.5118110236220466680 ) ) ;
#47943 = VECTOR ( 'NONE', #8298, 39.37007874015748143 ) ;
#47944 = DIRECTION ( 'NONE',  ( -0.8439299085898971375, -0.000000000000000000, 0.5364534550056020423 ) ) ;
#47945 = EDGE_LOOP ( 'NONE', ( #8206, #26119, #3872, #24279, #28159, #16573 ) ) ;
#47946 = LINE ( 'NONE', #28871, #28399 ) ;
#47947 = EDGE_CURVE ( 'NONE', #39823, #286, #1875, .T. ) ;
#47948 = ORIENTED_EDGE ( 'NONE', *, *, #29109, .T. ) ;
#47949 = LINE ( 'NONE', #28100, #29229 ) ;
#47950 = ADVANCED_FACE ( 'NONE', ( #30164 ), #955, .T. ) ;
#47951 = ORIENTED_EDGE ( 'NONE', *, *, #1922, .T. ) ;
#47952 = EDGE_CURVE ( 'NONE', #49218, #25289, #2038, .T. ) ;
#47953 = DIRECTION ( 'NONE',  ( -0.000000000000000000, 0.000000000000000000, 1.000000000000000000 ) ) ;
#47954 = CARTESIAN_POINT ( 'NONE',  ( 0.000000000000000000, 3.346456692913386100, 0.000000000000000000 ) ) ;
#47955 = CARTESIAN_POINT ( 'NONE',  ( 2.755905511811024056, 4.960629921259846142, -1.023622047244094224 ) ) ;
#47956 = CARTESIAN_POINT ( 'NONE',  ( 0.2483287796717625062, 1.509167455152593096, -2.942340884688746883 ) ) ;
#47957 = VERTEX_POINT ( 'NONE', #33802 ) ;
#47958 = CARTESIAN_POINT ( 'NONE',  ( 0.5455278134075216556, 3.346456692913386100, 2.007874015748021268 ) ) ;
#47959 = FACE_BOUND ( 'NONE', #6253, .T. ) ;
#47960 = EDGE_LOOP ( 'NONE', ( #3920, #34631, #16604, #5796 ) ) ;
#47961 = LINE ( 'NONE', #1529, #6488 ) ;
#47962 = ORIENTED_EDGE ( 'NONE', *, *, #21126, .F. ) ;
#47963 = LINE ( 'NONE', #43351, #12864 ) ;
#47964 = FACE_OUTER_BOUND ( 'NONE', #37822, .T. ) ;
#47965 = AXIS2_PLACEMENT_3D ( 'NONE', #29936, #41058, #17305 ) ;
#47966 = EDGE_CURVE ( 'NONE', #11883, #21408, #30423, .T. ) ;
#47967 = AXIS2_PLACEMENT_3D ( 'NONE', #7636, #50191, #30624 ) ;
#47968 = CARTESIAN_POINT ( 'NONE',  ( -1.195183497228115035E-16, 3.267716535433071279, 0.3149606299212576177 ) ) ;
#47969 = ORIENTED_EDGE ( 'NONE', *, *, #5253, .T. ) ;
#47970 = VERTEX_POINT ( 'NONE', #37923 ) ;
#47971 = ADVANCED_FACE ( 'NONE', ( #6672 ), #5906, .F. ) ;
#47972 = FACE_OUTER_BOUND ( 'NONE', #13794, .T. ) ;
#47974 = CARTESIAN_POINT ( 'NONE',  ( 1.636583440222563635, 3.267716535433071279, -2.839019714148966584E-16 ) ) ;
#47973 = VECTOR ( 'NONE', #41187, 39.37007874015748143 ) ;
#47975 = DIRECTION ( 'NONE',  ( 0.000000000000000000, -1.000000000000000000, 0.000000000000000000 ) ) ;
#47976 = VECTOR ( 'NONE', #6027, 39.37007874015748143 ) ;
#47977 = LINE ( 'NONE', #16009, #35266 ) ;
#47978 = CARTESIAN_POINT ( 'NONE',  ( 0.000000000000000000, 1.574803149606302854, 0.000000000000000000 ) ) ;
#47979 = VERTEX_POINT ( 'NONE', #22423 ) ;
#47980 = CARTESIAN_POINT ( 'NONE',  ( -1.636583440222564301, 3.346456692913386100, -0.9448818897637762948 ) ) ;
#47981 = ORIENTED_EDGE ( 'NONE', *, *, #22604, .T. ) ;
#47982 = ORIENTED_EDGE ( 'NONE', *, *, #36510, .F. ) ;
#47983 = ITEM_DEFINED_TRANSFORMATION ( 'NONE', 'NONE', #29206,  #26741 ) ;
#47984 = EDGE_CURVE ( 'NONE', #30956, #22242, #29662, .T. ) ;
#47985 = ORIENTED_EDGE ( 'NONE', *, *, #6556, .T. ) ;
#47986 = DIRECTION ( 'NONE',  ( -0.01601477604151182663, 0.9998717552508123996, -0.000000000000000000 ) ) ;
#47987 = CARTESIAN_POINT ( 'NONE',  ( 0.2156353639037333347, 0.03137346048107473445, -1.846898229409209558 ) ) ;
#47988 = DIRECTION ( 'NONE',  ( -0.000000000000000000, 0.000000000000000000, 1.000000000000000000 ) ) ;
#47989 = PLANE ( 'NONE',  #23062 ) ;
#47990 = ORIENTED_EDGE ( 'NONE', *, *, #26546, .F. ) ;
#47991 = ORIENTED_EDGE ( 'NONE', *, *, #29670, .F. ) ;
#47992 = DIRECTION ( 'NONE',  ( -0.5877852522924684742, 0.000000000000000000, -0.8090169943749506709 ) ) ;
#47993 = CARTESIAN_POINT ( 'NONE',  ( 1.128560816269277955, 1.725977917706353670, 1.984842472008916170 ) ) ;
#47994 = FACE_OUTER_BOUND ( 'NONE', #13042, .T. ) ;
#47995 = CARTESIAN_POINT ( 'NONE',  ( -0.07591351300297277671, 3.346456692913386100, 1.102362204724404160 ) ) ;
#47996 = CARTESIAN_POINT ( 'NONE',  ( -2.160407304981126320, 1.673304745347873324, -0.1462862061266896330 ) ) ;
#47997 = CARTESIAN_POINT ( 'NONE',  ( -0.5455278134075214336, 3.267716535433071279, -0.8267716535433049518 ) ) ;
#47998 = CARTESIAN_POINT ( 'NONE',  ( 1.859752236076028797, 0.5249316497054297148, 0.3015826091447992297 ) ) ;
#47999 = CARTESIAN_POINT ( 'NONE',  ( -0.2727639067037610499, 0.000000000000000000, -2.047244094488181343 ) ) ;
#48000 = AXIS2_PLACEMENT_3D ( 'NONE', #13483, #21740, #13235 ) ;
#48001 = ORIENTED_EDGE ( 'NONE', *, *, #49581, .T. ) ;
#48002 = PLANE ( 'NONE',  #30009 ) ;
#48003 = DIRECTION ( 'NONE',  ( -0.000000000000000000, 1.000000000000000000, 0.000000000000000000 ) ) ;
#48004 = EDGE_CURVE ( 'NONE', #33562, #21655, #41529, .T. ) ;
#48005 = VECTOR ( 'NONE', #12894, 39.37007874015748143 ) ;
#48006 = ORIENTED_EDGE ( 'NONE', *, *, #26409, .F. ) ;
#48007 = EDGE_CURVE ( 'NONE', #11192, #44848, #7544, .T. ) ;
#48008 = VECTOR ( 'NONE', #40620, 39.37007874015748143 ) ;
#48009 = ORIENTED_EDGE ( 'NONE', *, *, #8430, .F. ) ;
#48010 = VECTOR ( 'NONE', #10587, 39.37007874015748143 ) ;
#48011 = CARTESIAN_POINT ( 'NONE',  ( 0.5455278134075212115, 3.346456692913386100, -6.146657985744592735E-16 ) ) ;
#48012 = DIRECTION ( 'NONE',  ( 1.734723475976806848E-16, 0.000000000000000000, 1.000000000000000000 ) ) ;
#48013 = CARTESIAN_POINT ( 'NONE',  ( -1.985260859929298238, 3.267716535433071279, -1.141732283464563791 ) ) ;
#48014 = EDGE_CURVE ( 'NONE', #50795, #7249, #16623, .T. ) ;
#48015 = ORIENTED_EDGE ( 'NONE', *, *, #31555, .T. ) ;
#48016 = EDGE_CURVE ( 'NONE', #31313, #27397, #49989, .T. ) ;
#48017 = VECTOR ( 'NONE', #36564, 39.37007874015748143 ) ;
#48018 = ORIENTED_EDGE ( 'NONE', *, *, #42582, .F. ) ;
#48019 = PLANE ( 'NONE',  #38627 ) ;
#48020 = EDGE_LOOP ( 'NONE', ( #47900, #45768, #40603, #13625 ) ) ;
#48021 = LINE ( 'NONE', #25528, #18007 ) ;
#48022 = ORIENTED_EDGE ( 'NONE', *, *, #1265, .F. ) ;
#48023 = CARTESIAN_POINT ( 'NONE',  ( 0.9116672196811488327, 1.631344156046437899, 2.569185889370713127 ) ) ;
#48024 = FACE_OUTER_BOUND ( 'NONE', #38804, .T. ) ;
#48025 = CARTESIAN_POINT ( 'NONE',  ( 2.378961647330872342, 3.267716535433071279, -8.253681236146642869E-16 ) ) ;
#48026 = EDGE_CURVE ( 'NONE', #14385, #5048, #18039, .T. ) ;
#48027 = ORIENTED_EDGE ( 'NONE', *, *, #19177, .F. ) ;
#48028 = ORIENTED_EDGE ( 'NONE', *, *, #37437, .F. ) ;
#48029 = ORIENTED_EDGE ( 'NONE', *, *, #8071, .F. ) ;
#48030 = LINE ( 'NONE', #41349, #4081 ) ;
#48031 = EDGE_LOOP ( 'NONE', ( #10907, #50851, #44316, #2235 ) ) ;
#48032 = ORIENTED_EDGE ( 'NONE', *, *, #5898, .T. ) ;
#48033 = ADVANCED_FACE ( 'NONE', ( #33288 ), #18291, .F. ) ;
#48034 = CARTESIAN_POINT ( 'NONE',  ( -1.363819533518803473, 0.000000000000000000, -0.6692913385826760875 ) ) ;
#48035 = CARTESIAN_POINT ( 'NONE',  ( -0.07591351300297333182, 0.000000000000000000, -0.7874015748031470974 ) ) ;
#48036 = CARTESIAN_POINT ( 'NONE',  ( 2.109782028357643835, 1.650152804904060133, 1.745440299926597882 ) ) ;
#48037 = ORIENTED_EDGE ( 'NONE', *, *, #47514, .T. ) ;
#48038 = CARTESIAN_POINT ( 'NONE',  ( -2.454875160333845674, 0.000000000000000000, 0.1574803149606286423 ) ) ;
#48039 = CARTESIAN_POINT ( 'NONE',  ( 0.4696143004045478797, 0.000000000000000000, 0.5905511811023579360 ) ) ;
#48040 = EDGE_CURVE ( 'NONE', #23689, #19826, #25526, .T. ) ;
#48041 = DIRECTION ( 'NONE',  ( -0.01601477604151182663, 0.9998717552508123996, -0.000000000000000000 ) ) ;
#48042 = ORIENTED_EDGE ( 'NONE', *, *, #17572, .F. ) ;
#48043 = CARTESIAN_POINT ( 'NONE',  ( 0.9218113296639885990, 0.000000000000000000, -1.800737481590852118 ) ) ;
#48044 = AXIS2_PLACEMENT_3D ( 'NONE', #8006, #39508, #19868 ) ;
#48045 = CARTESIAN_POINT ( 'NONE',  ( -0.6214413264104945434, 0.000000000000000000, -1.417322834645664331 ) ) ;
#48046 = ORIENTED_EDGE ( 'NONE', *, *, #20900, .F. ) ;
#48047 = DIRECTION ( 'NONE',  ( -1.000000000000000000, 0.000000000000000000, -0.000000000000000000 ) ) ;
#48048 = ORIENTED_EDGE ( 'NONE', *, *, #4852, .F. ) ;
#48049 = VECTOR ( 'NONE', #16700, 39.37007874015748143 ) ;
#48050 = VERTEX_POINT ( 'NONE', #19486 ) ;
#48051 = DIRECTION ( 'NONE',  ( -3.469446951953613696E-16, 0.000000000000000000, -1.000000000000000000 ) ) ;
#48052 =( LENGTH_UNIT ( ) NAMED_UNIT ( * ) SI_UNIT ( $, .METRE. ) );
#48053 = ADVANCED_FACE ( 'NONE', ( #10490 ), #46084, .F. ) ;
#48054 = AXIS2_PLACEMENT_3D ( 'NONE', #27126, #19129, #50821 ) ;
#48055 = CIRCLE ( 'NONE', #11783, 2.246510896728926010 ) ;
#48056 = FACE_OUTER_BOUND ( 'NONE', #18995, .T. ) ;
#48057 = CARTESIAN_POINT ( 'NONE',  ( 0.3543214468173200293, 1.713577057256821190, 2.228085083314873316 ) ) ;
#48058 = CARTESIAN_POINT ( 'NONE',  ( -0.6214413264104939882, 3.267716535433071279, 1.732283464566921172 ) ) ;
#48059 = ORIENTED_EDGE ( 'NONE', *, *, #20163, .T. ) ;
#48060 = ORIENTED_EDGE ( 'NONE', *, *, #32370, .T. ) ;
#48061 = AXIS2_PLACEMENT_3D ( 'NONE', #24108, #39854, #95 ) ;
#48062 = EDGE_CURVE ( 'NONE', #39173, #36517, #27231, .T. ) ;
#48063 = CARTESIAN_POINT ( 'NONE',  ( 0.000000000000000000, 6.692913385826772199, 0.000000000000000000 ) ) ;
#48064 = ORIENTED_EDGE ( 'NONE', *, *, #8722, .T. ) ;
#48065 = CARTESIAN_POINT ( 'NONE',  ( -1.521361932310741016, 3.346456692913386100, -1.456692913385822186 ) ) ;
#48066 = CARTESIAN_POINT ( 'NONE',  ( 1.905671854841464175, 0.000000000000000000, 2.256015092822681645 ) ) ;
#48067 = CARTESIAN_POINT ( 'NONE',  ( 2.919426793319799707, 1.666276233232717896, 0.4451252810446822417 ) ) ;
#48068 = DIRECTION ( 'NONE',  ( 1.734723475976806848E-16, -0.000000000000000000, 1.000000000000000000 ) ) ;
#48069 = DIRECTION ( 'NONE',  ( -0.000000000000000000, 1.000000000000000000, -0.000000000000000000 ) ) ;
#48070 = ORIENTED_EDGE ( 'NONE', *, *, #2507, .T. ) ;
#48071 = DIRECTION ( 'NONE',  ( 1.000000000000000000, 0.000000000000000000, 0.000000000000000000 ) ) ;
#48072 = CARTESIAN_POINT ( 'NONE',  ( -1.083598637574820112, 0.000000000000000000, 2.747180975113330259 ) ) ;
#48073 = EDGE_CURVE ( 'NONE', #8409, #13544, #19234, .T. ) ;
#48074 = VERTEX_POINT ( 'NONE', #38122 ) ;
#48075 = CARTESIAN_POINT ( 'NONE',  ( -2.071704270381554913, 3.346456692913386100, 0.6299212598425164567 ) ) ;
#48076 = DIRECTION ( 'NONE',  ( 0.5128992774058948045, 0.000000000000000000, 0.8584487936018727616 ) ) ;
#48077 = CARTESIAN_POINT ( 'NONE',  ( 1.091055626815042645, 3.346456692913386100, 0.4330708661417287386 ) ) ;
#48078 = ORIENTED_EDGE ( 'NONE', *, *, #7973, .F. ) ;
#48079 = CARTESIAN_POINT ( 'NONE',  ( 0.000000000000000000, 3.267716535433071279, -1.456692913385822630 ) ) ;
#48080 = PLANE ( 'NONE',  #19224 ) ;
#48081 = EDGE_CURVE ( 'NONE', #41856, #38999, #2360, .T. ) ;
#48082 = CARTESIAN_POINT ( 'NONE',  ( -0.2156685157583831947, 1.617455082123532062, -2.945280361644576850 ) ) ;
#48083 = AXIS2_PLACEMENT_3D ( 'NONE', #9037, #46846, #18065 ) ;
#48084 = ORIENTED_EDGE ( 'NONE', *, *, #24329, .T. ) ;
#48085 = DIRECTION ( 'NONE',  ( 1.000000000000000000, 0.000000000000000000, 0.000000000000000000 ) ) ;
#48086 = CARTESIAN_POINT ( 'NONE',  ( -1.759095177137641075, 1.049866565067838264, 1.002495067533146988 ) ) ;
#48087 = VERTEX_POINT ( 'NONE', #26477 ) ;
#48088 = DIRECTION ( 'NONE',  ( 0.8805955318567391110, 0.000000000000000000, -0.4738686624729965269 ) ) ;
#48089 = CIRCLE ( 'NONE', #3606, 2.246510896728926010 ) ;
#48090 = CIRCLE ( 'NONE', #25024, 2.493791675044291445 ) ;
#48091 = CARTESIAN_POINT ( 'NONE',  ( -2.182111253630085290, 3.346456692913386100, -6.146657985744592735E-16 ) ) ;
#48092 = CARTESIAN_POINT ( 'NONE',  ( -1.091055626815042645, 0.000000000000000000, -0.5118110236220467790 ) ) ;
#48093 = CARTESIAN_POINT ( 'NONE',  ( -0.8783128861146038968, 0.01385187720497466773, 1.565997986929510644 ) ) ;
#48094 = VERTEX_POINT ( 'NONE', #50181 ) ;
#48095 = EDGE_LOOP ( 'NONE', ( #17909, #37, #47423, #47481 ) ) ;
#48096 = CARTESIAN_POINT ( 'NONE',  ( -1.695772546416002280, 0.000000000000000000, -2.417756147381373566 ) ) ;
#48097 = VECTOR ( 'NONE', #30216, 39.37007874015748143 ) ;
#48098 = DIRECTION ( 'NONE',  ( -3.469446951953613696E-16, 0.000000000000000000, -1.000000000000000000 ) ) ;
#48099 = ORIENTED_EDGE ( 'NONE', *, *, #1076, .F. ) ;
#48100 = CARTESIAN_POINT ( 'NONE',  ( 1.015142113812069313, 3.346456692913386100, 0.1574803149606286423 ) ) ;
#48101 = DIRECTION ( 'NONE',  ( -0.000000000000000000, 1.000000000000000000, -0.000000000000000000 ) ) ;
#48102 = DIRECTION ( 'NONE',  ( -1.156061316345074457E-16, -1.000000000000000000, 1.040474016969491568E-17 ) ) ;
#48103 = DIRECTION ( 'NONE',  ( 1.734723475976806848E-16, 0.000000000000000000, 1.000000000000000000 ) ) ;
#48104 = VERTEX_POINT ( 'NONE', #30366 ) ;
#48105 = ORIENTED_EDGE ( 'NONE', *, *, #34919, .F. ) ;
#48106 = CARTESIAN_POINT ( 'NONE',  ( -1.985260859929297572, 0.000000000000000000, 0.3149606299212578953 ) ) ;
#48107 = CARTESIAN_POINT ( 'NONE',  ( 0.000000000000000000, 3.267716535433071279, 1.377952755905504256 ) ) ;
#48108 = EDGE_CURVE ( 'NONE', #41853, #22384, #16534, .T. ) ;
#48109 = CARTESIAN_POINT ( 'NONE',  ( -0.7697430959579070198, 1.531135861556976119, -2.850707213328497858 ) ) ;
#48110 = CARTESIAN_POINT ( 'NONE',  ( 0.000000000000000000, 5.118110236220475784, 0.000000000000000000 ) ) ;
#48111 = FACE_BOUND ( 'NONE', #14769, .T. ) ;
#48112 = EDGE_LOOP ( 'NONE', ( #9457, #44163, #23188, #20200 ) ) ;
#48113 = DIRECTION ( 'NONE',  ( -0.01601477604151182663, 0.9998717552508123996, -0.000000000000000000 ) ) ;
#48114 = ORIENTED_EDGE ( 'NONE', *, *, #30239, .F. ) ;
#48115 = ORIENTED_EDGE ( 'NONE', *, *, #44908, .F. ) ;
#48116 = DIRECTION ( 'NONE',  ( 0.000000000000000000, 0.000000000000000000, -1.000000000000000000 ) ) ;
#48117 = EDGE_CURVE ( 'NONE', #19314, #18704, #11500, .T. ) ;
#48118 = EDGE_CURVE ( 'NONE', #19367, #11567, #34496, .T. ) ;
#48119 = EDGE_CURVE ( 'NONE', #46309, #40889, #41774, .T. ) ;
#48120 = EDGE_LOOP ( 'NONE', ( #17992, #30374, #38214, #8109 ) ) ;
#48121 = ORIENTED_EDGE ( 'NONE', *, *, #27070, .F. ) ;
#48122 = LINE ( 'NONE', #20799, #36832 ) ;
#48123 = ORIENTED_EDGE ( 'NONE', *, *, #18385, .T. ) ;
#48124 = VECTOR ( 'NONE', #25816, 39.37007874015748143 ) ;
#48125 = EDGE_CURVE ( 'NONE', #9419, #10330, #6867, .T. ) ;
#48126 = AXIS2_PLACEMENT_3D ( 'NONE', #41725, #10228, #14355 ) ;
#48127 = CARTESIAN_POINT ( 'NONE',  ( -2.151809081513409438, 1.673437530708463017, 0.2418202932658340965 ) ) ;
#48128 = CARTESIAN_POINT ( 'NONE',  ( 0.000000000000000000, 1.574803149606302854, 0.000000000000000000 ) ) ;
#48129 = CARTESIAN_POINT ( 'NONE',  ( -0.8221900955658373311, 6.692913385826772199, 2.050660405798877317 ) ) ;
#48130 = CONICAL_SURFACE ( 'NONE', #39097, 2.246510896728926010, 0.01601546068027819014 ) ;
#48131 = ADVANCED_FACE ( 'NONE', ( #18490 ), #38367, .F. ) ;
#48132 = VECTOR ( 'NONE', #13201, 39.37007874015748143 ) ;
#48133 = CARTESIAN_POINT ( 'NONE',  ( 1.363819533518803251, 0.000000000000000000, -0.7874015748031473194 ) ) ;
#48134 = DIRECTION ( 'NONE',  ( -0.000000000000000000, 1.000000000000000000, -0.000000000000000000 ) ) ;
#48135 = CARTESIAN_POINT ( 'NONE',  ( 0.04921259842519667277, 1.675881784547888831, 2.245244178460735540 ) ) ;
#48136 = VECTOR ( 'NONE', #46316, 39.37007874015748143 ) ;
#48137 = ORIENTED_EDGE ( 'NONE', *, *, #36250, .F. ) ;
#48138 = CARTESIAN_POINT ( 'NONE',  ( 0.5756566573088583993, 1.502670515430445386, 2.896516654582643291 ) ) ;
#48139 = CARTESIAN_POINT ( 'NONE',  ( 0.8182917201112817063, 3.346456692913386100, -1.929133858267711110 ) ) ;
#48140 = CARTESIAN_POINT ( 'NONE',  ( -1.166969139818016199, 3.346456692913386100, 1.535433070866133232 ) ) ;
#48141 = EDGE_CURVE ( 'NONE', #33328, #11080, #15623, .T. ) ;
#48142 = EDGE_LOOP ( 'NONE', ( #39689, #48724, #8587, #24915 ) ) ;
#48143 = CARTESIAN_POINT ( 'NONE',  ( -0.1071992566810134884, 0.000000000000000000, -1.740088185897663342 ) ) ;
#48144 = DIRECTION ( 'NONE',  ( 1.000000000000000000, 0.000000000000000000, 0.000000000000000000 ) ) ;
#48145 = EDGE_LOOP ( 'NONE', ( #50965, #46402, #47760, #18111 ) ) ;
#48146 = CARTESIAN_POINT ( 'NONE',  ( 2.919426793319799707, 1.448220119383965443, 0.4451252810446820196 ) ) ;
#48147 = CARTESIAN_POINT ( 'NONE',  ( 1.214590356376888280, 1.727355838235203667, 1.936932008856820930 ) ) ;
#48148 = EDGE_CURVE ( 'NONE', #26524, #15323, #31375, .T. ) ;
#48149 = DIRECTION ( 'NONE',  ( -0.7071067811865466846, -0.7071067811865483499, 7.903458058585701571E-16 ) ) ;
#48150 = ADVANCED_FACE ( 'NONE', ( #14619 ), #10740, .F. ) ;
#48151 = ORIENTED_EDGE ( 'NONE', *, *, #27689, .T. ) ;
#48152 = LINE ( 'NONE', #12056, #22454 ) ;
#48153 = ORIENTED_EDGE ( 'NONE', *, *, #31083, .T. ) ;
#48154 = FACE_BOUND ( 'NONE', #35191, .T. ) ;
#48155 = CARTESIAN_POINT ( 'NONE',  ( -1.636583440222563635, 3.346456692913386100, 0.6299212598425164567 ) ) ;
#48156 = CARTESIAN_POINT ( 'NONE',  ( -1.325491792074585451, 1.543512378121542961, -2.638988599164751925 ) ) ;
#48157 = LINE ( 'NONE', #32726, #21870 ) ;
#48158 = AXIS2_PLACEMENT_3D ( 'NONE', #9105, #47543, #16865 ) ;
#48159 = ORIENTED_EDGE ( 'NONE', *, *, #38629, .F. ) ;
#48160 = VERTEX_POINT ( 'NONE', #10992 ) ;
#48161 = CARTESIAN_POINT ( 'NONE',  ( -0.2727639067037602172, 3.267716535433071279, 2.047244094488179567 ) ) ;
#48162 = VERTEX_POINT ( 'NONE', #26731 ) ;
#48163 = VECTOR ( 'NONE', #542, 39.37007874015748143 ) ;
#48164 = DIRECTION ( 'NONE',  ( -0.000000000000000000, 1.000000000000000000, -0.000000000000000000 ) ) ;
#48165 = EDGE_LOOP ( 'NONE', ( #12238, #25395, #43030, #6907 ) ) ;
#48166 = VECTOR ( 'NONE', #44112, 39.37007874015748143 ) ;
#48167 = AXIS2_PLACEMENT_3D ( 'NONE', #15163, #11036, #34539 ) ;
#48168 = CARTESIAN_POINT ( 'NONE',  ( 0.000000000000000000, 3.267716535433071279, -0.9448818897637762948 ) ) ;
#48169 = ORIENTED_EDGE ( 'NONE', *, *, #28603, .T. ) ;
#48170 = CARTESIAN_POINT ( 'NONE',  ( 2.252332422952718183, 1.743977176619643910, -0.5645583697864726691 ) ) ;
#48171 = CARTESIAN_POINT ( 'NONE',  ( 1.515849743713622910, 0.000000000000000000, -1.426682437664332559 ) ) ;
#48172 = VECTOR ( 'NONE', #28911, 39.37007874015748143 ) ;
#48173 = ORIENTED_EDGE ( 'NONE', *, *, #5815, .T. ) ;
#48174 = DIRECTION ( 'NONE',  ( -0.9839295885986321100, 0.000000000000000000, 0.1785568947986229116 ) ) ;
#48175 = VERTEX_POINT ( 'NONE', #42477 ) ;
#48176 = DIRECTION ( 'NONE',  ( -0.000000000000000000, 1.000000000000000000, -0.000000000000000000 ) ) ;
#48177 = ADVANCED_FACE ( 'NONE', ( #38617 ), #3243, .T. ) ;
#48178 = ADVANCED_FACE ( 'NONE', ( #26977 ), #42729, .F. ) ;
#48179 = ORIENTED_EDGE ( 'NONE', *, *, #27201, .F. ) ;
#48180 = ORIENTED_EDGE ( 'NONE', *, *, #28828, .T. ) ;
#48181 = CARTESIAN_POINT ( 'NONE',  ( -1.712496953225537633, 3.346456692913386100, -0.9842519685039344823 ) ) ;
#48182 = EDGE_CURVE ( 'NONE', #21434, #34071, #381, .T. ) ;
#48183 = EDGE_LOOP ( 'NONE', ( #25330, #50006, #21659, #12234 ) ) ;
#48184 = LINE ( 'NONE', #28338, #50941 ) ;
#48185 = ORIENTED_EDGE ( 'NONE', *, *, #1303, .F. ) ;
#48186 = CARTESIAN_POINT ( 'NONE',  ( -0.04921259842519707522, 1.574803149606302854, 2.164795024401847456 ) ) ;
#48187 = DIRECTION ( 'NONE',  ( 0.000000000000000000, 1.160734090543304660E-16, -1.000000000000000000 ) ) ;
#48188 = CARTESIAN_POINT ( 'NONE',  ( -0.5455278134075214336, 3.346456692913386100, -1.141732283464563791 ) ) ;
#48189 = ORIENTED_EDGE ( 'NONE', *, *, #14076, .F. ) ;
#48190 = CARTESIAN_POINT ( 'NONE',  ( 0.000000000000000000, 3.267716535433071279, 0.000000000000000000 ) ) ;
#48191 = DIRECTION ( 'NONE',  ( -0.000000000000000000, -1.000000000000000000, -0.000000000000000000 ) ) ;
#48192 = AXIS2_PLACEMENT_3D ( 'NONE', #4927, #36429, #1308 ) ;
#48193 = DIRECTION ( 'NONE',  ( -1.000000000000000000, 0.000000000000000000, 0.000000000000000000 ) ) ;
#48194 = FACE_OUTER_BOUND ( 'NONE', #42601, .T. ) ;
#48195 = CIRCLE ( 'NONE', #31025, 2.244934639244525076 ) ;
#48196 = AXIS2_PLACEMENT_3D ( 'NONE', #13894, #37909, #40754 ) ;
#48197 = EDGE_CURVE ( 'NONE', #14116, #23634, #47853, .T. ) ;
#48198 = DIRECTION ( 'NONE',  ( -0.000000000000000000, 0.000000000000000000, 1.000000000000000000 ) ) ;
#48199 = VECTOR ( 'NONE', #3742, 39.37007874015748143 ) ;
#48200 = CARTESIAN_POINT ( 'NONE',  ( 1.081562861160096700, 0.04524287409729283588, -1.572369041216798768 ) ) ;
#48201 = EDGE_CURVE ( 'NONE', #34165, #50693, #896, .T. ) ;
#48202 = CARTESIAN_POINT ( 'NONE',  ( 0.07982360342473591996, 1.709180471932028711, 0.000000000000000000 ) ) ;
#48203 = ORIENTED_EDGE ( 'NONE', *, *, #40607, .T. ) ;
#48204 = CARTESIAN_POINT ( 'NONE',  ( -0.8949303405208608453, 1.574803149606302854, -1.971765468592543202 ) ) ;
#48205 = CARTESIAN_POINT ( 'NONE',  ( -1.325491792074585451, 1.698604322780517650, -2.638988599164751481 ) ) ;
#48206 = EDGE_CURVE ( 'NONE', #45835, #49700, #44256, .T. ) ;
#48207 = AXIS2_PLACEMENT_3D ( 'NONE', #5592, #48404, #36329 ) ;
#48208 = ORIENTED_EDGE ( 'NONE', *, *, #49708, .F. ) ;
#48209 = DIRECTION ( 'NONE',  ( 1.734723475976806848E-16, -0.000000000000000000, 1.000000000000000000 ) ) ;
#48210 = EDGE_CURVE ( 'NONE', #42475, #28392, #43735, .T. ) ;
#48211 = VERTEX_POINT ( 'NONE', #15865 ) ;
#48212 = FACE_OUTER_BOUND ( 'NONE', #23443, .T. ) ;
#48213 = FACE_OUTER_BOUND ( 'NONE', #47015, .T. ) ;
#48214 = CARTESIAN_POINT ( 'NONE',  ( -1.712496953225537633, 0.000000000000000000, 1.417322834645662333 ) ) ;
#48215 = DIRECTION ( 'NONE',  ( 0.000000000000000000, 1.000000000000000000, 0.000000000000000000 ) ) ;
#48216 = DIRECTION ( 'NONE',  ( 1.734723475976806848E-16, -0.000000000000000000, 1.000000000000000000 ) ) ;
#48217 = VERTEX_POINT ( 'NONE', #24388 ) ;
#48218 = CARTESIAN_POINT ( 'NONE',  ( -1.985260859929297572, 0.000000000000000000, -0.3149606299212589500 ) ) ;
#48219 = DIRECTION ( 'NONE',  ( -3.469446951953613696E-16, 0.000000000000000000, -1.000000000000000000 ) ) ;
#48220 = EDGE_LOOP ( 'NONE', ( #44817, #42155, #23335, #44858 ) ) ;
#48221 = PLANE ( 'NONE',  #27099 ) ;
#48222 = VERTEX_POINT ( 'NONE', #16906 ) ;
#48223 = CARTESIAN_POINT ( 'NONE',  ( -1.472219874544909546, 1.205361022782829114E-17, 2.560030851058948898 ) ) ;
#48224 = DIRECTION ( 'NONE',  ( 1.000000000000000000, 0.000000000000000000, 0.000000000000000000 ) ) ;
#48225 = LINE ( 'NONE', #8515, #36256 ) ;
#48226 = VECTOR ( 'NONE', #15718, 39.37007874015748143 ) ;
#48227 = ORIENTED_EDGE ( 'NONE', *, *, #4538, .F. ) ;
#48228 = ORIENTED_EDGE ( 'NONE', *, *, #9469, .T. ) ;
#48229 = AXIS2_PLACEMENT_3D ( 'NONE', #2023, #11872, #36661 ) ;
#48230 = CARTESIAN_POINT ( 'NONE',  ( 1.229551338984395059, 1.049866565877817237, -1.608606760006217717 ) ) ;
#48231 = CARTESIAN_POINT ( 'NONE',  ( 0.2156685157584258827, 1.205361022782829114E-17, -2.945280361644574185 ) ) ;
#48232 = FACE_BOUND ( 'NONE', #37863, .T. ) ;
#48233 = VECTOR ( 'NONE', #33863, 39.37007874015748143 ) ;
#48234 = CARTESIAN_POINT ( 'NONE',  ( -1.363819533518803029, 0.000000000000000000, -0.03937007874015868020 ) ) ;
#48235 = FACE_OUTER_BOUND ( 'NONE', #38245, .T. ) ;
#48236 = VECTOR ( 'NONE', #11621, 39.37007874015748143 ) ;
#48237 = ORIENTED_EDGE ( 'NONE', *, *, #27350, .F. ) ;
#48238 = DIRECTION ( 'NONE',  ( -0.000000000000000000, 1.000000000000000000, -0.000000000000000000 ) ) ;
#48239 = EDGE_CURVE ( 'NONE', #7511, #48407, #16652, .T. ) ;
#48240 = AXIS2_PLACEMENT_3D ( 'NONE', #45007, #5785, #29536 ) ;
#48241 = EDGE_CURVE ( 'NONE', #9429, #5467, #47839, .T. ) ;
#48242 = ORIENTED_EDGE ( 'NONE', *, *, #26162, .F. ) ;
#48243 = ORIENTED_EDGE ( 'NONE', *, *, #14836, .T. ) ;
#48244 = EDGE_CURVE ( 'NONE', #42191, #38194, #23203, .T. ) ;
#48245 = EDGE_LOOP ( 'NONE', ( #20409, #6791, #19199, #28729 ) ) ;
#48246 = CARTESIAN_POINT ( 'NONE',  ( -2.074656761898998170, 0.000000000000000000, -0.6223516566630912239 ) ) ;
#48247 = CARTESIAN_POINT ( 'NONE',  ( 1.833433833923351575, 3.267716535433071279, -6.361001426714000452E-16 ) ) ;
#48248 = CARTESIAN_POINT ( 'NONE',  ( 0.08139965876239094178, 1.610780518492231694, 0.000000000000000000 ) ) ;
#48249 = PLANE ( 'NONE',  #5747 ) ;
#48250 = ORIENTED_EDGE ( 'NONE', *, *, #33146, .T. ) ;
#48251 = EDGE_LOOP ( 'NONE', ( #9438, #33113, #43333, #42102 ) ) ;
#48252 = FACE_OUTER_BOUND ( 'NONE', #5744, .T. ) ;
#48253 = DIRECTION ( 'NONE',  ( -3.469446951953613696E-16, 0.000000000000000000, -1.000000000000000000 ) ) ;
#48254 = DIRECTION ( 'NONE',  ( 0.000000000000000000, -1.000000000000000000, 0.000000000000000000 ) ) ;
#48255 = FACE_OUTER_BOUND ( 'NONE', #32069, .T. ) ;
#48256 = LINE ( 'NONE', #28671, #5001 ) ;
#48257 = ADVANCED_FACE ( 'NONE', ( #120 ), #16130, .F. ) ;
#48258 = CARTESIAN_POINT ( 'NONE',  ( -1.363819533518803029, 3.346456692913386100, 1.417322834645662777 ) ) ;
#48259 = CARTESIAN_POINT ( 'NONE',  ( -1.636583440222564301, 0.000000000000000000, -1.771653543307080581 ) ) ;
#48260 = CARTESIAN_POINT ( 'NONE',  ( 1.062992125984251413, 0.5905511811023621549, 1.062992125984251413 ) ) ;
#48261 = VERTEX_POINT ( 'NONE', #8130 ) ;
#48262 = VECTOR ( 'NONE', #32838, 39.37007874015748143 ) ;
#48263 = CARTESIAN_POINT ( 'NONE',  ( 1.549117706237081782, 1.699905508662957754, 1.698309735495537431 ) ) ;
#48264 = DIRECTION ( 'NONE',  ( -1.000000000000000000, -0.000000000000000000, -0.000000000000000000 ) ) ;
#48265 = VECTOR ( 'NONE', #34079, 39.37007874015748143 ) ;
#48266 = EDGE_CURVE ( 'NONE', #28712, #19154, #43995, .T. ) ;
#48267 = B_SPLINE_CURVE_WITH_KNOTS ( 'NONE', 3,
 ( #25959, #17707, #14335, #21070 ),
 .UNSPECIFIED., .F., .F.,
 ( 4, 4 ),
 ( 2.174642743374414444E-07, 0.002500329454545664916 ),
 .UNSPECIFIED. ) ;
#48268 = ORIENTED_EDGE ( 'NONE', *, *, #33789, .T. ) ;
#48269 = AXIS2_PLACEMENT_3D ( 'NONE', #22870, #23118, #19237 ) ;
#48270 = EDGE_LOOP ( 'NONE', ( #44197, #14142, #43481, #17861 ) ) ;
#48271 = DIRECTION ( 'NONE',  ( 0.000000000000000000, 0.000000000000000000, -1.000000000000000000 ) ) ;
#48272 = LINE ( 'NONE', #35673, #11336 ) ;
#48273 = PLANE ( 'NONE',  #23884 ) ;
#48274 = ORIENTED_EDGE ( 'NONE', *, *, #28169, .T. ) ;
#48275 = AXIS2_PLACEMENT_3D ( 'NONE', #17476, #21100, #40717 ) ;
#48276 = ORIENTED_EDGE ( 'NONE', *, *, #5442, .F. ) ;
#48277 = CARTESIAN_POINT ( 'NONE',  ( 0.2727639067037610499, 3.346456692913386100, 1.732283464566921172 ) ) ;
#48278 = ORIENTED_EDGE ( 'NONE', *, *, #18286, .T. ) ;
#48279 = VERTEX_POINT ( 'NONE', #39625 ) ;
#48280 = CARTESIAN_POINT ( 'NONE',  ( -0.8942052331142552601, 3.267716535433071279, -0.9448818897637760728 ) ) ;
#48281 = CARTESIAN_POINT ( 'NONE',  ( -1.636583440222564301, 3.346456692913386100, 1.417869535855831753 ) ) ;
#48282 = VERTEX_POINT ( 'NONE', #47327 ) ;
#48283 = ORIENTED_EDGE ( 'NONE', *, *, #15436, .F. ) ;
#48284 = ORIENTED_EDGE ( 'NONE', *, *, #21065, .F. ) ;
#48285 = CARTESIAN_POINT ( 'NONE',  ( -1.905671854841497481, 1.689559879305088996, 2.256015092822653223 ) ) ;
#48286 = VERTEX_POINT ( 'NONE', #31896 ) ;
#48287 = VERTEX_POINT ( 'NONE', #8896 ) ;
#48288 = DIRECTION ( 'NONE',  ( -0.000000000000000000, 1.000000000000000000, -0.000000000000000000 ) ) ;
#48289 = DIRECTION ( 'NONE',  ( -1.000000000000000000, -0.000000000000000000, -0.000000000000000000 ) ) ;
#48290 = DIRECTION ( 'NONE',  ( 0.01601477604151182663, -0.9998717552508123996, 0.000000000000000000 ) ) ;
#48291 = ORIENTED_EDGE ( 'NONE', *, *, #16036, .F. ) ;
#48292 = DIRECTION ( 'NONE',  ( 1.734723475976806848E-16, 0.000000000000000000, 1.000000000000000000 ) ) ;
#48293 = DIRECTION ( 'NONE',  ( -0.000000000000000000, 1.000000000000000000, -0.000000000000000000 ) ) ;
#48294 = DIRECTION ( 'NONE',  ( -1.000000000000000000, 0.000000000000000000, 0.000000000000000000 ) ) ;
#48295 = VECTOR ( 'NONE', #1630, 39.37007874015748143 ) ;
#48296 = EDGE_LOOP ( 'NONE', ( #10958, #28184, #31753, #28435 ) ) ;
#48297 = DIRECTION ( 'NONE',  ( -0.01601477604151182663, 0.9998717552508123996, -0.000000000000000000 ) ) ;
#48298 = CARTESIAN_POINT ( 'NONE',  ( -0.8182917201112819283, 3.267716535433071279, 1.419509857074483292E-16 ) ) ;
#48299 = ADVANCED_FACE ( 'NONE', ( #20518 ), #27484, .F. ) ;
#48300 = VECTOR ( 'NONE', #9232, 39.37007874015748143 ) ;
#48301 = EDGE_CURVE ( 'NONE', #15287, #17089, #134, .T. ) ;
#48302 = VECTOR ( 'NONE', #23140, 39.37007874015748143 ) ;
#48303 = DIRECTION ( 'NONE',  ( -0.000000000000000000, 1.000000000000000000, -0.000000000000000000 ) ) ;
#48304 = ORIENTED_EDGE ( 'NONE', *, *, #23745, .T. ) ;
#48305 = ORIENTED_EDGE ( 'NONE', *, *, #47358, .T. ) ;
#48306 = DIRECTION ( 'NONE',  ( 1.734723475976806848E-16, -0.000000000000000000, 1.000000000000000000 ) ) ;
#48307 = DIRECTION ( 'NONE',  ( -0.9998717552508122886, -0.01601477604151180928, 0.000000000000000000 ) ) ;
#48308 = VECTOR ( 'NONE', #16073, 39.37007874015748143 ) ;
#48309 = EDGE_CURVE ( 'NONE', #10670, #15077, #4770, .T. ) ;
#48310 = DIRECTION ( 'NONE',  ( 1.734723475976806848E-16, 0.000000000000000000, 1.000000000000000000 ) ) ;
#48311 = AXIS2_PLACEMENT_3D ( 'NONE', #29566, #48630, #41195 ) ;
#48312 = DIRECTION ( 'NONE',  ( 0.6427876096865403621, -0.7660444431189770143, 1.858431260983764056E-16 ) ) ;
#48313 = EDGE_CURVE ( 'NONE', #9387, #45742, #47583, .T. ) ;
#48314 = CARTESIAN_POINT ( 'NONE',  ( -0.2834077913992260056, 0.000000000000000000, -0.2440651625074179987 ) ) ;
#48315 = ORIENTED_EDGE ( 'NONE', *, *, #23612, .T. ) ;
#48316 = ORIENTED_EDGE ( 'NONE', *, *, #10813, .T. ) ;
#48317 = VECTOR ( 'NONE', #7065, 39.37007874015748143 ) ;
#48318 = DIRECTION ( 'NONE',  ( -0.000000000000000000, 1.000000000000000000, -0.000000000000000000 ) ) ;
#48319 = ORIENTED_EDGE ( 'NONE', *, *, #43569, .F. ) ;
#48320 = CARTESIAN_POINT ( 'NONE',  ( 2.919426793319799707, 0.000000000000000000, 0.4451252810446820196 ) ) ;
#48321 = CARTESIAN_POINT ( 'NONE',  ( 0.000000000000000000, 3.267716535433071279, -0.9842519685039348154 ) ) ;
#48322 = EDGE_CURVE ( 'NONE', #29978, #2834, #19738, .T. ) ;
#48323 = FACE_OUTER_BOUND ( 'NONE', #21980, .T. ) ;
#48324 = DIRECTION ( 'NONE',  ( 0.000000000000000000, 0.000000000000000000, 1.000000000000000000 ) ) ;
#48325 = PLANE ( 'NONE',  #8070 ) ;
#48326 = ORIENTED_EDGE ( 'NONE', *, *, #34707, .F. ) ;
#48327 = CARTESIAN_POINT ( 'NONE',  ( 0.8227799331039051811, 6.692913385826772199, 2.052232022298800640 ) ) ;
#48328 = EDGE_CURVE ( 'NONE', #12462, #18551, #5024, .T. ) ;
#48329 = DIRECTION ( 'NONE',  ( 0.000000000000000000, 0.000000000000000000, -1.000000000000000000 ) ) ;
#48330 = ORIENTED_EDGE ( 'NONE', *, *, #28181, .T. ) ;
#48331 = CARTESIAN_POINT ( 'NONE',  ( 0.000000000000000000, 3.267716535433071279, 1.377952755905504256 ) ) ;
#48332 = DIRECTION ( 'NONE',  ( -0.000000000000000000, 1.000000000000000000, -0.000000000000000000 ) ) ;
#48333 = CARTESIAN_POINT ( 'NONE',  ( 2.503359584574370800, 1.751360814071121430, 0.3887651481859802360 ) ) ;
#48334 = ORIENTED_EDGE ( 'NONE', *, *, #22658, .F. ) ;
#48335 = VECTOR ( 'NONE', #11290, 39.37007874015748143 ) ;
#48336 = DIRECTION ( 'NONE',  ( -0.000000000000000000, 1.000000000000000000, -0.000000000000000000 ) ) ;
#48337 = CARTESIAN_POINT ( 'NONE',  ( 2.473322567160110452, 1.458187968338687357, -1.612982232707932173 ) ) ;
#48338 = VECTOR ( 'NONE', #25753, 39.37007874015748143 ) ;
#48339 = VERTEX_POINT ( 'NONE', #31627 ) ;
#48340 = DIRECTION ( 'NONE',  ( 1.000000000000000000, 0.000000000000000000, 0.000000000000000000 ) ) ;
#48341 = FACE_OUTER_BOUND ( 'NONE', #4232, .T. ) ;
#48342 = VERTEX_POINT ( 'NONE', #1915 ) ;
#48343 = CARTESIAN_POINT ( 'NONE',  ( 1.833433833923351353, 3.346456692913386100, -0.5118110236220471121 ) ) ;
#48344 = EDGE_CURVE ( 'NONE', #8620, #10759, #13426, .T. ) ;
#48345 = DIRECTION ( 'NONE',  ( 1.734723475976806848E-16, -0.000000000000000000, 1.000000000000000000 ) ) ;
#48346 = LINE ( 'NONE', #44503, #44474 ) ;
#48347 = FACE_OUTER_BOUND ( 'NONE', #19746, .T. ) ;
#48348 = CARTESIAN_POINT ( 'NONE',  ( 0.04921259842519690175, 0.02870789531899127500, 1.849213118431110914 ) ) ;
#48349 = ORIENTED_EDGE ( 'NONE', *, *, #49947, .F. ) ;
#48350 = ORIENTED_EDGE ( 'NONE', *, *, #24971, .T. ) ;
#48351 = LINE ( 'NONE', #45257, #5892 ) ;
#48352 = CARTESIAN_POINT ( 'NONE',  ( -0.07591351300297277671, 0.000000000000000000, 0.7874015748031456541 ) ) ;
#48353 = ORIENTED_EDGE ( 'NONE', *, *, #16958, .F. ) ;
#48354 = DIRECTION ( 'NONE',  ( -1.000000000000000000, 0.000000000000000000, 1.734723475976806848E-16 ) ) ;
#48355 = DIRECTION ( 'NONE',  ( 0.000000000000000000, 0.000000000000000000, -1.000000000000000000 ) ) ;
#48356 = LINE ( 'NONE', #32929, #26936 ) ;
#48357 = DIRECTION ( 'NONE',  ( -0.5773502691896261751, 0.5773502691896261751, 0.5773502691896248429 ) ) ;
#48358 = EDGE_LOOP ( 'NONE', ( #42415, #47860, #2560, #43916 ) ) ;
#48359 = ORIENTED_EDGE ( 'NONE', *, *, #41175, .F. ) ;
#48360 = LINE ( 'NONE', #40158, #38626 ) ;
#48361 = LINE ( 'NONE', #16406, #22512 ) ;
#48362 = CARTESIAN_POINT ( 'NONE',  ( -1.363819533518803029, 3.267716535433071279, 1.417322834645662777 ) ) ;
#48363 = ORIENTED_EDGE ( 'NONE', *, *, #17282, .T. ) ;
#48364 = FACE_OUTER_BOUND ( 'NONE', #8807, .T. ) ;
#48365 = FACE_BOUND ( 'NONE', #40844, .T. ) ;
#48366 = VERTEX_POINT ( 'NONE', #45012 ) ;
#48367 = LINE ( 'NONE', #40165, #8441 ) ;
#48368 = ORIENTED_EDGE ( 'NONE', *, *, #35057, .T. ) ;
#48369 = VERTEX_POINT ( 'NONE', #17409 ) ;
#48370 = CARTESIAN_POINT ( 'NONE',  ( 1.363819533518803029, 3.346456692913386100, -1.605145679676863724 ) ) ;
#48371 = B_SPLINE_CURVE_WITH_KNOTS ( 'NONE', 3,
 ( #44594, #40494, #12876, #39269 ),
 .UNSPECIFIED., .F., .F.,
 ( 4, 4 ),
 ( 0.01480784793388801278, 0.03075119829274991501 ),
 .UNSPECIFIED. ) ;
#48372 = EDGE_CURVE ( 'NONE', #39490, #180, #6038, .T. ) ;
#48373 = ADVANCED_FACE ( 'NONE', ( #14044 ), #11666, .T. ) ;
#48374 = VECTOR ( 'NONE', #15318, 39.37007874015748143 ) ;
#48375 = VERTEX_POINT ( 'NONE', #5790 ) ;
#48376 = CARTESIAN_POINT ( 'NONE',  ( 0.2627480064045706332, 0.000000000000000000, 1.723473835155035605 ) ) ;
#48377 = ADVANCED_FACE ( 'NONE', ( #5276 ), #33430, .F. ) ;
#48378 = ORIENTED_EDGE ( 'NONE', *, *, #28042, .F. ) ;
#48379 = VECTOR ( 'NONE', #7098, 39.37007874015748143 ) ;
#48380 = CARTESIAN_POINT ( 'NONE',  ( -0.5455278134075214336, 0.000000000000000000, -1.574803149606293529 ) ) ;
#48381 = CARTESIAN_POINT ( 'NONE',  ( 0.000000000000000000, 0.07874015748031502893, 0.000000000000000000 ) ) ;
#48382 = CARTESIAN_POINT ( 'NONE',  ( 1.472219874544873131, 0.000000000000000000, 2.560030851058970214 ) ) ;
#48383 = DIRECTION ( 'NONE',  ( -0.9362348706397368714, 0.000000000000000000, -0.3513748240813434620 ) ) ;
#48384 = CARTESIAN_POINT ( 'NONE',  ( 0.7423782071083082634, 3.346456692913386100, -1.771653543307081025 ) ) ;
#48385 = LINE ( 'NONE', #40689, #42673 ) ;
#48386 = ORIENTED_EDGE ( 'NONE', *, *, #32502, .F. ) ;
#48387 = CARTESIAN_POINT ( 'NONE',  ( 0.07982360342473591996, 1.709180471932028711, 0.000000000000000000 ) ) ;
#48388 = FACE_OUTER_BOUND ( 'NONE', #32250, .T. ) ;
#48389 = ORIENTED_EDGE ( 'NONE', *, *, #28557, .T. ) ;
#48390 = DIRECTION ( 'NONE',  ( 0.000000000000000000, 0.000000000000000000, -1.000000000000000000 ) ) ;
#48391 = CARTESIAN_POINT ( 'NONE',  ( 0.000000000000000000, 6.692913385826772199, 0.000000000000000000 ) ) ;
#48392 = EDGE_LOOP ( 'NONE', ( #24097, #45575, #45471, #2514 ) ) ;
#48393 = PLANE ( 'NONE',  #39471 ) ;
#48394 = EDGE_CURVE ( 'NONE', #13777, #4133, #9922, .T. ) ;
#48395 = PLANE ( 'NONE',  #13575 ) ;
#48396 = CARTESIAN_POINT ( 'NONE',  ( 1.014069264286642014, 0.5905511811023621549, 1.062992125984251635 ) ) ;
#48397 = ORIENTED_EDGE ( 'NONE', *, *, #1822, .F. ) ;
#48398 = DIRECTION ( 'NONE',  ( -0.01601477604151182663, 0.9998717552508123996, -0.000000000000000000 ) ) ;
#48399 = ORIENTED_EDGE ( 'NONE', *, *, #36420, .T. ) ;
#48400 = FACE_BOUND ( 'NONE', #39970, .T. ) ;
#48401 = EDGE_CURVE ( 'NONE', #18633, #46194, #29018, .T. ) ;
#48402 = FACE_OUTER_BOUND ( 'NONE', #32926, .T. ) ;
#48403 = CARTESIAN_POINT ( 'NONE',  ( -1.158605206299305079, 1.033703605627220856, -2.292445033001472510 ) ) ;
#48404 = DIRECTION ( 'NONE',  ( 0.5624310017906212211, 0.000000000000000000, -0.8268442224656336048 ) ) ;
#48405 = AXIS2_PLACEMENT_3D ( 'NONE', #25149, #36518, #9657 ) ;
#48406 = VECTOR ( 'NONE', #11418, 39.37007874015748143 ) ;
#48407 = VERTEX_POINT ( 'NONE', #5535 ) ;
#48408 = ORIENTED_EDGE ( 'NONE', *, *, #26709, .T. ) ;
#48409 = DIRECTION ( 'NONE',  ( 1.734723475976806848E-16, 0.000000000000000000, 1.000000000000000000 ) ) ;
#48410 = ORIENTED_EDGE ( 'NONE', *, *, #27177, .T. ) ;
#48411 = B_SPLINE_CURVE_WITH_KNOTS ( 'NONE', 3,
 ( #7158, #38396, #34272, #26507 ),
 .UNSPECIFIED., .F., .F.,
 ( 4, 4 ),
 ( 0.001167289351993227057, 0.003667579486304786175 ),
 .UNSPECIFIED. ) ;
#48412 = EDGE_CURVE ( 'NONE', #50925, #24535, #21568, .T. ) ;
#48413 = CARTESIAN_POINT ( 'NONE',  ( 1.363819533518803251, 3.346456692913386100, 0.4724409448818871482 ) ) ;
#48414 = ORIENTED_EDGE ( 'NONE', *, *, #38133, .T. ) ;
#48415 = EDGE_CURVE ( 'NONE', #30087, #6948, #9411, .T. ) ;
#48416 = DIRECTION ( 'NONE',  ( -1.000000000000000000, 0.000000000000000000, 0.000000000000000000 ) ) ;
#48417 = ORIENTED_EDGE ( 'NONE', *, *, #38582, .T. ) ;
#48418 = CARTESIAN_POINT ( 'NONE',  ( 0.8182917201112819283, 3.346456692913386100, 0.7874015748031454320 ) ) ;
#48419 = AXIS2_PLACEMENT_3D ( 'NONE', #46906, #27311, #14446 ) ;
#48420 = CARTESIAN_POINT ( 'NONE',  ( -4.268512490100411402E-16, 0.000000000000000000, -2.086614173228339641 ) ) ;
#48421 = EDGE_LOOP ( 'NONE', ( #39430, #13120, #37550, #5542 ) ) ;
#48422 = DIRECTION ( 'NONE',  ( 0.000000000000000000, -1.000000000000000000, 0.000000000000000000 ) ) ;
#48423 = VERTEX_POINT ( 'NONE', #37552 ) ;
#48424 = ORIENTED_EDGE ( 'NONE', *, *, #1303, .T. ) ;
#48425 = VECTOR ( 'NONE', #40181, 39.37007874015748143 ) ;
#48426 = EDGE_CURVE ( 'NONE', #528, #20175, #2170, .T. ) ;
#48427 = ORIENTED_EDGE ( 'NONE', *, *, #10486, .T. ) ;
#48428 = ORIENTED_EDGE ( 'NONE', *, *, #24436, .F. ) ;
#48429 = ADVANCED_FACE ( 'NONE', ( #21535 ), #2430, .F. ) ;
#48430 = EDGE_CURVE ( 'NONE', #34518, #5087, #1406, .T. ) ;
#48431 = LINE ( 'NONE', #44585, #21451 ) ;
#48432 = EDGE_CURVE ( 'NONE', #2087, #28641, #25918, .T. ) ;
#48433 = VERTEX_POINT ( 'NONE', #32664 ) ;
#48434 = DIRECTION ( 'NONE',  ( -0.000000000000000000, 1.000000000000000000, -0.000000000000000000 ) ) ;
#48435 = VERTEX_POINT ( 'NONE', #13796 ) ;
#48436 = DIRECTION ( 'NONE',  ( 0.000000000000000000, 0.000000000000000000, -1.000000000000000000 ) ) ;
#48437 = VECTOR ( 'NONE', #7681, 39.37007874015748143 ) ;
#48438 = VECTOR ( 'NONE', #1522, 39.37007874015748143 ) ;
#48439 = CARTESIAN_POINT ( 'NONE',  ( -0.07591351300297333182, 0.000000000000000000, -0.4724409448818883694 ) ) ;
#48440 = ORIENTED_EDGE ( 'NONE', *, *, #6771, .T. ) ;
#48441 = CARTESIAN_POINT ( 'NONE',  ( -1.891439052599157122, 1.677607092856729709, 1.073712343777111222 ) ) ;
#48442 = CARTESIAN_POINT ( 'NONE',  ( 2.932638728931774352, 1.764957438482779528, 0.3475908556738225297 ) ) ;
#48443 = PLANE ( 'NONE',  #14223 ) ;
#48444 = DIRECTION ( 'NONE',  ( 1.734723475976806848E-16, 0.000000000000000000, 1.000000000000000000 ) ) ;
#48445 = AXIS2_PLACEMENT_3D ( 'NONE', #21558, #46040, #1938 ) ;
#48446 = DIRECTION ( 'NONE',  ( -0.000000000000000000, -1.000000000000000000, -0.000000000000000000 ) ) ;
#48447 = PLANE ( 'NONE',  #22369 ) ;
#48448 = VECTOR ( 'NONE', #6483, 39.37007874015748143 ) ;
#48449 = DIRECTION ( 'NONE',  ( -1.000000000000000000, 0.000000000000000000, -0.000000000000000000 ) ) ;
#48450 = ORIENTED_EDGE ( 'NONE', *, *, #22247, .T. ) ;
#48451 = CARTESIAN_POINT ( 'NONE',  ( 0.4696143004045478797, 3.346456692913386100, -0.9842519685039348154 ) ) ;
#48452 = EDGE_CURVE ( 'NONE', #1599, #1205, #13541, .T. ) ;
#48453 = LINE ( 'NONE', #48708, #5309 ) ;
#48454 = AXIS2_PLACEMENT_3D ( 'NONE', #16424, #9183, #19766 ) ;
#48455 = ORIENTED_EDGE ( 'NONE', *, *, #4287, .F. ) ;
#48456 = CARTESIAN_POINT ( 'NONE',  ( 1.500371432800224003, 1.481001073728986484, 2.543211078004788295 ) ) ;
#48457 = AXIS2_PLACEMENT_3D ( 'NONE', #16367, #28479, #31864 ) ;
#48458 = VERTEX_POINT ( 'NONE', #36779 ) ;
#48459 = CARTESIAN_POINT ( 'NONE',  ( -2.339241080213612101, 1.584370211609867685, 1.802537235681884065 ) ) ;
#48460 = EDGE_CURVE ( 'NONE', #43653, #46669, #17159, .T. ) ;
#48461 = LINE ( 'NONE', #44370, #19256 ) ;
#48462 = DIRECTION ( 'NONE',  ( 0.000000000000000000, -1.000000000000000000, 0.000000000000000000 ) ) ;
#48463 = EDGE_CURVE ( 'NONE', #2530, #1296, #48351, .T. ) ;
#48464 = DIRECTION ( 'NONE',  ( -3.469446951953613696E-16, 0.000000000000000000, -1.000000000000000000 ) ) ;
#48465 = CARTESIAN_POINT ( 'NONE',  ( 3.937007874015748143, 4.960629921259846142, 1.023622047244094446 ) ) ;
#48466 = VERTEX_POINT ( 'NONE', #28766 ) ;
#48467 = EDGE_CURVE ( 'NONE', #45283, #14052, #44508, .T. ) ;
#48468 = DIRECTION ( 'NONE',  ( 0.7530714660036099684, 1.288287287306305530E-16, 0.6579387259397138088 ) ) ;
#48469 = FACE_BOUND ( 'NONE', #17108, .T. ) ;
#48470 = EDGE_LOOP ( 'NONE', ( #34680, #47590, #32194, #42927 ) ) ;
#48471 = CARTESIAN_POINT ( 'NONE',  ( 2.378961647330872342, 3.230577599468342775, 0.6299212598425161236 ) ) ;
#48472 = ORIENTED_EDGE ( 'NONE', *, *, #7617, .F. ) ;
#48473 = PLANE ( 'NONE',  #37607 ) ;
#48474 = CARTESIAN_POINT ( 'NONE',  ( 2.491402175429654253, 1.659612532563349285, -1.585592796919505831 ) ) ;
#48475 = VECTOR ( 'NONE', #8452, 39.37007874015748143 ) ;
#48476 = LINE ( 'NONE', #8063, #1837 ) ;
#48477 = EDGE_CURVE ( 'NONE', #33855, #28296, #34930, .T. ) ;
#48478 = DIRECTION ( 'NONE',  ( -0.000000000000000000, 1.000000000000000000, -0.000000000000000000 ) ) ;
#48479 = ORIENTED_EDGE ( 'NONE', *, *, #36215, .T. ) ;
#48480 = VERTEX_POINT ( 'NONE', #46518 ) ;
#48481 = CARTESIAN_POINT ( 'NONE',  ( -0.6214413264104939882, 0.000000000000000000, 0.2755905511810998187 ) ) ;
#48482 = DIRECTION ( 'NONE',  ( 1.734723475976806848E-16, 0.000000000000000000, 1.000000000000000000 ) ) ;
#48483 = FACE_BOUND ( 'NONE', #12690, .T. ) ;
#48484 = EDGE_CURVE ( 'NONE', #31704, #21978, #25690, .T. ) ;
#48485 = ORIENTED_EDGE ( 'NONE', *, *, #7026, .F. ) ;
#48486 = EDGE_CURVE ( 'NONE', #14018, #13884, #14808, .T. ) ;
#48487 = AXIS2_PLACEMENT_3D ( 'NONE', #41037, #9275, #25530 ) ;
#48488 = CARTESIAN_POINT ( 'NONE',  ( 0.4696143004045479352, 0.000000000000000000, -0.7874015748031473194 ) ) ;
#48489 = CARTESIAN_POINT ( 'NONE',  ( -0.6233543567505159810, 5.905511811023623991, -2.073689640095379705 ) ) ;
#48490 = ORIENTED_EDGE ( 'NONE', *, *, #16557, .F. ) ;
#48491 = EDGE_CURVE ( 'NONE', #4498, #42300, #24095, .T. ) ;
#48492 = ADVANCED_FACE ( 'NONE', ( #26917 ), #27168, .T. ) ;
#48493 =( GEOMETRIC_REPRESENTATION_CONTEXT ( 3 ) GLOBAL_UNCERTAINTY_ASSIGNED_CONTEXT ( ( #8669 ) ) GLOBAL_UNIT_ASSIGNED_CONTEXT ( ( #21318, #34398, #7018 ) ) REPRESENTATION_CONTEXT ( 'NONE', 'WORKASPACE' ) );
#48494 = CARTESIAN_POINT ( 'NONE',  ( 0.000000000000000000, 3.267716535433071279, 1.220472440944875059 ) ) ;
#48495 = EDGE_CURVE ( 'NONE', #2174, #21262, #10928, .T. ) ;
#48496 = DIRECTION ( 'NONE',  ( 0.2225209339563184452, -1.160734090543304660E-16, -0.9749279121818227312 ) ) ;
#48497 = ORIENTED_EDGE ( 'NONE', *, *, #29240, .T. ) ;
#48498 = ORIENTED_EDGE ( 'NONE', *, *, #18494, .F. ) ;
#48499 = VECTOR ( 'NONE', #5324, 39.37007874015748143 ) ;
#48500 = ORIENTED_EDGE ( 'NONE', *, *, #28410, .T. ) ;
#48501 = LINE ( 'NONE', #13183, #19336 ) ;
#48502 = DIRECTION ( 'NONE',  ( -1.000000000000000000, 0.000000000000000000, 1.734723475976806848E-16 ) ) ;
#48503 = DIRECTION ( 'NONE',  ( 1.734723475976806848E-16, -0.000000000000000000, 1.000000000000000000 ) ) ;
#48504 = DIRECTION ( 'NONE',  ( 0.000000000000000000, 0.000000000000000000, -1.000000000000000000 ) ) ;
#48505 = ORIENTED_EDGE ( 'NONE', *, *, #50686, .T. ) ;
#48506 = VERTEX_POINT ( 'NONE', #10424 ) ;
#48507 = CARTESIAN_POINT ( 'NONE',  ( -1.105178190331685961, 1.205361022782829114E-17, -1.437421806808603542 ) ) ;
#48508 =( LENGTH_UNIT ( ) NAMED_UNIT ( * ) SI_UNIT ( $, .METRE. ) );
#48509 = DIRECTION ( 'NONE',  ( 0.000000000000000000, 0.6427876096865404731, 0.7660444431189771253 ) ) ;
#48510 = CARTESIAN_POINT ( 'NONE',  ( 0.3136974817028392315, 0.000000000000000000, -2.936457595020219635 ) ) ;
#48511 = CARTESIAN_POINT ( 'NONE',  ( -0.8942052331142547050, 3.346456692913386100, 1.062992125984246083 ) ) ;
#48512 = LINE ( 'NONE', #12943, #39132 ) ;
#48513 = VECTOR ( 'NONE', #29345, 39.37007874015748143 ) ;
#48514 = CARTESIAN_POINT ( 'NONE',  ( 2.623503965249849301, 1.205361022782829114E-17, 1.355882097269873965 ) ) ;
#48515 = ORIENTED_EDGE ( 'NONE', *, *, #32804, .T. ) ;
#48516 = DIRECTION ( 'NONE',  ( 0.01601477604151182663, -0.9998717552508123996, 0.000000000000000000 ) ) ;
#48517 = LINE ( 'NONE', #5954, #13710 ) ;
#48518 = ORIENTED_EDGE ( 'NONE', *, *, #43668, .T. ) ;
#48519 = VERTEX_POINT ( 'NONE', #39049 ) ;
#48520 = AXIS2_PLACEMENT_3D ( 'NONE', #36216, #24077, #12205 ) ;
#48522 = LINE ( 'NONE', #40824, #45489 ) ;
#48521 = CONICAL_SURFACE ( 'NONE', #18095, 2.165354330708661568, 0.2617993877991570129 ) ;
#48523 = CARTESIAN_POINT ( 'NONE',  ( -1.363819533518803473, 3.256074231195845936, 2.034181048058245178 ) ) ;
#48524 = EDGE_CURVE ( 'NONE', #50172, #28376, #30553, .T. ) ;
#48525 = ORIENTED_EDGE ( 'NONE', *, *, #30409, .F. ) ;
#48526 = AXIS2_PLACEMENT_3D ( 'NONE', #23043, #18160, #37793 ) ;
#48527 = ADVANCED_FACE ( 'NONE', ( #15307 ), #46020, .T. ) ;
#48528 = ORIENTED_EDGE ( 'NONE', *, *, #26974, .F. ) ;
#48529 = DIRECTION ( 'NONE',  ( -3.469446951953613696E-16, 0.000000000000000000, -1.000000000000000000 ) ) ;
#48530 = ORIENTED_EDGE ( 'NONE', *, *, #13039, .F. ) ;
#48531 = VECTOR ( 'NONE', #44994, 39.37007874015748143 ) ;
#48532 = ORIENTED_EDGE ( 'NONE', *, *, #36179, .F. ) ;
#48533 = CARTESIAN_POINT ( 'NONE',  ( -1.091055626815042645, 3.346456692913386100, -0.9448818897637760728 ) ) ;
#48534 = B_SPLINE_CURVE_WITH_KNOTS ( 'NONE', 3,
 ( #11256, #42982, #30880, #50434 ),
 .UNSPECIFIED., .F., .F.,
 ( 4, 4 ),
 ( 2.001965537720647568E-07, 0.002500201682199559936 ),
 .UNSPECIFIED. ) ;
#48535 = CARTESIAN_POINT ( 'NONE',  ( 0.1198125009631641619, 0.5249316475426862860, -1.880232807967558761 ) ) ;
#48536 = ORIENTED_EDGE ( 'NONE', *, *, #23875, .T. ) ;
#48537 = DIMENSIONAL_EXPONENTS ( 1.000000000000000000, 0.000000000000000000, 0.000000000000000000, 0.000000000000000000, 0.000000000000000000, 0.000000000000000000, 0.000000000000000000 ) ;
#48538 = ORIENTED_EDGE ( 'NONE', *, *, #44766, .F. ) ;
#48539 = ORIENTED_EDGE ( 'NONE', *, *, #21799, .T. ) ;
#48540 = DIRECTION ( 'NONE',  ( -0.000000000000000000, 1.000000000000000000, -0.000000000000000000 ) ) ;
#48541 = ORIENTED_EDGE ( 'NONE', *, *, #1367, .T. ) ;
#48542 = ORIENTED_EDGE ( 'NONE', *, *, #19113, .T. ) ;
#48543 = FACE_OUTER_BOUND ( 'NONE', #13354, .T. ) ;
#48544 = CARTESIAN_POINT ( 'NONE',  ( -2.076656781855024114, 1.674640491952791077, 0.6230015025396302697 ) ) ;
#48545 = CARTESIAN_POINT ( 'NONE',  ( 0.2727639067037602172, 3.346456692913386100, -1.732283464566922726 ) ) ;
#48546 = EDGE_CURVE ( 'NONE', #5661, #1626, #46270, .T. ) ;
#48547 = ORIENTED_EDGE ( 'NONE', *, *, #47881, .F. ) ;
#48548 = EDGE_CURVE ( 'NONE', #7183, #536, #30044, .T. ) ;
#48549 = LINE ( 'NONE', #44198, #8174 ) ;
#48550 = CARTESIAN_POINT ( 'NONE',  ( -0.2727639067037607723, 0.000000000000000000, -0.1574803149606301411 ) ) ;
#48551 = VECTOR ( 'NONE', #37741, 39.37007874015748854 ) ;
#48552 = LINE ( 'NONE', #24595, #31950 ) ;
#48553 = ORIENTED_EDGE ( 'NONE', *, *, #42057, .F. ) ;
#48554 = EDGE_CURVE ( 'NONE', #3036, #36908, #50122, .T. ) ;
#48555 = LINE ( 'NONE', #13238, #15827 ) ;
#48556 = CARTESIAN_POINT ( 'NONE',  ( -0.9302092402134559679, 3.346456692913386100, 1.889763779527550147 ) ) ;
#48557 = ADVANCED_FACE ( 'NONE', ( #2931 ), #34433, .F. ) ;
#48558 = DIRECTION ( 'NONE',  ( 0.000000000000000000, 0.000000000000000000, -1.000000000000000000 ) ) ;
#48559 = ORIENTED_EDGE ( 'NONE', *, *, #16470, .F. ) ;
#48560 = ORIENTED_EDGE ( 'NONE', *, *, #10519, .T. ) ;
#48561 = B_SPLINE_CURVE_WITH_KNOTS ( 'NONE', 3,
 ( #9165, #41181, #21043, #24914 ),
 .UNSPECIFIED., .F., .F.,
 ( 4, 4 ),
 ( 0.05135061866764987354, 0.05233018460755119172 ),
 .UNSPECIFIED. ) ;
#48562 = CARTESIAN_POINT ( 'NONE',  ( -2.182111253630085290, 3.346456692913386100, 0.9448818897637749625 ) ) ;
#48563 =( NAMED_UNIT ( * ) PLANE_ANGLE_UNIT ( ) SI_UNIT ( $, .RADIAN. ) );
#48564 = EDGE_CURVE ( 'NONE', #4986, #44778, #41385, .T. ) ;
#48565 = VECTOR ( 'NONE', #7275, 39.37007874015748143 ) ;
#48566 = CARTESIAN_POINT ( 'NONE',  ( -1.985260859929297794, 3.346456692913386100, -0.5118110236220464460 ) ) ;
#48567 = FACE_OUTER_BOUND ( 'NONE', #34180, .T. ) ;
#48568 = DIRECTION ( 'NONE',  ( 0.9989930665413151445, 0.000000000000000000, -0.04486483035050446017 ) ) ;
#48569 = ORIENTED_EDGE ( 'NONE', *, *, #4108, .T. ) ;
#48570 = ORIENTED_EDGE ( 'NONE', *, *, #11859, .F. ) ;
#48571 = DIRECTION ( 'NONE',  ( -0.9998717552508122886, -0.01601477604151185785, 0.000000000000000000 ) ) ;
#48572 = VECTOR ( 'NONE', #24645, 39.37007874015748143 ) ;
#48573 = VERTEX_POINT ( 'NONE', #26172 ) ;
#48574 = LINE ( 'NONE', #48320, #211 ) ;
#48575 = LINE ( 'NONE', #33645, #25948 ) ;
#48576 = CARTESIAN_POINT ( 'NONE',  ( 0.1968503937007869686, 0.000000000000000000, -2.086614173228339641 ) ) ;
#48577 = CARTESIAN_POINT ( 'NONE',  ( -0.5662636741187642153, 0.000000000000000000, 1.648861433446455971 ) ) ;
#48578 = DIRECTION ( 'NONE',  ( 3.586865599282426309E-17, -1.000000000000000000, -1.103923720497134591E-16 ) ) ;
#48579 = EDGE_LOOP ( 'NONE', ( #17213, #16870, #31448, #31279 ) ) ;
#48580 = CARTESIAN_POINT ( 'NONE',  ( -0.8182917201112817063, 3.267716535433071279, 1.419509857074483046E-16 ) ) ;
#48581 = LINE ( 'NONE', #44988, #23230 ) ;
#48582 = VERTEX_POINT ( 'NONE', #41917 ) ;
#48583 = LINE ( 'NONE', #13267, #37275 ) ;
#48584 = DIRECTION ( 'NONE',  ( 0.000000000000000000, 0.000000000000000000, -1.000000000000000000 ) ) ;
#48585 = VECTOR ( 'NONE', #9799, 39.37007874015748143 ) ;
#48586 = EDGE_LOOP ( 'NONE', ( #405, #35901, #6527, #47458, #37199 ) ) ;
#48587 = PLANE ( 'NONE',  #9360 ) ;
#48588 = DIRECTION ( 'NONE',  ( -1.000000000000000000, 0.000000000000000000, 0.000000000000000000 ) ) ;
#48589 = EDGE_CURVE ( 'NONE', #45311, #10447, #42416, .T. ) ;
#48590 = ADVANCED_FACE ( 'NONE', ( #26419 ), #19168, .F. ) ;
#48591 = ORIENTED_EDGE ( 'NONE', *, *, #46291, .T. ) ;
#48592 = DIRECTION ( 'NONE',  ( 0.9959742939952397345, 1.036504026185339538E-17, -0.08963930890342654279 ) ) ;
#48593 = CARTESIAN_POINT ( 'NONE',  ( -1.635196357419856472, 0.5249316475426862860, 0.9358222695712326011 ) ) ;
#48594 = VERTEX_POINT ( 'NONE', #18425 ) ;
#48595 = CARTESIAN_POINT ( 'NONE',  ( 1.287906020515830585, 3.346456692913386100, 1.889763779527550369 ) ) ;
#48596 = EDGE_CURVE ( 'NONE', #12397, #50364, #5369, .T. ) ;
#48597 = AXIS2_PLACEMENT_3D ( 'NONE', #42818, #14960, #7460 ) ;
#48598 = CARTESIAN_POINT ( 'NONE',  ( -2.277873973731453283, 1.205361022782829114E-17, 1.879489153247635214 ) ) ;
#48599 = CARTESIAN_POINT ( 'NONE',  ( 2.437180031585944207, 1.658768335924418080, -1.667735833703099191 ) ) ;
#48600 = LINE ( 'NONE', #38054, #30962 ) ;
#48601 = EDGE_CURVE ( 'NONE', #41415, #40985, #30804, .T. ) ;
#48602 = LINE ( 'NONE', #13284, #43577 ) ;
#48603 = ORIENTED_EDGE ( 'NONE', *, *, #48615, .T. ) ;
#48604 = ORIENTED_EDGE ( 'NONE', *, *, #40903, .F. ) ;
#48605 = CARTESIAN_POINT ( 'NONE',  ( -0.2727639067037608278, 0.000000000000000000, -1.929133858267710000 ) ) ;
#48606 = CARTESIAN_POINT ( 'NONE',  ( -2.182111253630085734, 0.000000000000000000, -1.141732283464563791 ) ) ;
#48607 = ORIENTED_EDGE ( 'NONE', *, *, #47807, .T. ) ;
#48608 = DIRECTION ( 'NONE',  ( -5.207613805427244364E-18, -1.000000000000000000, -1.159565308550900415E-16 ) ) ;
#48609 = DIRECTION ( 'NONE',  ( -0.000000000000000000, 1.000000000000000000, -0.000000000000000000 ) ) ;
#48610 = VECTOR ( 'NONE', #35682, 39.37007874015748854 ) ;
#48611 = LINE ( 'NONE', #16911, #26097 ) ;
#48612 = DIRECTION ( 'NONE',  ( -1.000000000000000000, 0.000000000000000000, 1.734723475976806848E-16 ) ) ;
#48613 = ORIENTED_EDGE ( 'NONE', *, *, #13986, .F. ) ;
#48614 = EDGE_LOOP ( 'NONE', ( #29543, #41111, #27339, #12112 ) ) ;
#48615 = EDGE_CURVE ( 'NONE', #32836, #36716, #35438, .T. ) ;
#48616 = CARTESIAN_POINT ( 'NONE',  ( 0.000000000000000000, 3.267716535433071279, 0.9055118110236164419 ) ) ;
#48617 = DIRECTION ( 'NONE',  ( -1.000000000000000000, 0.000000000000000000, -0.000000000000000000 ) ) ;
#48618 = CYLINDRICAL_SURFACE ( 'NONE', #47769, 2.165354330708661568 ) ;
#48619 = ORIENTED_EDGE ( 'NONE', *, *, #48016, .F. ) ;
#48620 = CARTESIAN_POINT ( 'NONE',  ( 0.000000000000000000, 3.267716535433071279, -0.9842519685039344823 ) ) ;
#48621 = FACE_BOUND ( 'NONE', #42110, .T. ) ;
#48622 = B_SPLINE_CURVE_WITH_KNOTS ( 'NONE', 3,
 ( #16666, #8652, #3064, #8401 ),
 .UNSPECIFIED., .F., .F.,
 ( 4, 4 ),
 ( 2.074994414937302994E-07, 0.002500489374955372577 ),
 .UNSPECIFIED. ) ;
#48623 = ORIENTED_EDGE ( 'NONE', *, *, #16884, .T. ) ;
#48624 = EDGE_CURVE ( 'NONE', #35542, #29386, #13163, .T. ) ;
#48625 = DIRECTION ( 'NONE',  ( -0.000000000000000000, 1.000000000000000000, -0.000000000000000000 ) ) ;
#48626 = VERTEX_POINT ( 'NONE', #312 ) ;
#48627 = ORIENTED_EDGE ( 'NONE', *, *, #18548, .F. ) ;
#48628 = DIRECTION ( 'NONE',  ( 0.3930250316539147803, -1.160734090543304660E-16, 0.9195277725514544587 ) ) ;
#48629 = ORIENTED_EDGE ( 'NONE', *, *, #16932, .F. ) ;
#48630 = DIRECTION ( 'NONE',  ( -1.000000000000000000, 0.000000000000000000, 1.734723475976806848E-16 ) ) ;
#48631 = VERTEX_POINT ( 'NONE', #20182 ) ;
#48632 = ADVANCED_FACE ( 'NONE', ( #4444 ), #30699, .T. ) ;
#48633 = CARTESIAN_POINT ( 'NONE',  ( 0.8454231601665999074, 1.623017753118757067, 2.112564685048140323 ) ) ;
#48634 = CARTESIAN_POINT ( 'NONE',  ( -1.621795816027382875, 0.000000000000000000, -0.6396693727619442438 ) ) ;
#48635 = AXIS2_PLACEMENT_3D ( 'NONE', #39403, #28285, #37331 ) ;
#48636 = DIRECTION ( 'NONE',  ( -1.000000000000000000, 0.000000000000000000, 0.000000000000000000 ) ) ;
#48637 = LINE ( 'NONE', #44792, #41021 ) ;
#48638 = CARTESIAN_POINT ( 'NONE',  ( -1.091055626815042645, 3.346456692913386100, -1.141732283464563569 ) ) ;
#48639 = ORIENTED_EDGE ( 'NONE', *, *, #2206, .T. ) ;
#48640 = DIRECTION ( 'NONE',  ( 1.734723475976806848E-16, 0.000000000000000000, 1.000000000000000000 ) ) ;
#48641 = VECTOR ( 'NONE', #34313, 39.37007874015748143 ) ;
#48642 = DIRECTION ( 'NONE',  ( -3.469446951953613696E-16, 0.000000000000000000, -1.000000000000000000 ) ) ;
#48643 = ORIENTED_EDGE ( 'NONE', *, *, #28864, .T. ) ;
#48644 = CARTESIAN_POINT ( 'NONE',  ( 0.8454231601665999074, 1.623017753118757067, 2.112564685048140323 ) ) ;
#48645 = CARTESIAN_POINT ( 'NONE',  ( -1.363819533518803473, 3.267716535433071279, 2.027638360164056852 ) ) ;
#48646 = ORIENTED_EDGE ( 'NONE', *, *, #4703, .T. ) ;
#48647 = DIRECTION ( 'NONE',  ( 0.000000000000000000, 1.000000000000000000, 0.000000000000000000 ) ) ;
#48648 = CARTESIAN_POINT ( 'NONE',  ( -0.2727639067037602727, 0.000000000000000000, 1.850393700787392293 ) ) ;
#48649 = CARTESIAN_POINT ( 'NONE',  ( 2.111804831410495353, 1.708917971481227260, -0.9561481288353351760 ) ) ;
#48650 = EDGE_CURVE ( 'NONE', #6833, #30930, #48476, .T. ) ;
#48651 = ORIENTED_EDGE ( 'NONE', *, *, #10915, .F. ) ;
#48652 = DIRECTION ( 'NONE',  ( -0.000000000000000000, 1.000000000000000000, -0.000000000000000000 ) ) ;
#48653 = ORIENTED_EDGE ( 'NONE', *, *, #12507, .T. ) ;
#48654 = FACE_BOUND ( 'NONE', #20179, .T. ) ;
#48655 = ADVANCED_FACE ( 'NONE', ( #50861 ), #39812, .T. ) ;
#48656 = LINE ( 'NONE', #697, #2027 ) ;
#48657 = DIRECTION ( 'NONE',  ( 0.000000000000000000, -1.000000000000000000, 0.000000000000000000 ) ) ;
#48659 = EDGE_CURVE ( 'NONE', #26933, #49804, #31563, .T. ) ;
#48658 = DIRECTION ( 'NONE',  ( -0.000000000000000000, 1.000000000000000000, -0.000000000000000000 ) ) ;
#48660 = ADVANCED_FACE ( 'NONE', ( #17039 ), #35688, .F. ) ;
#48661 = EDGE_LOOP ( 'NONE', ( #36681, #21053, #33790, #42893 ) ) ;
#48662 = ORIENTED_EDGE ( 'NONE', *, *, #13614, .F. ) ;
#48663 = DIRECTION ( 'NONE',  ( 1.734723475976806848E-16, -0.000000000000000000, 1.000000000000000000 ) ) ;
#48664 = B_SPLINE_CURVE_WITH_KNOTS ( 'NONE', 3,
 ( #31149, #43256, #35277, #38891 ),
 .UNSPECIFIED., .F., .F.,
 ( 4, 4 ),
 ( 2.034093849253954962E-05, 0.002520358861215416576 ),
 .UNSPECIFIED. ) ;
#48665 = ORIENTED_EDGE ( 'NONE', *, *, #18268, .T. ) ;
#48666 = DIRECTION ( 'NONE',  ( 1.000000000000000000, 0.000000000000000000, -3.469446951953613696E-16 ) ) ;
#48667 = ORIENTED_EDGE ( 'NONE', *, *, #4623, .T. ) ;
#48668 = AXIS2_PLACEMENT_3D ( 'NONE', #42322, #3596, #3093 ) ;
#48669 = CARTESIAN_POINT ( 'NONE',  ( -2.362204724409449952, 1.172985819482486702, -6.724448087328469681E-16 ) ) ;
#48670 = AXIS2_PLACEMENT_3D ( 'NONE', #44368, #9011, #21143 ) ;
#48671 = ADVANCED_FACE ( 'NONE', ( #35182 ), #31825, .F. ) ;
#48672 = ORIENTED_EDGE ( 'NONE', *, *, #9241, .T. ) ;
#48673 = DIRECTION ( 'NONE',  ( 1.734723475976806848E-16, -0.000000000000000000, 1.000000000000000000 ) ) ;
#48674 = PLANE ( 'NONE',  #21515 ) ;
#48675 = ORIENTED_EDGE ( 'NONE', *, *, #6815, .F. ) ;
#48676 = EDGE_CURVE ( 'NONE', #47661, #38330, #12194, .T. ) ;
#48677 = PLANE ( 'NONE',  #5935 ) ;
#48678 = ORIENTED_EDGE ( 'NONE', *, *, #4123, .F. ) ;
#48679 = AXIS2_PLACEMENT_3D ( 'NONE', #37619, #17986, #2743 ) ;
#48680 = ORIENTED_EDGE ( 'NONE', *, *, #38720, .F. ) ;
#48681 = EDGE_CURVE ( 'NONE', #6600, #15817, #19673, .T. ) ;
#48682 = ORIENTED_EDGE ( 'NONE', *, *, #44854, .F. ) ;
#48683 = EDGE_LOOP ( 'NONE', ( #5410, #25586, #832, #13691 ) ) ;
#48684 = CARTESIAN_POINT ( 'NONE',  ( 0.08119777152254364916, 1.623385212329073957, 0.000000000000000000 ) ) ;
#48685 = B_SPLINE_CURVE_WITH_KNOTS ( 'NONE', 3,
 ( #26781, #34297, #37917, #6915 ),
 .UNSPECIFIED., .F., .F.,
 ( 4, 4 ),
 ( 0.001575154832295005101, 0.004075306633636652590 ),
 .UNSPECIFIED. ) ;
#48686 = ORIENTED_EDGE ( 'NONE', *, *, #15522, .F. ) ;
#48687 = DIRECTION ( 'NONE',  ( 0.000000000000000000, -1.000000000000000000, 0.000000000000000000 ) ) ;
#48688 = EDGE_CURVE ( 'NONE', #45405, #14632, #40783, .T. ) ;
#48689 = VERTEX_POINT ( 'NONE', #9537 ) ;
#48690 = DIRECTION ( 'NONE',  ( -0.000000000000000000, 1.000000000000000000, -0.000000000000000000 ) ) ;
#48691 = DIRECTION ( 'NONE',  ( 0.000000000000000000, -1.000000000000000000, 0.000000000000000000 ) ) ;
#48692 = ORIENTED_EDGE ( 'NONE', *, *, #49935, .T. ) ;
#48693 = CARTESIAN_POINT ( 'NONE',  ( 0.8227799331039050701, 5.905511811023623991, 2.052232022298799752 ) ) ;
#48694 = CARTESIAN_POINT ( 'NONE',  ( -2.164823134740035737, 1.574811347331577016, -0.04796011690018289753 ) ) ;
#48695 = VERTEX_POINT ( 'NONE', #43672 ) ;
#48696 = DIRECTION ( 'NONE',  ( -0.1785568947986370392, -1.142009442734629415E-16, 0.9839295885986295565 ) ) ;
#48697 = LINE ( 'NONE', #28348, #3537 ) ;
#48698 = ADVANCED_FACE ( 'NONE', ( #29150 ), #32794, .T. ) ;
#48699 = AXIS2_PLACEMENT_3D ( 'NONE', #45908, #35075, #31202 ) ;
#48700 = DIRECTION ( 'NONE',  ( -0.000000000000000000, 1.000000000000000000, -0.000000000000000000 ) ) ;
#48701 = EDGE_CURVE ( 'NONE', #28908, #6809, #39289, .T. ) ;
#48702 = LINE ( 'NONE', #45358, #47862 ) ;
#48703 = AXIS2_PLACEMENT_3D ( 'NONE', #50215, #18778, #19272 ) ;
#48704 = VECTOR ( 'NONE', #13987, 39.37007874015748143 ) ;
#48705 = DIRECTION ( 'NONE',  ( 0.000000000000000000, -1.000000000000000000, 0.000000000000000000 ) ) ;
#48706 = VERTEX_POINT ( 'NONE', #17291 ) ;
#48707 = LINE ( 'NONE', #16755, #46013 ) ;
#48708 = CARTESIAN_POINT ( 'NONE',  ( -1.636583440222563635, 3.346456692913386100, 1.259842519685033357 ) ) ;
#48709 = ORIENTED_EDGE ( 'NONE', *, *, #17643, .F. ) ;
#48710 = CARTESIAN_POINT ( 'NONE',  ( 2.081842287654605883, 3.245535198059565030, -1.299212598425194320 ) ) ;
#48711 = CIRCLE ( 'NONE', #42949, 2.246510896728926010 ) ;
#48712 = ORIENTED_EDGE ( 'NONE', *, *, #39480, .T. ) ;
#48713 = CARTESIAN_POINT ( 'NONE',  ( 0.2727639067037610499, 3.346456692913386100, 1.417322834645662777 ) ) ;
#48714 = EDGE_CURVE ( 'NONE', #13413, #17741, #15562, .T. ) ;
#48715 = DIRECTION ( 'NONE',  ( 1.000000000000000000, 0.000000000000000000, 0.000000000000000000 ) ) ;
#48716 = VECTOR ( 'NONE', #26961, 39.37007874015748143 ) ;
#48717 = DIRECTION ( 'NONE',  ( 1.160706738777443955E-16, 1.000000000000000000, -5.589669052740684758E-17 ) ) ;
#48718 = DIRECTION ( 'NONE',  ( 1.734723475976806848E-16, -0.000000000000000000, 1.000000000000000000 ) ) ;
#48719 = DIRECTION ( 'NONE',  ( 0.000000000000000000, 1.000000000000000000, 0.000000000000000000 ) ) ;
#48720 = ORIENTED_EDGE ( 'NONE', *, *, #32471, .T. ) ;
#48721 = EDGE_CURVE ( 'NONE', #37350, #11567, #47005, .T. ) ;
#48722 = CARTESIAN_POINT ( 'NONE',  ( 1.139289024838126441, 1.634917426876648427, -2.479181505015526366 ) ) ;
#48723 = FACE_BOUND ( 'NONE', #48112, .T. ) ;
#48724 = ORIENTED_EDGE ( 'NONE', *, *, #40814, .T. ) ;
#48725 = CARTESIAN_POINT ( 'NONE',  ( -1.597750071202345135, 0.000000000000000000, -0.7364305798568749895 ) ) ;
#48726 = ORIENTED_EDGE ( 'NONE', *, *, #5059, .T. ) ;
#48727 = CARTESIAN_POINT ( 'NONE',  ( 0.000000000000000000, 1.574803149606302854, 0.000000000000000000 ) ) ;
#48728 = FACE_OUTER_BOUND ( 'NONE', #38942, .T. ) ;
#48729 = CARTESIAN_POINT ( 'NONE',  ( -1.675546303352015709, 1.681065010344670041, 1.399148864732502995 ) ) ;
#48730 = CARTESIAN_POINT ( 'NONE',  ( -1.232995795418201812, 0.000000000000000000, 1.780798594093550680 ) ) ;
#48731 = ORIENTED_EDGE ( 'NONE', *, *, #3123, .F. ) ;
#48732 = ORIENTED_EDGE ( 'NONE', *, *, #40000, .T. ) ;
#48733 = CARTESIAN_POINT ( 'NONE',  ( -1.387241876633673598, 1.574803149606302854, 1.662624236931676824 ) ) ;
#48734 = DIRECTION ( 'NONE',  ( 0.000000000000000000, -1.156482317317871478E-16, -1.000000000000000000 ) ) ;
#48735 = FACE_BOUND ( 'NONE', #3194, .T. ) ;
#48736 = ORIENTED_EDGE ( 'NONE', *, *, #7, .F. ) ;
#48737 = B_SPLINE_CURVE_WITH_KNOTS ( 'NONE', 3,
 ( #36100, #44587, #12092, #20857 ),
 .UNSPECIFIED., .F., .F.,
 ( 4, 4 ),
 ( 0.01284703861903681646, 0.03074048250902328486 ),
 .UNSPECIFIED. ) ;
#48738 = VECTOR ( 'NONE', #28994, 39.37007874015748143 ) ;
#48739 = VECTOR ( 'NONE', #45029, 39.37007874015748143 ) ;
#48740 = CARTESIAN_POINT ( 'NONE',  ( -1.662320194739477452, 1.205361022782829114E-17, -1.388601395075575784 ) ) ;
#48741 = CARTESIAN_POINT ( 'NONE',  ( -1.695772546416001392, 1.551146592414875958, -2.417756147381374010 ) ) ;
#48742 = EDGE_CURVE ( 'NONE', #3322, #15064, #15028, .T. ) ;
#48743 = ORIENTED_EDGE ( 'NONE', *, *, #31133, .F. ) ;
#48744 = DIRECTION ( 'NONE',  ( 1.734723475976806848E-16, -0.000000000000000000, 1.000000000000000000 ) ) ;
#48745 = AXIS2_PLACEMENT_3D ( 'NONE', #12511, #23879, #8387 ) ;
#48746 = DIRECTION ( 'NONE',  ( -0.000000000000000000, 0.000000000000000000, 1.000000000000000000 ) ) ;
#48747 = ORIENTED_EDGE ( 'NONE', *, *, #50003, .T. ) ;
#48748 = ORIENTED_EDGE ( 'NONE', *, *, #4272, .F. ) ;
#48749 = CIRCLE ( 'NONE', #1807, 2.165354330708661568 ) ;
#48750 = EDGE_CURVE ( 'NONE', #2388, #25196, #1786, .T. ) ;
#48751 = ORIENTED_EDGE ( 'NONE', *, *, #22784, .T. ) ;
#48752 = DIRECTION ( 'NONE',  ( -0.000000000000000000, 1.000000000000000000, -0.000000000000000000 ) ) ;
#48753 = CONICAL_SURFACE ( 'NONE', #26530, 2.165354330708661568, 0.2617993877991570129 ) ;
#48754 = LINE ( 'NONE', #29435, #11782 ) ;
#48755 = EDGE_CURVE ( 'NONE', #18572, #47436, #26302, .T. ) ;
#48756 = EDGE_CURVE ( 'NONE', #37287, #19191, #33991, .T. ) ;
#48757 = DIRECTION ( 'NONE',  ( 1.734723475976806848E-16, -0.000000000000000000, 1.000000000000000000 ) ) ;
#48758 = DIRECTION ( 'NONE',  ( -0.01601477604151182663, 0.9998717552508123996, -0.000000000000000000 ) ) ;
#48759 = VERTEX_POINT ( 'NONE', #46150 ) ;
#48760 = ORIENTED_EDGE ( 'NONE', *, *, #29732, .T. ) ;
#48761 = PLANE ( 'NONE',  #42261 ) ;
#48762 = DIRECTION ( 'NONE',  ( -0.000000000000000000, -1.000000000000000000, -0.000000000000000000 ) ) ;
#48763 = B_SPLINE_CURVE_WITH_KNOTS ( 'NONE', 3,
 ( #34888, #49572, #18642, #38519 ),
 .UNSPECIFIED., .F., .F.,
 ( 4, 4 ),
 ( 2.655981481195813069E-07, 0.002500437463240591605 ),
 .UNSPECIFIED. ) ;
#48764 = DIRECTION ( 'NONE',  ( -0.000000000000000000, 1.000000000000000000, -0.000000000000000000 ) ) ;
#48765 = EDGE_CURVE ( 'NONE', #50693, #16476, #37427, .T. ) ;
#48766 = DIRECTION ( 'NONE',  ( 1.734723475976806848E-16, 0.000000000000000000, 1.000000000000000000 ) ) ;
#48767 = CARTESIAN_POINT ( 'NONE',  ( -0.8241443283111672402, 1.596276574288824301, 2.055867440327626916 ) ) ;
#48768 = LINE ( 'NONE', #29448, #21004 ) ;
#48769 = PLANE ( 'NONE',  #48932 ) ;
#48770 = ORIENTED_EDGE ( 'NONE', *, *, #41233, .T. ) ;
#48771 = CARTESIAN_POINT ( 'NONE',  ( -1.636583440222563635, 3.346456692913386100, 0.7480314960629874665 ) ) ;
#48772 = LINE ( 'NONE', #36694, #12860 ) ;
#48773 = ORIENTED_EDGE ( 'NONE', *, *, #48241, .T. ) ;
#48775 = EDGE_CURVE ( 'NONE', #23942, #35864, #26045, .T. ) ;
#48774 = ORIENTED_EDGE ( 'NONE', *, *, #13908, .F. ) ;
#48776 = DIRECTION ( 'NONE',  ( 0.000000000000000000, 0.000000000000000000, -1.000000000000000000 ) ) ;
#48777 = AXIS2_PLACEMENT_3D ( 'NONE', #39067, #31074, #39321 ) ;
#48778 = DIRECTION ( 'NONE',  ( 0.000000000000000000, -1.000000000000000000, 0.000000000000000000 ) ) ;
#48779 = VERTEX_POINT ( 'NONE', #41799 ) ;
#48780 = EDGE_CURVE ( 'NONE', #5399, #16323, #48988, .T. ) ;
#48781 = VECTOR ( 'NONE', #3435, 39.37007874015748143 ) ;
#48782 = EDGE_CURVE ( 'NONE', #6227, #31182, #2049, .T. ) ;
#48783 = ORIENTED_EDGE ( 'NONE', *, *, #43202, .F. ) ;
#48784 = CARTESIAN_POINT ( 'NONE',  ( -0.5455278134075214336, 0.000000000000000000, 2.204724409448808764 ) ) ;
#48785 = VERTEX_POINT ( 'NONE', #18302 ) ;
#48786 = VECTOR ( 'NONE', #42028, 39.37007874015748143 ) ;
#48787 = CARTESIAN_POINT ( 'NONE',  ( -1.363819533518803029, 3.346456692913386100, 0.7874015748031456541 ) ) ;
#48788 = PLANE ( 'NONE',  #42843 ) ;
#48789 = ORIENTED_EDGE ( 'NONE', *, *, #36691, .T. ) ;
#48790 = ORIENTED_EDGE ( 'NONE', *, *, #5685, .F. ) ;
#48791 = ORIENTED_EDGE ( 'NONE', *, *, #17590, .T. ) ;
#48792 = CARTESIAN_POINT ( 'NONE',  ( 0.2727639067037604947, 0.000000000000000000, 0.1574803149606283648 ) ) ;
#48793 = ORIENTED_EDGE ( 'NONE', *, *, #25382, .T. ) ;
#48794 = ORIENTED_EDGE ( 'NONE', *, *, #24220, .T. ) ;
#48795 = LINE ( 'NONE', #34118, #4224 ) ;
#48796 = CARTESIAN_POINT ( 'NONE',  ( 0.000000000000000000, 3.346456692913386100, 0.000000000000000000 ) ) ;
#48797 = PLANE ( 'NONE',  #49080 ) ;
#48798 = ORIENTED_EDGE ( 'NONE', *, *, #25483, .F. ) ;
#48799 = DIRECTION ( 'NONE',  ( -0.000000000000000000, 1.000000000000000000, -0.000000000000000000 ) ) ;
#48800 = DIRECTION ( 'NONE',  ( 0.9998717552508121775, 0.01601477604151182663, 0.000000000000000000 ) ) ;
#48801 = LINE ( 'NONE', #44958, #25338 ) ;
#48802 = ORIENTED_EDGE ( 'NONE', *, *, #43442, .F. ) ;
#48803 = LINE ( 'NONE', #10120, #16662 ) ;
#48804 = CARTESIAN_POINT ( 'NONE',  ( 1.560669927219590747, 3.267716535433071279, 1.414498409778230492 ) ) ;
#48805 = CARTESIAN_POINT ( 'NONE',  ( -1.636583440222563635, 3.267716535433071279, 2.839019714148966584E-16 ) ) ;
#48806 = ORIENTED_EDGE ( 'NONE', *, *, #9074, .F. ) ;
#48807 = EDGE_LOOP ( 'NONE', ( #16895, #15805, #2510, #30971 ) ) ;
#48808 =( NAMED_UNIT ( * ) SI_UNIT ( $, .STERADIAN. ) SOLID_ANGLE_UNIT ( ) );
#48810 = CIRCLE ( 'NONE', #26588, 2.246510896728926010 ) ;
#48809 = CARTESIAN_POINT ( 'NONE',  ( 0.000000000000000000, 3.267716535433071279, 2.165354330708650465 ) ) ;
#48811 = ADVANCED_FACE ( 'NONE', ( #42047 ), #6176, .F. ) ;
#48812 = EDGE_CURVE ( 'NONE', #22659, #14850, #45637, .T. ) ;
#48813 = LINE ( 'NONE', #45215, #3864 ) ;
#48814 = LINE ( 'NONE', #45469, #9025 ) ;
#48815 = VERTEX_POINT ( 'NONE', #38191 ) ;
#48817 = EDGE_CURVE ( 'NONE', #19132, #39563, #10048, .T. ) ;
#48816 = ORIENTED_EDGE ( 'NONE', *, *, #32831, .F. ) ;
#48818 = VECTOR ( 'NONE', #46341, 39.37007874015748143 ) ;
#48819 = LINE ( 'NONE', #16872, #21781 ) ;
#48820 = CIRCLE ( 'NONE', #21674, 1.850107469027523432 ) ;
#48821 = ORIENTED_EDGE ( 'NONE', *, *, #31680, .F. ) ;
#48822 = DIRECTION ( 'NONE',  ( -1.000000000000000000, 0.000000000000000000, 0.000000000000000000 ) ) ;
#48823 = DIRECTION ( 'NONE',  ( 1.000000000000000000, 0.000000000000000000, 0.000000000000000000 ) ) ;
#48824 = VECTOR ( 'NONE', #29243, 39.37007874015748143 ) ;
#48825 = VECTOR ( 'NONE', #49017, 39.37007874015748143 ) ;
#48826 = DIRECTION ( 'NONE',  ( 0.01601477604151182663, -0.9998717552508123996, 0.000000000000000000 ) ) ;
#48827 = CARTESIAN_POINT ( 'NONE',  ( 1.775400203342704986, 1.746929418358725172, -2.359903268218703332 ) ) ;
#48828 = LINE ( 'NONE', #1377, #12202 ) ;
#48829 = VERTEX_POINT ( 'NONE', #30174 ) ;
#48830 = FACE_OUTER_BOUND ( 'NONE', #47190, .T. ) ;
#48831 = EDGE_CURVE ( 'NONE', #48458, #19314, #33813, .T. ) ;
#48832 = CARTESIAN_POINT ( 'NONE',  ( 0.3136974817028393425, 1.724153038295522800, -2.936457595020219635 ) ) ;
#48833 = VERTEX_POINT ( 'NONE', #21927 ) ;
#48834 = DIRECTION ( 'NONE',  ( 0.000000000000000000, -1.000000000000000000, 0.000000000000000000 ) ) ;
#48835 = EDGE_CURVE ( 'NONE', #40451, #20168, #10558, .T. ) ;
#48836 = LINE ( 'NONE', #13269, #2243 ) ;
#48837 = LINE ( 'NONE', #45238, #48531 ) ;
#48838 = VERTEX_POINT ( 'NONE', #5667 ) ;
#48839 = CARTESIAN_POINT ( 'NONE',  ( 0.000000000000000000, 6.692913385826772199, 0.000000000000000000 ) ) ;
#48840 = EDGE_CURVE ( 'NONE', #47624, #784, #13927, .T. ) ;
#48841 = DIRECTION ( 'NONE',  ( -0.000000000000000000, 1.000000000000000000, -0.000000000000000000 ) ) ;
#48842 = EDGE_CURVE ( 'NONE', #50859, #19026, #10301, .T. ) ;
#48843 = EDGE_LOOP ( 'NONE', ( #4079, #33456, #19922, #36894 ) ) ;
#48844 = CARTESIAN_POINT ( 'NONE',  ( -2.150793259809249847, 1.575027863729615341, -0.2506944975021367372 ) ) ;
#48845 = CARTESIAN_POINT ( 'NONE',  ( 0.04921259842519682542, 0.5249316475426857309, 1.883403453246504933 ) ) ;
#48846 = EDGE_LOOP ( 'NONE', ( #49006, #25917, #5358, #9410 ) ) ;
#48847 = CARTESIAN_POINT ( 'NONE',  ( 0.5455278134075217666, 0.000000000000000000, 1.889763779527550369 ) ) ;
#48848 = DIRECTION ( 'NONE',  ( -0.000000000000000000, -1.000000000000000000, -0.000000000000000000 ) ) ;
#48849 = DIRECTION ( 'NONE',  ( -0.000000000000000000, 1.000000000000000000, -0.000000000000000000 ) ) ;
#48850 = CYLINDRICAL_SURFACE ( 'NONE', #48240, 2.165354330708661568 ) ;
#48851 = CARTESIAN_POINT ( 'NONE',  ( 0.4696143004045484903, 3.267716535433071279, 1.102362204724404160 ) ) ;
#48852 = AXIS2_PLACEMENT_3D ( 'NONE', #23821, #32347, #39821 ) ;
#48853 = ORIENTED_EDGE ( 'NONE', *, *, #40295, .F. ) ;
#48854 = ORIENTED_EDGE ( 'NONE', *, *, #34854, .T. ) ;
#48855 = CARTESIAN_POINT ( 'NONE',  ( -0.5455278134075208785, 3.346456692913386100, 1.259842519685033357 ) ) ;
#48856 = CARTESIAN_POINT ( 'NONE',  ( -1.363819533518803029, 0.000000000000000000, 1.102362204724404160 ) ) ;
#48857 = ORIENTED_EDGE ( 'NONE', *, *, #46475, .T. ) ;
#48858 = CARTESIAN_POINT ( 'NONE',  ( -0.5455278134075212115, 3.267716535433071279, 9.463399047163220715E-17 ) ) ;
#48859 = CARTESIAN_POINT ( 'NONE',  ( 0.000000000000000000, 2.755905511811022723, 0.000000000000000000 ) ) ;
#48860 = FACE_OUTER_BOUND ( 'NONE', #17709, .T. ) ;
#48861 = VECTOR ( 'NONE', #28142, 39.37007874015748143 ) ;
#48862 = VECTOR ( 'NONE', #19079, 39.37007874015748143 ) ;
#48863 = VERTEX_POINT ( 'NONE', #30435 ) ;
#48864 = VERTEX_POINT ( 'NONE', #14170 ) ;
#48865 = CARTESIAN_POINT ( 'NONE',  ( -1.743145509346916588, 0.000000000000000000, 0.000000000000000000 ) ) ;
#48866 = CARTESIAN_POINT ( 'NONE',  ( -2.932023289724621673, 1.575122962489508449, 0.3475074887687388259 ) ) ;
#48867 = CARTESIAN_POINT ( 'NONE',  ( -2.491402175429631605, 1.581999109372839385, -1.585592796919542025 ) ) ;
#48868 = EDGE_LOOP ( 'NONE', ( #37808, #13116, #28061, #18253 ) ) ;
#48869 = DIRECTION ( 'NONE',  ( 0.000000000000000000, 1.000000000000000000, 0.000000000000000000 ) ) ;
#48870 = FACE_BOUND ( 'NONE', #8784, .T. ) ;
#48871 = VECTOR ( 'NONE', #48892, 39.37007874015748143 ) ;
#48872 = ORIENTED_EDGE ( 'NONE', *, *, #22057, .F. ) ;
#48873 = FACE_OUTER_BOUND ( 'NONE', #23154, .T. ) ;
#48874 = ORIENTED_EDGE ( 'NONE', *, *, #30685, .F. ) ;
#48875 = ORIENTED_EDGE ( 'NONE', *, *, #452, .T. ) ;
#48876 = CARTESIAN_POINT ( 'NONE',  ( -1.306307708855430905, 0.000000000000000000, -1.226175564698866349 ) ) ;
#48877 = ORIENTED_EDGE ( 'NONE', *, *, #16866, .F. ) ;
#48878 = LINE ( 'NONE', #6329, #29412 ) ;
#48879 = CARTESIAN_POINT ( 'NONE',  ( 0.7115265288965786361, 1.624529684782195282, -2.393174330701326902 ) ) ;
#48880 = ORIENTED_EDGE ( 'NONE', *, *, #10650, .F. ) ;
#48881 = EDGE_CURVE ( 'NONE', #19346, #49275, #10802, .T. ) ;
#48882 = EDGE_CURVE ( 'NONE', #17742, #29343, #25535, .T. ) ;
#48883 = DIRECTION ( 'NONE',  ( -1.000000000000000000, 0.000000000000000000, 1.734723475976806848E-16 ) ) ;
#48884 = CARTESIAN_POINT ( 'NONE',  ( 1.363819533518803695, 3.267716535433071279, 1.732283464566921172 ) ) ;
#48885 = EDGE_CURVE ( 'NONE', #1280, #43842, #16496, .T. ) ;
#48886 = DIRECTION ( 'NONE',  ( 1.000000000000000000, 0.000000000000000000, 0.000000000000000000 ) ) ;
#48887 = FACE_OUTER_BOUND ( 'NONE', #2195, .T. ) ;
#48888 = VECTOR ( 'NONE', #29160, 39.37007874015748143 ) ;
#48889 = CARTESIAN_POINT ( 'NONE',  ( -1.679154924913551783, 0.000000000000000000, 0.4938453199301923724 ) ) ;
#48890 = DIRECTION ( 'NONE',  ( 0.9998717552508121775, 0.01601477604151182663, 0.000000000000000000 ) ) ;
#48891 = EDGE_LOOP ( 'NONE', ( #17349, #27886, #46761, #28977 ) ) ;
#48892 = DIRECTION ( 'NONE',  ( 0.000000000000000000, 1.000000000000000000, -0.000000000000000000 ) ) ;
#48893 = VECTOR ( 'NONE', #35735, 39.37007874015748143 ) ;
#48894 = DIRECTION ( 'NONE',  ( -3.986037398843765983E-20, -1.000000000000000000, -1.160734090543304660E-16 ) ) ;
#48895 = CIRCLE ( 'NONE', #30810, 2.165354330708661568 ) ;
#48896 = VECTOR ( 'NONE', #27268, 39.37007874015748143 ) ;
#48897 = ORIENTED_EDGE ( 'NONE', *, *, #40176, .F. ) ;
#48898 = CARTESIAN_POINT ( 'NONE',  ( 2.106197740627112402, 3.267716535433071279, -7.307341331430322647E-16 ) ) ;
#48899 = EDGE_CURVE ( 'NONE', #39780, #28095, #41293, .T. ) ;
#48900 = DIRECTION ( 'NONE',  ( -8.021399753802198224E-17, -1.000000000000000000, 8.389726389140549123E-17 ) ) ;
#48901 = VERTEX_POINT ( 'NONE', #19553 ) ;
#48902 = LINE ( 'NONE', #2223, #37061 ) ;
#48903 = LINE ( 'NONE', #17715, #12637 ) ;
#48904 = DIRECTION ( 'NONE',  ( -0.01601477604151182663, 0.9998717552508123996, -0.000000000000000000 ) ) ;
#48905 = VECTOR ( 'NONE', #7288, 39.37007874015748143 ) ;
#48906 = ADVANCED_FACE ( 'NONE', ( #39442 ), #7442, .F. ) ;
#48907 = ORIENTED_EDGE ( 'NONE', *, *, #34767, .F. ) ;
#48908 = DIRECTION ( 'NONE',  ( -3.469446951953613696E-16, 0.000000000000000000, -1.000000000000000000 ) ) ;
#48909 = VERTEX_POINT ( 'NONE', #43298 ) ;
#48910 = FACE_BOUND ( 'NONE', #31443, .T. ) ;
#48911 = CARTESIAN_POINT ( 'NONE',  ( -1.195183497228115035E-16, 0.000000000000000000, 0.6299212598425161236 ) ) ;
#48912 = DIRECTION ( 'NONE',  ( -0.9998717552508121775, -0.01601477604151182316, 0.000000000000000000 ) ) ;
#48913 = LINE ( 'NONE', #37356, #34258 ) ;
#48914 = VERTEX_POINT ( 'NONE', #35321 ) ;
#48915 = ORIENTED_EDGE ( 'NONE', *, *, #36057, .F. ) ;
#48916 = LINE ( 'NONE', #40466, #22979 ) ;
#48917 = ORIENTED_EDGE ( 'NONE', *, *, #34238, .T. ) ;
#48918 = CARTESIAN_POINT ( 'NONE',  ( -0.2727639067037602172, 0.000000000000000000, 1.417322834645662777 ) ) ;
#48919 = VERTEX_POINT ( 'NONE', #27301 ) ;
#48920 = CARTESIAN_POINT ( 'NONE',  ( 1.966928503432568975, 3.267716535433071279, 0.9055118110236164419 ) ) ;
#48921 = ORIENTED_EDGE ( 'NONE', *, *, #5901, .T. ) ;
#48922 = CARTESIAN_POINT ( 'NONE',  ( -1.930190994932096782, 0.000000000000000000, -0.9827944786818723077 ) ) ;
#48923 = VECTOR ( 'NONE', #139, 39.37007874015748143 ) ;
#48924 = CARTESIAN_POINT ( 'NONE',  ( -0.3486774197067339376, 3.346456692913386100, 2.137096964226333107 ) ) ;
#48925 = AXIS2_PLACEMENT_3D ( 'NONE', #33071, #13437, #33325 ) ;
#48926 = ORIENTED_EDGE ( 'NONE', *, *, #39929, .F. ) ;
#48927 = CARTESIAN_POINT ( 'NONE',  ( -0.04921259842519708216, 1.612473435230266317, 2.479391863569011090 ) ) ;
#48928 = VECTOR ( 'NONE', #35868, 39.37007874015748854 ) ;
#48929 = ORIENTED_EDGE ( 'NONE', *, *, #48782, .F. ) ;
#48930 = ORIENTED_EDGE ( 'NONE', *, *, #3839, .F. ) ;
#48931 = VECTOR ( 'NONE', #3995, 39.37007874015748143 ) ;
#48932 = AXIS2_PLACEMENT_3D ( 'NONE', #44922, #5706, #37207 ) ;
#48933 = VERTEX_POINT ( 'NONE', #15939 ) ;
#48934 = ORIENTED_EDGE ( 'NONE', *, *, #34488, .F. ) ;
#48935 = CARTESIAN_POINT ( 'NONE',  ( 0.000000000000000000, 3.346456692913386100, 0.000000000000000000 ) ) ;
#48936 = EDGE_CURVE ( 'NONE', #22636, #18363, #27557, .T. ) ;
#48937 = AXIS2_PLACEMENT_3D ( 'NONE', #29962, #11351, #6217 ) ;
#48938 = EDGE_CURVE ( 'NONE', #12593, #13726, #7690, .T. ) ;
#48939 = ORIENTED_EDGE ( 'NONE', *, *, #9702, .T. ) ;
#48940 = CARTESIAN_POINT ( 'NONE',  ( -0.07591351300297284610, 3.267716535433071279, 1.220472440944875281 ) ) ;
#48941 = ORIENTED_EDGE ( 'NONE', *, *, #13029, .F. ) ;
#48942 = DIRECTION ( 'NONE',  ( 0.8660254037844431485, 0.000000000000000000, 0.4999999999999918954 ) ) ;
#48943 = ADVANCED_FACE ( 'NONE', ( #23180 ), #35572, .T. ) ;
#48944 = ADVANCED_FACE ( 'NONE', ( #34562 ), #38934, .F. ) ;
#48945 = EDGE_CURVE ( 'NONE', #32953, #41924, #36806, .T. ) ;
#48946 = CARTESIAN_POINT ( 'NONE',  ( 0.1067246931122726866, 0.02962905676920215767, 0.000000000000000000 ) ) ;
#48947 = ORIENTED_EDGE ( 'NONE', *, *, #28101, .T. ) ;
#48948 = CARTESIAN_POINT ( 'NONE',  ( -1.091055626815042645, 3.267716535433071279, 1.889763779527550147 ) ) ;
#48949 = DIRECTION ( 'NONE',  ( 0.9998717552508121775, 0.01601477604151182663, 0.000000000000000000 ) ) ;
#48950 = ORIENTED_EDGE ( 'NONE', *, *, #21245, .F. ) ;
#48951 = CARTESIAN_POINT ( 'NONE',  ( -2.182111253630085290, 3.346456692913386100, -6.146657985744592735E-16 ) ) ;
#48952 = CARTESIAN_POINT ( 'NONE',  ( 0.1968503937007872462, 3.346456692913386100, -1.456692913385822630 ) ) ;
#48953 = CARTESIAN_POINT ( 'NONE',  ( -1.909347346926324906, 0.000000000000000000, 1.220472440944875059 ) ) ;
#48954 = LINE ( 'NONE', #21637, #40534 ) ;
#48955 = DIRECTION ( 'NONE',  ( 1.000000000000000000, -0.000000000000000000, 0.000000000000000000 ) ) ;
#48956 = ADVANCED_FACE ( 'NONE', ( #22682 ), #31497, .F. ) ;
#48957 = ORIENTED_EDGE ( 'NONE', *, *, #32499, .T. ) ;
#48958 = DIRECTION ( 'NONE',  ( -0.000000000000000000, 1.000000000000000000, -0.000000000000000000 ) ) ;
#48959 = CARTESIAN_POINT ( 'NONE',  ( 0.000000000000000000, 3.267716535433071279, 0.9448818897637749625 ) ) ;
#48960 = B_SPLINE_CURVE_WITH_KNOTS ( 'NONE', 3,
 ( #2050, #45389, #10051, #25792 ),
 .UNSPECIFIED., .F., .F.,
 ( 4, 4 ),
 ( 0.0002761238990249075508, 0.003451782018764085365 ),
 .UNSPECIFIED. ) ;
#48961 = B_SPLINE_CURVE_WITH_KNOTS ( 'NONE', 3,
 ( #31498, #20116, #19608, #35378 ),
 .UNSPECIFIED., .F., .F.,
 ( 4, 4 ),
 ( 6.288086478203287970E-07, 0.002380327432043047396 ),
 .UNSPECIFIED. ) ;
#48962 = VERTEX_POINT ( 'NONE', #23690 ) ;
#48963 = DIRECTION ( 'NONE',  ( -0.000000000000000000, 1.000000000000000000, -0.000000000000000000 ) ) ;
#48964 = AXIS2_PLACEMENT_3D ( 'NONE', #47552, #7845, #347 ) ;
#48965 = ADVANCED_FACE ( 'NONE', ( #3820 ), #19299, .F. ) ;
#48966 = CONICAL_SURFACE ( 'NONE', #4489, 3.033577403570480779, 1.554780866114618743 ) ;
#48967 = ORIENTED_EDGE ( 'NONE', *, *, #31514, .T. ) ;
#48968 = CARTESIAN_POINT ( 'NONE',  ( 0.1910111227923183275, 0.000000000000000000, -1.940223436340324570 ) ) ;
#48969 = VECTOR ( 'NONE', #43284, 39.37007874015748143 ) ;
#48971 = AXIS2_PLACEMENT_3D ( 'NONE', #25203, #8436, #39930 ) ;
#48970 = FACE_OUTER_BOUND ( 'NONE', #28910, .T. ) ;
#48972 = CARTESIAN_POINT ( 'NONE',  ( 2.378961647330872786, 3.267716535433071279, 0.1181102362204698858 ) ) ;
#48973 = B_SPLINE_CURVE_WITH_KNOTS ( 'NONE', 3,
 ( #30334, #11904, #15773, #46056 ),
 .UNSPECIFIED., .F., .F.,
 ( 4, 4 ),
 ( 0.1211775127643062860, 0.1625894504277921315 ),
 .UNSPECIFIED. ) ;
#48974 = FACE_OUTER_BOUND ( 'NONE', #35270, .T. ) ;
#48975 = PLANE ( 'NONE',  #49127 ) ;
#48976 = ORIENTED_EDGE ( 'NONE', *, *, #50626, .F. ) ;
#48977 = ADVANCED_FACE ( 'NONE', ( #15445 ), #47140, .F. ) ;
#48978 = CARTESIAN_POINT ( 'NONE',  ( 0.2727639067037609943, 0.000000000000000000, 1.535433070866133898 ) ) ;
#48979 = VECTOR ( 'NONE', #43975, 39.37007874015748143 ) ;
#48980 = PLANE ( 'NONE',  #19648 ) ;
#48981 = DIRECTION ( 'NONE',  ( 1.000000000000000000, 0.000000000000000000, -3.469446951953613696E-16 ) ) ;
#48982 = ORIENTED_EDGE ( 'NONE', *, *, #9203, .F. ) ;
#48983 = CARTESIAN_POINT ( 'NONE',  ( -1.598711713507984022, 1.574803149606302854, -1.460438370699401522 ) ) ;
#48984 = CARTESIAN_POINT ( 'NONE',  ( -1.909347346926324906, 3.267716535433071279, -1.102362204724405492 ) ) ;
#48985 = EDGE_CURVE ( 'NONE', #18498, #44838, #46395, .T. ) ;
#48986 = ORIENTED_EDGE ( 'NONE', *, *, #30089, .F. ) ;
#48987 = DIRECTION ( 'NONE',  ( 1.734723475976806848E-16, 0.000000000000000000, 1.000000000000000000 ) ) ;
#48988 = LINE ( 'NONE', #14430, #168 ) ;
#48989 = CARTESIAN_POINT ( 'NONE',  ( 1.083598637574781920, 1.736150426126270130, 2.747180975113346246 ) ) ;
#48990 = ORIENTED_EDGE ( 'NONE', *, *, #24034, .F. ) ;
#48991 = ORIENTED_EDGE ( 'NONE', *, *, #47467, .T. ) ;
#48992 = CARTESIAN_POINT ( 'NONE',  ( 1.287906020515830585, 3.346456692913386100, 1.740706023381843659 ) ) ;
#48993 = FACE_OUTER_BOUND ( 'NONE', #33736, .T. ) ;
#48994 = FACE_BOUND ( 'NONE', #32921, .T. ) ;
#48995 = LINE ( 'NONE', #21938, #36933 ) ;
#48996 = CARTESIAN_POINT ( 'NONE',  ( -0.6214413264104945434, 3.346456692913386100, -2.047244094488181343 ) ) ;
#48997 = ORIENTED_EDGE ( 'NONE', *, *, #1438, .F. ) ;
#48998 = ORIENTED_EDGE ( 'NONE', *, *, #40487, .F. ) ;
#48999 = DIRECTION ( 'NONE',  ( 0.7530714660036196273, 1.288287287306305530E-16, -0.6579387259397027066 ) ) ;
#49000 = AXIS2_PLACEMENT_3D ( 'NONE', #9829, #45165, #5180 ) ;
#49001 = CARTESIAN_POINT ( 'NONE',  ( -2.153807523435207649, 5.905511811023623991, 0.2420910006175677753 ) ) ;
#49002 = ORIENTED_EDGE ( 'NONE', *, *, #41792, .F. ) ;
#49003 = ORIENTED_EDGE ( 'NONE', *, *, #17510, .T. ) ;
#49004 = B_SPLINE_CURVE_WITH_KNOTS ( 'NONE', 3,
 ( #23587, #39336, #35468, #47294 ),
 .UNSPECIFIED., .F., .F.,
 ( 4, 4 ),
 ( 2.002016769723030562E-07, 0.002500200812166948009 ),
 .UNSPECIFIED. ) ;
#49005 = AXIS2_PLACEMENT_3D ( 'NONE', #50668, #14866, #30609 ) ;
#49006 = ORIENTED_EDGE ( 'NONE', *, *, #23698, .T. ) ;
#49007 = CARTESIAN_POINT ( 'NONE',  ( -1.166969139818015977, 3.346456692913386100, -1.732283464566922726 ) ) ;
#49008 = EDGE_CURVE ( 'NONE', #6577, #2835, #3310, .T. ) ;
#49009 = CARTESIAN_POINT ( 'NONE',  ( -2.695799277629577162, 1.571269479597534824, -1.205759334241492731 ) ) ;
#49010 = EDGE_CURVE ( 'NONE', #3513, #46251, #23429, .T. ) ;
#49011 = DIRECTION ( 'NONE',  ( -0.9998717552508121775, -0.01601477604151182663, 0.000000000000000000 ) ) ;
#49012 = EDGE_CURVE ( 'NONE', #12583, #10448, #19805, .T. ) ;
#49013 = CARTESIAN_POINT ( 'NONE',  ( -1.709950266952966036, 0.000000000000000000, -0.3398067978735320183 ) ) ;
#49014 = ORIENTED_EDGE ( 'NONE', *, *, #50626, .T. ) ;
#49015 = EDGE_LOOP ( 'NONE', ( #39904, #33710, #32341, #12765 ) ) ;
#49016 = AXIS2_PLACEMENT_3D ( 'NONE', #27373, #10882, #43115 ) ;
#49017 = DIRECTION ( 'NONE',  ( -0.000000000000000000, 1.000000000000000000, -0.000000000000000000 ) ) ;
#49018 = CARTESIAN_POINT ( 'NONE',  ( -1.363819533518803473, 3.346456692913386100, -0.6692913385826760875 ) ) ;
#49019 = CARTESIAN_POINT ( 'NONE',  ( 2.152441353505198940, 6.692913385826772199, -0.2419059403264808283 ) ) ;
#49020 = DIRECTION ( 'NONE',  ( 0.4338837391175656699, 1.045612331811453550E-16, -0.9009688679024154823 ) ) ;
#49021 = LINE ( 'NONE', #13705, #21051 ) ;
#49022 = FACE_OUTER_BOUND ( 'NONE', #42067, .T. ) ;
#49023 = ORIENTED_EDGE ( 'NONE', *, *, #37072, .F. ) ;
#49024 = DIRECTION ( 'NONE',  ( -0.9998717552508122886, -0.01601477604151185785, 0.000000000000000000 ) ) ;
#49025 = FACE_OUTER_BOUND ( 'NONE', #14146, .T. ) ;
#49026 = ORIENTED_EDGE ( 'NONE', *, *, #39906, .T. ) ;
#49027 = VERTEX_POINT ( 'NONE', #50998 ) ;
#49028 = LINE ( 'NONE', #29457, #28219 ) ;
#49029 = DIRECTION ( 'NONE',  ( -3.469446951953613696E-16, 0.000000000000000000, -1.000000000000000000 ) ) ;
#49030 = VERTEX_POINT ( 'NONE', #15689 ) ;
#49031 = EDGE_CURVE ( 'NONE', #9971, #44436, #11811, .T. ) ;
#49032 = VECTOR ( 'NONE', #50771, 39.37007874015748143 ) ;
#49033 = VECTOR ( 'NONE', #36065, 39.37007874015748143 ) ;
#49034 = VERTEX_POINT ( 'NONE', #36341 ) ;
#49035 = AXIS2_PLACEMENT_3D ( 'NONE', #34347, #18846, #22717 ) ;
#49036 = CARTESIAN_POINT ( 'NONE',  ( 0.4696143004045484903, 0.000000000000000000, 1.417322834645662777 ) ) ;
#49037 = EDGE_CURVE ( 'NONE', #19985, #1980, #20124, .T. ) ;
#49038 = AXIS2_PLACEMENT_3D ( 'NONE', #8825, #305, #31819 ) ;
#49039 = ORIENTED_EDGE ( 'NONE', *, *, #22861, .F. ) ;
#49040 = CARTESIAN_POINT ( 'NONE',  ( 1.015142113812069313, 3.267716535433071279, -0.6692913385826764205 ) ) ;
#49041 = DIRECTION ( 'NONE',  ( -3.469446951953613696E-16, 0.000000000000000000, -1.000000000000000000 ) ) ;
#49042 = EDGE_CURVE ( 'NONE', #17416, #12576, #20821, .T. ) ;
#49043 = VERTEX_POINT ( 'NONE', #44326 ) ;
#49044 = ORIENTED_EDGE ( 'NONE', *, *, #45823, .T. ) ;
#49045 = VECTOR ( 'NONE', #30104, 39.37007874015748143 ) ;
#49046 = CARTESIAN_POINT ( 'NONE',  ( -1.405314191946755997, 1.685393272164901646, 1.683309666213049560 ) ) ;
#49047 = ORIENTED_EDGE ( 'NONE', *, *, #26702, .T. ) ;
#49048 = VERTEX_POINT ( 'NONE', #48418 ) ;
#49049 = ADVANCED_FACE ( 'NONE', ( #20844 ), #24465, .F. ) ;
#49050 = CARTESIAN_POINT ( 'NONE',  ( 2.110884035022549732, 1.741711621820001943, -0.9557545615714394538 ) ) ;
#49051 = CARTESIAN_POINT ( 'NONE',  ( 1.901071203648723618, 1.705542687144442571, -1.313853494766966223 ) ) ;
#49052 = FACE_OUTER_BOUND ( 'NONE', #44583, .T. ) ;
#49053 = ADVANCED_FACE ( 'NONE', ( #13106 ), #8972, .F. ) ;
#49054 = ORIENTED_EDGE ( 'NONE', *, *, #29128, .T. ) ;
#49055 = DIRECTION ( 'NONE',  ( 0.000000000000000000, 0.000000000000000000, 1.000000000000000000 ) ) ;
#49056 = DIRECTION ( 'NONE',  ( -0.000000000000000000, 1.000000000000000000, -0.000000000000000000 ) ) ;
#49057 = CARTESIAN_POINT ( 'NONE',  ( 2.168245791271197209, 1.753049777144058297, -2.004968704497248844 ) ) ;
#49058 = ORIENTED_EDGE ( 'NONE', *, *, #39791, .F. ) ;
#49059 = DIRECTION ( 'NONE',  ( 0.9195277725514489076, 0.000000000000000000, 0.3930250316539278810 ) ) ;
#49060 = PLANE ( 'NONE',  #13720 ) ;
#49061 = DIRECTION ( 'NONE',  ( -1.000000000000000000, 0.000000000000000000, 0.000000000000000000 ) ) ;
#49062 = EDGE_LOOP ( 'NONE', ( #12177, #14515, #44210, #43773 ) ) ;
#49063 = VERTEX_POINT ( 'NONE', #20057 ) ;
#49064 = ADVANCED_FACE ( 'NONE', ( #36086 ), #38945, .T. ) ;
#49065 = CARTESIAN_POINT ( 'NONE',  ( 0.1968503937007872462, 3.346456692913386100, 0.1181102362204701633 ) ) ;
#49066 = DIRECTION ( 'NONE',  ( 0.000000000000000000, 0.7071067811865482389, 0.7071067811865467956 ) ) ;
#49067 = EDGE_CURVE ( 'NONE', #536, #48466, #44574, .T. ) ;
#49068 = EDGE_CURVE ( 'NONE', #13102, #38331, #17234, .T. ) ;
#49069 = PLANE ( 'NONE',  #19732 ) ;
#49070 = ORIENTED_EDGE ( 'NONE', *, *, #37125, .F. ) ;
#49071 = ORIENTED_EDGE ( 'NONE', *, *, #24355, .F. ) ;
#49072 = COLOUR_RGB ( '',0.7921568627450980005, 0.8196078431372548767, 0.9333333333333333481 ) ;
#49073 = ADVANCED_FACE ( 'NONE', ( #35827 ), #9223, .F. ) ;
#49074 = AXIS2_PLACEMENT_3D ( 'NONE', #14859, #27221, #6609 ) ;
#49075 = CARTESIAN_POINT ( 'NONE',  ( -1.812531910417308101, 1.588581096961242389, 1.999811551830815715 ) ) ;
#49076 = VERTEX_POINT ( 'NONE', #44070 ) ;
#49077 = DIRECTION ( 'NONE',  ( -0.000000000000000000, 1.000000000000000000, -0.000000000000000000 ) ) ;
#49078 = CARTESIAN_POINT ( 'NONE',  ( 1.833433833923351353, 3.267716535433071279, 0.3149606299212576177 ) ) ;
#49079 = VECTOR ( 'NONE', #38126, 39.37007874015748143 ) ;
#49080 = AXIS2_PLACEMENT_3D ( 'NONE', #41356, #37493, #2111 ) ;
#49081 = EDGE_CURVE ( 'NONE', #46932, #10831, #454, .T. ) ;
#49082 = CARTESIAN_POINT ( 'NONE',  ( 0.8182917201112819283, 0.000000000000000000, 0.1574803149606286423 ) ) ;
#49083 = CARTESIAN_POINT ( 'NONE',  ( -0.8329809839909440017, 1.205361022782829114E-17, -2.833254665166566877 ) ) ;
#49084 = DIRECTION ( 'NONE',  ( 0.01601477604151182663, -0.9998717552508123996, 0.000000000000000000 ) ) ;
#49085 = CIRCLE ( 'NONE', #30153, 2.165354330708661568 ) ;
#49086 = ORIENTED_EDGE ( 'NONE', *, *, #48004, .T. ) ;
#49087 = CARTESIAN_POINT ( 'NONE',  ( 0.1067246931122726866, 0.02962905676920215767, 0.000000000000000000 ) ) ;
#49088 = CARTESIAN_POINT ( 'NONE',  ( 2.106197740627112402, 3.346456692913386100, 1.102362204724403938 ) ) ;
#49089 = CARTESIAN_POINT ( 'NONE',  ( 0.7423782071083087075, 3.346456692913386100, -1.259842519685035134 ) ) ;
#49090 = VERTEX_POINT ( 'NONE', #43557 ) ;
#49091 = CARTESIAN_POINT ( 'NONE',  ( -1.627052366890036739, 1.591492494466993923, -2.155719988184307212 ) ) ;
#49092 = DIRECTION ( 'NONE',  ( -1.000000000000000000, -0.000000000000000000, -0.000000000000000000 ) ) ;
#49093 = LINE ( 'NONE', #33414, #35384 ) ;
#49094 = VERTEX_POINT ( 'NONE', #43811 ) ;
#49095 = EDGE_CURVE ( 'NONE', #4027, #5831, #8458, .T. ) ;
#49096 = CARTESIAN_POINT ( 'NONE',  ( -0.2727639067037603837, 3.267716535433071279, 4.731699523581606660E-17 ) ) ;
#49097 = CARTESIAN_POINT ( 'NONE',  ( -0.8182917201112814842, 3.267716535433071279, 1.220472440944875281 ) ) ;
#49098 = ORIENTED_EDGE ( 'NONE', *, *, #35119, .F. ) ;
#49099 = LINE ( 'NONE', #13785, #22232 ) ;
#49100 = FACE_OUTER_BOUND ( 'NONE', #28131, .T. ) ;
#49101 = ORIENTED_EDGE ( 'NONE', *, *, #37087, .F. ) ;
#49102 = CARTESIAN_POINT ( 'NONE',  ( -1.971247363764855320, 1.574803149606302854, -0.8960709840011922278 ) ) ;
#49103 = EDGE_CURVE ( 'NONE', #19688, #3143, #37447, .T. ) ;
#49104 = DIRECTION ( 'NONE',  ( 0.000000000000000000, 1.000000000000000000, 0.000000000000000000 ) ) ;
#49105 = CARTESIAN_POINT ( 'NONE',  ( 0.000000000000000000, 3.267716535433071279, -1.417322834645664331 ) ) ;
#49106 = CARTESIAN_POINT ( 'NONE',  ( 1.833791099076603537, 1.574803149606302854, -1.151507526013694216 ) ) ;
#49107 = ADVANCED_FACE ( 'NONE', ( #28320 ), #5350, .F. ) ;
#49108 = EDGE_CURVE ( 'NONE', #47112, #21738, #15862, .T. ) ;
#49109 = CIRCLE ( 'NONE', #11231, 1.743387098533651480 ) ;
#49110 = EDGE_CURVE ( 'NONE', #30179, #35447, #47655, .T. ) ;
#49111 = CARTESIAN_POINT ( 'NONE',  ( -2.353647019958005071, 1.172985819482486924, -0.9842519685039374799 ) ) ;
#49112 = ORIENTED_EDGE ( 'NONE', *, *, #12627, .T. ) ;
#49113 = ORIENTED_EDGE ( 'NONE', *, *, #44830, .T. ) ;
#49114 = DIRECTION ( 'NONE',  ( -0.9998717552508121775, -0.01601477604151182663, 0.000000000000000000 ) ) ;
#49115 = VECTOR ( 'NONE', #19008, 39.37007874015748143 ) ;
#49116 = LINE ( 'NONE', #29542, #35365 ) ;
#49117 = AXIS2_PLACEMENT_3D ( 'NONE', #33010, #34016, #33518 ) ;
#49118 = EDGE_LOOP ( 'NONE', ( #46452, #8811, #28276, #19418 ) ) ;
#49119 = CARTESIAN_POINT ( 'NONE',  ( 1.300279662861326013, 0.04874602395362847423, 1.413491677621213860 ) ) ;
#49120 = LINE ( 'NONE', #13292, #10434 ) ;
#49121 = PLANE ( 'NONE',  #20340 ) ;
#49122 = VECTOR ( 'NONE', #18430, 39.37007874015748143 ) ;
#49123 = ORIENTED_EDGE ( 'NONE', *, *, #20504, .T. ) ;
#49124 = EDGE_LOOP ( 'NONE', ( #14982, #44487 ) ) ;
#49125 = CARTESIAN_POINT ( 'NONE',  ( 4.268512490100411402E-16, 0.000000000000000000, 1.889763779527550369 ) ) ;
#49126 = DIRECTION ( 'NONE',  ( 0.7660444431189771253, 0.6427876096865404731, 2.214792131866782686E-16 ) ) ;
#49127 = AXIS2_PLACEMENT_3D ( 'NONE', #41030, #24766, #9269 ) ;
#49128 = CARTESIAN_POINT ( 'NONE',  ( 1.833433833923351797, 3.267716535433071279, -6.361001426714001438E-16 ) ) ;
#49129 = ORIENTED_EDGE ( 'NONE', *, *, #34360, .F. ) ;
#49130 = CYLINDRICAL_SURFACE ( 'NONE', #8396, 1.181102362204723200 ) ;
#49132 = AXIS2_PLACEMENT_3D ( 'NONE', #49934, #2497, #14107 ) ;
#49131 = FACE_OUTER_BOUND ( 'NONE', #47841, .T. ) ;
#49133 = ORIENTED_EDGE ( 'NONE', *, *, #5065, .F. ) ;
#49134 = LINE ( 'NONE', #49633, #32367 ) ;
#49135 = ORIENTED_EDGE ( 'NONE', *, *, #15936, .F. ) ;
#49136 = ORIENTED_EDGE ( 'NONE', *, *, #38218, .T. ) ;
#49137 = EDGE_CURVE ( 'NONE', #4890, #20741, #20588, .T. ) ;
#49138 = CARTESIAN_POINT ( 'NONE',  ( 0.1968503937007878568, 3.267716535433071279, 1.259842519685033357 ) ) ;
#49139 = PLANE ( 'NONE',  #45626 ) ;
#49140 = EDGE_CURVE ( 'NONE', #2123, #39618, #17736, .T. ) ;
#49141 = EDGE_LOOP ( 'NONE', ( #37132, #49847, #567, #39047 ) ) ;
#49142 = LINE ( 'NONE', #21819, #22817 ) ;
#49143 = EDGE_CURVE ( 'NONE', #37431, #4542, #21610, .T. ) ;
#49144 = CARTESIAN_POINT ( 'NONE',  ( 1.526828301548457834, 3.346456692913386100, 1.535433070866133898 ) ) ;
#49145 = VERTEX_POINT ( 'NONE', #49687 ) ;
#49146 = EDGE_CURVE ( 'NONE', #34665, #13554, #37370, .T. ) ;
#49147 = CARTESIAN_POINT ( 'NONE',  ( 0.1968503937007870241, 3.267716535433071279, -2.204724409448811429 ) ) ;
#49148 = DIRECTION ( 'NONE',  ( 0.000000000000000000, -1.000000000000000000, 0.000000000000000000 ) ) ;
#49149 = CONICAL_SURFACE ( 'NONE', #26913, 2.165354330708661568, 0.2617993877991570129 ) ;
#49150 = PLANE ( 'NONE',  #8276 ) ;
#49151 = CARTESIAN_POINT ( 'NONE',  ( -0.5455278134075208785, 0.000000000000000000, 1.574803149606291974 ) ) ;
#49152 = LINE ( 'NONE', #18464, #40223 ) ;
#49153 = VECTOR ( 'NONE', #49709, 39.37007874015748143 ) ;
#49154 = ORIENTED_EDGE ( 'NONE', *, *, #5334, .F. ) ;
#49155 = DIRECTION ( 'NONE',  ( 1.734723475976806848E-16, -0.000000000000000000, 1.000000000000000000 ) ) ;
#49156 = AXIS2_PLACEMENT_3D ( 'NONE', #2204, #45288, #21319 ) ;
#49157 = B_SPLINE_CURVE_WITH_KNOTS ( 'NONE', 3,
 ( #16349, #44467, #4981, #36997 ),
 .UNSPECIFIED., .F., .F.,
 ( 4, 4 ),
 ( 0.1211873102087489551, 0.1625992483279400380 ),
 .UNSPECIFIED. ) ;
#49158 = DIRECTION ( 'NONE',  ( 0.9998717552508121775, 0.01601477604151182663, 0.000000000000000000 ) ) ;
#49159 = ORIENTED_EDGE ( 'NONE', *, *, #19461, .T. ) ;
#49160 = DIRECTION ( 'NONE',  ( -0.000000000000000000, -1.000000000000000000, -0.000000000000000000 ) ) ;
#49161 = DIRECTION ( 'NONE',  ( -3.986037398843765983E-20, -1.000000000000000000, -1.160734090543304660E-16 ) ) ;
#49162 = ORIENTED_EDGE ( 'NONE', *, *, #17462, .T. ) ;
#49163 = CARTESIAN_POINT ( 'NONE',  ( 2.378961647330872786, 0.000000000000000000, -1.161035397307311917E-15 ) ) ;
#49164 = AXIS2_PLACEMENT_3D ( 'NONE', #21313, #13564, #5814 ) ;
#49165 = DIRECTION ( 'NONE',  ( 1.000000000000000000, 0.000000000000000000, 0.000000000000000000 ) ) ;
#49166 = CARTESIAN_POINT ( 'NONE',  ( -0.8182917201112815953, 3.267716535433071279, 1.419509857074482553E-16 ) ) ;
#49167 = VECTOR ( 'NONE', #14298, 39.37007874015748143 ) ;
#49168 = ORIENTED_EDGE ( 'NONE', *, *, #34159, .T. ) ;
#49169 = CARTESIAN_POINT ( 'NONE',  ( 1.636583440222563857, 0.000000000000000000, -0.6299212598425181220 ) ) ;
#49170 = VERTEX_POINT ( 'NONE', #29087 ) ;
#49171 = FACE_BOUND ( 'NONE', #44425, .T. ) ;
#49172 = DIRECTION ( 'NONE',  ( -3.469446951953613696E-16, 0.000000000000000000, -1.000000000000000000 ) ) ;
#49173 = LINE ( 'NONE', #37355, #22666 ) ;
#49174 = CARTESIAN_POINT ( 'NONE',  ( 0.1968503937007870241, 0.000000000000000000, -2.204724409448811429 ) ) ;
#49175 = EDGE_CURVE ( 'NONE', #45835, #46993, #41238, .T. ) ;
#49176 = B_SPLINE_CURVE_WITH_KNOTS ( 'NONE', 3,
 ( #39589, #39332, #7344, #19198 ),
 .UNSPECIFIED., .F., .F.,
 ( 4, 4 ),
 ( 0.1211873102087489551, 0.1625992483279400103 ),
 .UNSPECIFIED. ) ;
#49177 = ADVANCED_FACE ( 'NONE', ( #1986 ), #38150, .F. ) ;
#49178 = ORIENTED_EDGE ( 'NONE', *, *, #23210, .T. ) ;
#49179 = ORIENTED_EDGE ( 'NONE', *, *, #35866, .T. ) ;
#49180 = EDGE_CURVE ( 'NONE', #5543, #18782, #45328, .T. ) ;
#49181 = CARTESIAN_POINT ( 'NONE',  ( 0.9914495361338625523, 1.636256239573039117, 2.781765111341823360 ) ) ;
#49182 = ORIENTED_EDGE ( 'NONE', *, *, #43117, .F. ) ;
#49183 = CARTESIAN_POINT ( 'NONE',  ( -0.5455278134075214336, 0.000000000000000000, -8.878505979408855953E-16 ) ) ;
#49184 = ORIENTED_EDGE ( 'NONE', *, *, #11264, .F. ) ;
#49185 = CARTESIAN_POINT ( 'NONE',  ( 0.6507993007407579800, 1.619900495825837838, -2.173134161263437392 ) ) ;
#49186 = ORIENTED_EDGE ( 'NONE', *, *, #25973, .F. ) ;
#49187 = DIRECTION ( 'NONE',  ( -0.000000000000000000, 1.000000000000000000, -0.000000000000000000 ) ) ;
#49188 = AXIS2_PLACEMENT_3D ( 'NONE', #36762, #5770, #14025 ) ;
#49189 = CARTESIAN_POINT ( 'NONE',  ( 2.389170071857189992, 1.752995279934814965, 1.341552826535246545 ) ) ;
#49190 = AXIS2_PLACEMENT_3D ( 'NONE', #3724, #50403, #7351 ) ;
#49191 = VERTEX_POINT ( 'NONE', #38132 ) ;
#49192 = CARTESIAN_POINT ( 'NONE',  ( 0.000000000000000000, 3.267716535433071279, 1.535433070866133898 ) ) ;
#49193 = EDGE_LOOP ( 'NONE', ( #15554, #25730, #11012, #49446 ) ) ;
#49194 = ORIENTED_EDGE ( 'NONE', *, *, #28557, .F. ) ;
#49195 = ADVANCED_FACE ( 'NONE', ( #33500 ), #18499, .F. ) ;
#49196 = EDGE_CURVE ( 'NONE', #38185, #44444, #25475, .T. ) ;
#49197 = VERTEX_POINT ( 'NONE', #33243 ) ;
#49198 = ORIENTED_EDGE ( 'NONE', *, *, #48412, .F. ) ;
#49199 = LINE ( 'NONE', #22388, #5485 ) ;
#49200 = EDGE_CURVE ( 'NONE', #2091, #15789, #10498, .T. ) ;
#49201 = ORIENTED_EDGE ( 'NONE', *, *, #21282, .F. ) ;
#49203 = CARTESIAN_POINT ( 'NONE',  ( 0.1968503937007869686, 3.267716535433071279, -2.401574803149598480 ) ) ;
#49202 = VECTOR ( 'NONE', #26009, 39.37007874015748854 ) ;
#49204 = EDGE_CURVE ( 'NONE', #48261, #19363, #26242, .T. ) ;
#49205 = LINE ( 'NONE', #36874, #16172 ) ;
#49206 = CARTESIAN_POINT ( 'NONE',  ( 2.011396482730577251, 0.9928247669144205645, 1.666980445438335234 ) ) ;
#49207 = B_SPLINE_CURVE_WITH_KNOTS ( 'NONE', 3,
 ( #27991, #20244, #36009, #12504 ),
 .UNSPECIFIED., .F., .F.,
 ( 4, 4 ),
 ( 0.1211873102087489551, 0.1625992483279400380 ),
 .UNSPECIFIED. ) ;
#49208 = ORIENTED_EDGE ( 'NONE', *, *, #14066, .T. ) ;
#49209 = CARTESIAN_POINT ( 'NONE',  ( 0.1968503937007873017, 0.000000000000000000, -1.259842519685035134 ) ) ;
#49210 = CARTESIAN_POINT ( 'NONE',  ( 2.100403847690402337, 3.346456692913386100, 0.1574803149606280872 ) ) ;
#49211 = ORIENTED_EDGE ( 'NONE', *, *, #36503, .T. ) ;
#49212 = DIRECTION ( 'NONE',  ( -1.000000000000000000, -0.000000000000000000, -0.000000000000000000 ) ) ;
#49213 = DIRECTION ( 'NONE',  ( -1.000000000000000000, -0.000000000000000000, -0.000000000000000000 ) ) ;
#49214 = CARTESIAN_POINT ( 'NONE',  ( -0.8329809839909436686, 1.706281419137876565, -2.833254665166566877 ) ) ;
#49215 = CARTESIAN_POINT ( 'NONE',  ( 2.164658444855302122, 5.905511811023623991, -0.04795272066889885720 ) ) ;
#49216 = CARTESIAN_POINT ( 'NONE',  ( 0.4788131938641113083, 0.000000000000000000, 2.914091152102192162 ) ) ;
#49217 = CARTESIAN_POINT ( 'NONE',  ( -1.739713118882874276, 4.162957430336159157E-05, 0.1138408270437312325 ) ) ;
#49218 = VERTEX_POINT ( 'NONE', #2502 ) ;
#49219 = CARTESIAN_POINT ( 'NONE',  ( 0.2727639067037604392, 3.346456692913386100, 0.2755905511810994302 ) ) ;
#49220 = VECTOR ( 'NONE', #48294, 39.37007874015748143 ) ;
#49221 = VECTOR ( 'NONE', #30729, 39.37007874015748143 ) ;
#49222 = DIRECTION ( 'NONE',  ( 1.000000000000000000, -0.000000000000000000, 0.000000000000000000 ) ) ;
#49223 = ORIENTED_EDGE ( 'NONE', *, *, #39222, .F. ) ;
#49224 = DIRECTION ( 'NONE',  ( 1.734723475976806848E-16, -0.000000000000000000, 1.000000000000000000 ) ) ;
#49225 = ORIENTED_EDGE ( 'NONE', *, *, #38920, .F. ) ;
#49226 = FACE_OUTER_BOUND ( 'NONE', #31293, .T. ) ;
#49227 = CARTESIAN_POINT ( 'NONE',  ( 0.2727639067037604392, 0.000000000000000000, -0.03937007874015908959 ) ) ;
#49228 = LINE ( 'NONE', #13910, #653 ) ;
#49229 = FACE_OUTER_BOUND ( 'NONE', #16015, .T. ) ;
#49230 = CARTESIAN_POINT ( 'NONE',  ( 0.000000000000000000, 0.000000000000000000, 0.000000000000000000 ) ) ;
#49231 = ORIENTED_EDGE ( 'NONE', *, *, #41594, .T. ) ;
#49232 = B_SPLINE_CURVE_WITH_KNOTS ( 'NONE', 3,
 ( #50691, #15886, #47343, #12021 ),
 .UNSPECIFIED., .F., .F.,
 ( 4, 4 ),
 ( 0.0002011623507270493549, 0.04991335192709614454 ),
 .UNSPECIFIED. ) ;
#49233 = DIRECTION ( 'NONE',  ( -0.7530714660036099684, 7.639920857896035043E-17, -0.6579387259397138088 ) ) ;
#49234 = EDGE_CURVE ( 'NONE', #28604, #16977, #13358, .T. ) ;
#49235 = EDGE_LOOP ( 'NONE', ( #28874, #37231, #33499, #41606 ) ) ;
#49236 = EDGE_CURVE ( 'NONE', #19595, #23409, #9989, .T. ) ;
#49237 = CARTESIAN_POINT ( 'NONE',  ( -2.348444893129629563, 1.580171291669419276, 1.319637673352544338 ) ) ;
#49238 = ORIENTED_EDGE ( 'NONE', *, *, #38399, .F. ) ;
#49239 = PLANE ( 'NONE',  #42768 ) ;
#49240 = CARTESIAN_POINT ( 'NONE',  ( -1.091055626815042201, 3.346456692913386100, 1.574803149606291974 ) ) ;
#49241 = EDGE_CURVE ( 'NONE', #45327, #35692, #2323, .T. ) ;
#49242 = ORIENTED_EDGE ( 'NONE', *, *, #30690, .F. ) ;
#49243 = ADVANCED_FACE ( 'NONE', ( #29865 ), #25227, .F. ) ;
#49244 = CARTESIAN_POINT ( 'NONE',  ( -1.636583440222563635, 0.000000000000000000, 0.9448818897637749625 ) ) ;
#49245 = DIRECTION ( 'NONE',  ( 1.734723475976806848E-16, -0.000000000000000000, 1.000000000000000000 ) ) ;
#49246 = EDGE_CURVE ( 'NONE', #6476, #15435, #34001, .T. ) ;
#49247 = DIRECTION ( 'NONE',  ( -0.000000000000000000, 0.000000000000000000, 1.000000000000000000 ) ) ;
#49248 = ORIENTED_EDGE ( 'NONE', *, *, #6224, .T. ) ;
#49249 = ORIENTED_EDGE ( 'NONE', *, *, #2407, .F. ) ;
#49250 = DIRECTION ( 'NONE',  ( 0.000000000000000000, 1.000000000000000000, -1.156482317317871478E-16 ) ) ;
#49251 = FACE_BOUND ( 'NONE', #8407, .T. ) ;
#49252 = ORIENTED_EDGE ( 'NONE', *, *, #42644, .F. ) ;
#49253 = CARTESIAN_POINT ( 'NONE',  ( 1.636583440222563857, 3.346456692913386100, 1.259842519685033135 ) ) ;
#49254 = EDGE_CURVE ( 'NONE', #5100, #2988, #11742, .T. ) ;
#49255 = DIRECTION ( 'NONE',  ( -3.469446951953613696E-16, 0.000000000000000000, -1.000000000000000000 ) ) ;
#49256 = EDGE_CURVE ( 'NONE', #22312, #9751, #1729, .T. ) ;
#49257 = AXIS2_PLACEMENT_3D ( 'NONE', #18163, #14545, #38305 ) ;
#49258 = CIRCLE ( 'NONE', #26231, 2.164630168518208109 ) ;
#49259 = EDGE_LOOP ( 'NONE', ( #46287, #39522, #15365, #17142 ) ) ;
#49260 = ORIENTED_EDGE ( 'NONE', *, *, #33906, .F. ) ;
#49261 = CARTESIAN_POINT ( 'NONE',  ( -1.636583440222563635, 3.346456692913386100, 0.1181102362204704270 ) ) ;
#49262 = LINE ( 'NONE', #1552, #45158 ) ;
#49263 = EDGE_CURVE ( 'NONE', #44079, #22183, #14368, .T. ) ;
#49264 = ORIENTED_EDGE ( 'NONE', *, *, #9348, .T. ) ;
#49265 = ORIENTED_EDGE ( 'NONE', *, *, #33020, .F. ) ;
#49266 = AXIS2_PLACEMENT_3D ( 'NONE', #40281, #24010, #16529 ) ;
#49267 = ORIENTED_EDGE ( 'NONE', *, *, #12256, .F. ) ;
#49268 = DIRECTION ( 'NONE',  ( -1.000000000000000000, 0.000000000000000000, -0.000000000000000000 ) ) ;
#49269 = DIRECTION ( 'NONE',  ( -0.000000000000000000, 1.000000000000000000, -0.000000000000000000 ) ) ;
#49270 = CONICAL_SURFACE ( 'NONE', #16444, 3.033577403570480779, 1.554780866114618743 ) ;
#49271 = DIRECTION ( 'NONE',  ( -1.000000000000000000, 0.000000000000000000, -0.000000000000000000 ) ) ;
#49272 = CARTESIAN_POINT ( 'NONE',  ( -0.2727639067037607723, 3.346456692913386100, -1.102362204724405714 ) ) ;
#49273 = CIRCLE ( 'NONE', #44362, 2.246510896728926010 ) ;
#49274 = ORIENTED_EDGE ( 'NONE', *, *, #13485, .T. ) ;
#49275 = VERTEX_POINT ( 'NONE', #23370 ) ;
#49276 = LINE ( 'NONE', #34342, #48825 ) ;
#49277 = LINE ( 'NONE', #42319, #3907 ) ;
#49278 = DIRECTION ( 'NONE',  ( -3.469446951953613696E-16, 0.000000000000000000, -1.000000000000000000 ) ) ;
#49279 = EDGE_CURVE ( 'NONE', #36035, #27704, #18322, .T. ) ;
#49280 = FACE_OUTER_BOUND ( 'NONE', #29965, .T. ) ;
#49281 = LINE ( 'NONE', #29704, #50308 ) ;
#49282 = CARTESIAN_POINT ( 'NONE',  ( -0.5455278134075214336, 3.346456692913386100, -1.771653543307081025 ) ) ;
#49283 = DIRECTION ( 'NONE',  ( 1.734723475976806848E-16, -0.000000000000000000, 1.000000000000000000 ) ) ;
#49284 = VERTEX_POINT ( 'NONE', #38876 ) ;
#49285 = PLANE ( 'NONE',  #43178 ) ;
#49286 = DIRECTION ( 'NONE',  ( 0.000000000000000000, 0.000000000000000000, -1.000000000000000000 ) ) ;
#49287 = VERTEX_POINT ( 'NONE', #46836 ) ;
#49288 = VERTEX_POINT ( 'NONE', #11257 ) ;
#49289 = CARTESIAN_POINT ( 'NONE',  ( 0.000000000000000000, 3.346456692913386100, 0.000000000000000000 ) ) ;
#49290 = ORIENTED_EDGE ( 'NONE', *, *, #40263, .T. ) ;
#49291 = EDGE_CURVE ( 'NONE', #19894, #30240, #30881, .T. ) ;
#49292 = ORIENTED_EDGE ( 'NONE', *, *, #19003, .T. ) ;
#49293 = DIRECTION ( 'NONE',  ( 1.734723475976806848E-16, -0.000000000000000000, 1.000000000000000000 ) ) ;
#49294 = AXIS2_PLACEMENT_3D ( 'NONE', #25423, #43562, #8215 ) ;
#49295 = EDGE_LOOP ( 'NONE', ( #1272, #28989, #3891, #44576 ) ) ;
#49296 = EDGE_CURVE ( 'NONE', #34006, #22659, #11509, .T. ) ;
#49297 = AXIS2_PLACEMENT_3D ( 'NONE', #49125, #13551, #29801 ) ;
#49298 = AXIS2_PLACEMENT_3D ( 'NONE', #7798, #23537, #43150 ) ;
#49299 = DIRECTION ( 'NONE',  ( -3.469446951953613696E-16, 0.000000000000000000, -1.000000000000000000 ) ) ;
#49300 = CARTESIAN_POINT ( 'NONE',  ( 0.000000000000000000, 0.000000000000000000, 0.000000000000000000 ) ) ;
#49301 = EDGE_CURVE ( 'NONE', #10548, #6479, #7386, .T. ) ;
#49302 = EDGE_CURVE ( 'NONE', #43953, #23181, #35258, .T. ) ;
#49303 = VECTOR ( 'NONE', #19512, 39.37007874015748143 ) ;
#49304 = ORIENTED_EDGE ( 'NONE', *, *, #13344, .F. ) ;
#49305 = ORIENTED_EDGE ( 'NONE', *, *, #7985, .T. ) ;
#49306 = DIRECTION ( 'NONE',  ( -0.000000000000000000, 1.000000000000000000, -0.000000000000000000 ) ) ;
#49307 = ORIENTED_EDGE ( 'NONE', *, *, #40776, .T. ) ;
#49308 = ORIENTED_EDGE ( 'NONE', *, *, #16257, .F. ) ;
#49309 = CARTESIAN_POINT ( 'NONE',  ( -0.8429824507881226170, 1.205361022782829114E-17, -1.637047627937372241 ) ) ;
#49310 = DIRECTION ( 'NONE',  ( 0.000000000000000000, -1.000000000000000000, 0.000000000000000000 ) ) ;
#49311 = CARTESIAN_POINT ( 'NONE',  ( 0.2727639067037609943, 0.000000000000000000, 0.9055118110236167750 ) ) ;
#49312 = CONICAL_SURFACE ( 'NONE', #36160, 3.033577403570480779, 1.554780866114618743 ) ;
#49313 = ORIENTED_EDGE ( 'NONE', *, *, #16062, .T. ) ;
#49314 = CIRCLE ( 'NONE', #44405, 2.165354330708661568 ) ;
#49315 = CARTESIAN_POINT ( 'NONE',  ( 0.4696143004045479352, 3.346456692913386100, 0.4724409448818868706 ) ) ;
#49316 = EDGE_CURVE ( 'NONE', #14608, #39550, #31862, .T. ) ;
#49317 = DIRECTION ( 'NONE',  ( -0.000000000000000000, 1.000000000000000000, -0.000000000000000000 ) ) ;
#49318 = CARTESIAN_POINT ( 'NONE',  ( 2.076281802138679300, 3.346456692913386100, -0.3543307086614178592 ) ) ;
#49319 = EDGE_LOOP ( 'NONE', ( #34762, #22804, #2849, #23380 ) ) ;
#49320 = LINE ( 'NONE', #41364, #46323 ) ;
#49321 = LINE ( 'NONE', #2380, #35974 ) ;
#49322 = CARTESIAN_POINT ( 'NONE',  ( -0.4433489891367861091, 6.692913385826772199, 2.167441310503416485 ) ) ;
#49323 = EDGE_CURVE ( 'NONE', #27124, #13102, #27242, .T. ) ;
#49324 = VERTEX_POINT ( 'NONE', #34752 ) ;
#49325 = VERTEX_POINT ( 'NONE', #3508 ) ;
#49326 = DIRECTION ( 'NONE',  ( -3.469446951953613696E-16, 0.000000000000000000, -1.000000000000000000 ) ) ;
#49327 = EDGE_CURVE ( 'NONE', #4522, #10796, #2690, .T. ) ;
#49328 = CARTESIAN_POINT ( 'NONE',  ( -0.07591351300297284610, 0.000000000000000000, 1.535433070866133898 ) ) ;
#49329 = CARTESIAN_POINT ( 'NONE',  ( 0.6233543567505469563, 6.692913385826772199, -2.073689640095370379 ) ) ;
#49330 = ORIENTED_EDGE ( 'NONE', *, *, #13325, .F. ) ;
#49331 = ORIENTED_EDGE ( 'NONE', *, *, #13803, .F. ) ;
#49332 = DIRECTION ( 'NONE',  ( -0.000000000000000000, -1.000000000000000000, -0.000000000000000000 ) ) ;
#49333 = EDGE_LOOP ( 'NONE', ( #11443, #4217, #13297, #45553, #17553, #46644 ) ) ;
#49334 = FACE_OUTER_BOUND ( 'NONE', #50424, .T. ) ;
#49335 = EDGE_CURVE ( 'NONE', #49191, #46791, #15634, .T. ) ;
#49336 = CARTESIAN_POINT ( 'NONE',  ( 1.363819533518803251, 3.267716535433071279, -2.365849761790805487E-16 ) ) ;
#49337 = AXIS2_PLACEMENT_3D ( 'NONE', #3952, #42921, #35449 ) ;
#49338 = VECTOR ( 'NONE', #42842, 39.37007874015748143 ) ;
#49339 = AXIS2_PLACEMENT_3D ( 'NONE', #1567, #24295, #40812 ) ;
#49340 = CARTESIAN_POINT ( 'NONE',  ( -1.087426130748108788, 0.01050254589070086231, -1.412988192946641020 ) ) ;
#49341 = CARTESIAN_POINT ( 'NONE',  ( 1.015142113812069313, 3.346456692913386100, 0.7874015748031454320 ) ) ;
#49342 = FACE_OUTER_BOUND ( 'NONE', #8347, .T. ) ;
#49343 = VERTEX_POINT ( 'NONE', #50435 ) ;
#49344 = CARTESIAN_POINT ( 'NONE',  ( 0.7423782071083092626, 3.346456692913386100, 1.574803149606291974 ) ) ;
#49345 = CARTESIAN_POINT ( 'NONE',  ( -1.363819533518803473, 3.267716535433071279, 2.365849761790805980E-16 ) ) ;
#49346 = EDGE_CURVE ( 'NONE', #35447, #45462, #15385, .T. ) ;
#49347 = VECTOR ( 'NONE', #3923, 39.37007874015748143 ) ;
#49348 = DIRECTION ( 'NONE',  ( 1.734723475976806848E-16, 0.000000000000000000, 1.000000000000000000 ) ) ;
#49349 = ADVANCED_FACE ( 'NONE', ( #3254 ), #7884, .F. ) ;
#49350 = EDGE_LOOP ( 'NONE', ( #32544, #16837, #46892, #2046 ) ) ;
#49351 = DIRECTION ( 'NONE',  ( 1.734723475976806848E-16, -0.000000000000000000, 1.000000000000000000 ) ) ;
#49352 = CARTESIAN_POINT ( 'NONE',  ( 1.636583440222563857, 0.000000000000000000, -0.8267716535433055070 ) ) ;
#49353 = CARTESIAN_POINT ( 'NONE',  ( 0.07982360342473591996, 1.709180471932028711, 0.000000000000000000 ) ) ;
#49354 = ORIENTED_EDGE ( 'NONE', *, *, #34668, .F. ) ;
#49355 = CARTESIAN_POINT ( 'NONE',  ( -2.823445274216743073, 1.576824725690453954, 0.8656477926280276014 ) ) ;
#49356 = ORIENTED_EDGE ( 'NONE', *, *, #18392, .T. ) ;
#49357 = DIRECTION ( 'NONE',  ( 0.000000000000000000, -0.000000000000000000, 1.000000000000000000 ) ) ;
#49358 = DIRECTION ( 'NONE',  ( -0.000000000000000000, -1.000000000000000000, -0.000000000000000000 ) ) ;
#49359 = ORIENTED_EDGE ( 'NONE', *, *, #43892, .T. ) ;
#49360 = LINE ( 'NONE', #46014, #45947 ) ;
#49361 = EDGE_CURVE ( 'NONE', #4073, #7296, #39124, .T. ) ;
#49362 = PLANE ( 'NONE',  #2875 ) ;
#49363 = CARTESIAN_POINT ( 'NONE',  ( 1.636583440222563635, 0.000000000000000000, -1.456692913385823296 ) ) ;
#49364 = DIRECTION ( 'NONE',  ( 1.000000000000000000, -0.000000000000000000, 0.000000000000000000 ) ) ;
#49365 = VECTOR ( 'NONE', #26669, 39.37007874015748143 ) ;
#49366 = EDGE_CURVE ( 'NONE', #36553, #49324, #13411, .T. ) ;
#49367 = PLANE ( 'NONE',  #33771 ) ;
#49368 = EDGE_LOOP ( 'NONE', ( #18112, #28247, #49201, #1314 ) ) ;
#49369 = VERTEX_POINT ( 'NONE', #46589 ) ;
#49370 = CARTESIAN_POINT ( 'NONE',  ( 2.464291103507799008, 0.000000000000000000, -1.626664315311302733 ) ) ;
#49371 = CARTESIAN_POINT ( 'NONE',  ( 0.2727639067037609943, 3.346456692913386100, 1.850393700787392293 ) ) ;
#49372 = ORIENTED_EDGE ( 'NONE', *, *, #50263, .F. ) ;
#49373 = CARTESIAN_POINT ( 'NONE',  ( 1.909347346926324684, 0.000000000000000000, 1.102362204724403938 ) ) ;
#49374 = DIRECTION ( 'NONE',  ( 0.000000000000000000, -1.000000000000000000, 0.000000000000000000 ) ) ;
#49375 = CARTESIAN_POINT ( 'NONE',  ( -0.2727639067037608278, 3.346456692913386100, -1.299212598425193210 ) ) ;
#49376 = ORIENTED_EDGE ( 'NONE', *, *, #20193, .T. ) ;
#49377 = EDGE_LOOP ( 'NONE', ( #39233, #30851, #29790, #28718 ) ) ;
#49378 = DIRECTION ( 'NONE',  ( -0.7660444431189771253, 0.6427876096865404731, 0.000000000000000000 ) ) ;
#49379 = FACE_OUTER_BOUND ( 'NONE', #8281, .T. ) ;
#49380 = CARTESIAN_POINT ( 'NONE',  ( 0.000000000000000000, 3.267716535433071279, 0.5905511811023579360 ) ) ;
#49381 = ORIENTED_EDGE ( 'NONE', *, *, #28762, .T. ) ;
#49382 = VECTOR ( 'NONE', #21522, 39.37007874015748143 ) ;
#49383 = LINE ( 'NONE', #25673, #34749 ) ;
#49384 = FACE_BOUND ( 'NONE', #41482, .T. ) ;
#49385 = ORIENTED_EDGE ( 'NONE', *, *, #50056, .T. ) ;
#49386 = CARTESIAN_POINT ( 'NONE',  ( 0.000000000000000000, 0.4235180831842794702, 1.062992125984251635 ) ) ;
#49387 = VERTEX_POINT ( 'NONE', #42741 ) ;
#49388 = VERTEX_POINT ( 'NONE', #4020 ) ;
#49389 = VECTOR ( 'NONE', #12172, 39.37007874015748143 ) ;
#49390 = DIRECTION ( 'NONE',  ( 1.000000000000000000, 0.000000000000000000, 0.000000000000000000 ) ) ;
#49391 = CARTESIAN_POINT ( 'NONE',  ( 0.002207914879453961969, 5.905511811023623991, 0.04916304461325442243 ) ) ;
#49392 = DIRECTION ( 'NONE',  ( -0.01601477604151182663, 0.9998717552508123996, -0.000000000000000000 ) ) ;
#49394 = ORIENTED_EDGE ( 'NONE', *, *, #7399, .F. ) ;
#49393 = EDGE_CURVE ( 'NONE', #4531, #2803, #23124, .T. ) ;
#49395 = LINE ( 'NONE', #26694, #26094 ) ;
#49396 = DIRECTION ( 'NONE',  ( -1.105928667600717569E-16, 1.000000000000000000, -6.607616187506203079E-17 ) ) ;
#49397 = VERTEX_POINT ( 'NONE', #22620 ) ;
#49398 = DIRECTION ( 'NONE',  ( -1.000000000000000000, -0.000000000000000000, -0.000000000000000000 ) ) ;
#49399 = ADVANCED_FACE ( 'NONE', ( #14627 ), #42251, .T. ) ;
#49400 = CARTESIAN_POINT ( 'NONE',  ( -2.348388583459264822, 1.678599427619271722, 1.319607371826798659 ) ) ;
#49401 = EDGE_CURVE ( 'NONE', #32285, #12432, #46092, .T. ) ;
#49402 = CIRCLE ( 'NONE', #15643, 2.246510896728926010 ) ;
#49403 = EDGE_CURVE ( 'NONE', #19154, #26003, #8144, .T. ) ;
#49404 = CARTESIAN_POINT ( 'NONE',  ( 1.162932091021788183, 1.205361022782829114E-17, -1.684364178081092067 ) ) ;
#49405 = LINE ( 'NONE', #21831, #45115 ) ;
#49406 = FACE_OUTER_BOUND ( 'NONE', #46718, .T. ) ;
#49407 = EDGE_LOOP ( 'NONE', ( #3846, #44014, #40885, #45720, #6061, #50272, #37099, #16224, #46075, #14424, #3925, #19940, #46881, #29530, #48720, #18073, #21431, #47208, #22578, #18181, #15754, #19917, #4768 ) ) ;
#49408 = LINE ( 'NONE', #6343, #12612 ) ;
#49409 = DIRECTION ( 'NONE',  ( -1.000000000000000000, 0.000000000000000000, 1.734723475976806848E-16 ) ) ;
#49410 = VECTOR ( 'NONE', #25560, 39.37007874015748143 ) ;
#49411 = VERTEX_POINT ( 'NONE', #20265 ) ;
#49412 = CYLINDRICAL_SURFACE ( 'NONE', #28106, 2.086614173228346303 ) ;
#49413 = FACE_OUTER_BOUND ( 'NONE', #7006, .T. ) ;
#49414 = ORIENTED_EDGE ( 'NONE', *, *, #49316, .T. ) ;
#49415 = DIRECTION ( 'NONE',  ( 0.000000000000000000, 0.000000000000000000, 1.000000000000000000 ) ) ;
#49416 = EDGE_CURVE ( 'NONE', #6398, #4293, #39635, .T. ) ;
#49417 = CARTESIAN_POINT ( 'NONE',  ( 0.2727639067037610499, 0.000000000000000000, 1.417322834645662777 ) ) ;
#49418 = FACE_OUTER_BOUND ( 'NONE', #2060, .T. ) ;
#49419 = ORIENTED_EDGE ( 'NONE', *, *, #49428, .T. ) ;
#49420 = CARTESIAN_POINT ( 'NONE',  ( 0.8182917201112817063, 0.000000000000000000, -2.244094488188969283 ) ) ;
#49421 = VECTOR ( 'NONE', #11931, 39.37007874015748854 ) ;
#49422 = ORIENTED_EDGE ( 'NONE', *, *, #47032, .F. ) ;
#49423 = DIRECTION ( 'NONE',  ( -0.000000000000000000, 1.000000000000000000, -0.000000000000000000 ) ) ;
#49424 = LINE ( 'NONE', #45564, #45668 ) ;
#49425 = EDGE_CURVE ( 'NONE', #11701, #42898, #7619, .T. ) ;
#49426 = DIRECTION ( 'NONE',  ( -0.000000000000000000, 0.000000000000000000, 1.000000000000000000 ) ) ;
#49427 = FACE_OUTER_BOUND ( 'NONE', #13360, .T. ) ;
#49428 = EDGE_CURVE ( 'NONE', #784, #11828, #27751, .T. ) ;
#49429 = EDGE_CURVE ( 'NONE', #42191, #45506, #48361, .T. ) ;
#49430 = ORIENTED_EDGE ( 'NONE', *, *, #37252, .T. ) ;
#49431 = VERTEX_POINT ( 'NONE', #4266 ) ;
#49432 = FACE_OUTER_BOUND ( 'NONE', #6820, .T. ) ;
#49433 = DIRECTION ( 'NONE',  ( 0.000000000000000000, 0.000000000000000000, 1.000000000000000000 ) ) ;
#49434 = ORIENTED_EDGE ( 'NONE', *, *, #36855, .F. ) ;
#49435 = CARTESIAN_POINT ( 'NONE',  ( -0.8578470342358641698, 1.030463582533445166, 2.425782518084936612 ) ) ;
#49436 = ORIENTED_EDGE ( 'NONE', *, *, #13070, .T. ) ;
#49437 = DIRECTION ( 'NONE',  ( -0.01601477604151182663, 0.9998717552508123996, -0.000000000000000000 ) ) ;
#49438 = DIRECTION ( 'NONE',  ( -0.000000000000000000, 1.000000000000000000, -0.000000000000000000 ) ) ;
#49439 = ORIENTED_EDGE ( 'NONE', *, *, #1463, .T. ) ;
#49440 = DIRECTION ( 'NONE',  ( -3.986037398843765983E-20, -1.000000000000000000, -1.160734090543304660E-16 ) ) ;
#49441 = ORIENTED_EDGE ( 'NONE', *, *, #21895, .F. ) ;
#49442 = ORIENTED_EDGE ( 'NONE', *, *, #24231, .T. ) ;
#49443 = AXIS2_PLACEMENT_3D ( 'NONE', #5626, #38394, #43003 ) ;
#49444 = VECTOR ( 'NONE', #1360, 39.37007874015748143 ) ;
#49445 = VERTEX_POINT ( 'NONE', #28518 ) ;
#49446 = ORIENTED_EDGE ( 'NONE', *, *, #35548, .F. ) ;
#49447 = CARTESIAN_POINT ( 'NONE',  ( -0.7053729475263631477, 3.267716535433071279, 2.047244094488179567 ) ) ;
#49448 = ORIENTED_EDGE ( 'NONE', *, *, #41520, .T. ) ;
#49449 = LINE ( 'NONE', #14386, #11421 ) ;
#49450 = CARTESIAN_POINT ( 'NONE',  ( 0.1968503937007872462, 3.267716535433071279, 0.4330708661417287386 ) ) ;
#49451 = EDGE_CURVE ( 'NONE', #49431, #22488, #44520, .T. ) ;
#49452 = EDGE_CURVE ( 'NONE', #1336, #2180, #44007, .T. ) ;
#49453 = CARTESIAN_POINT ( 'NONE',  ( 1.744867630759598498, 0.5220937483424626935, 1.454430778622096465 ) ) ;
#49454 = EDGE_CURVE ( 'NONE', #13787, #22204, #16665, .T. ) ;
#49455 = CARTESIAN_POINT ( 'NONE',  ( 1.450992585860268136, 0.5222384346921369325, 1.735592794888963120 ) ) ;
#49456 = DIRECTION ( 'NONE',  ( 1.734723475976806848E-16, -0.000000000000000000, 1.000000000000000000 ) ) ;
#49457 = ORIENTED_EDGE ( 'NONE', *, *, #33502, .F. ) ;
#49458 = FACE_OUTER_BOUND ( 'NONE', #1728, .T. ) ;
#49459 = DIRECTION ( 'NONE',  ( 0.000000000000000000, 0.000000000000000000, -1.000000000000000000 ) ) ;
#49460 = CARTESIAN_POINT ( 'NONE',  ( -0.6380732109764247761, 1.697682040615038801, -2.127022210610377773 ) ) ;
#49461 = DIRECTION ( 'NONE',  ( 0.000000000000000000, 0.000000000000000000, -1.000000000000000000 ) ) ;
#49462 = EDGE_CURVE ( 'NONE', #35644, #18957, #1160, .T. ) ;
#49463 = ORIENTED_EDGE ( 'NONE', *, *, #42078, .F. ) ;
#49464 = CARTESIAN_POINT ( 'NONE',  ( 0.08139965876239094178, 1.610780518492231694, 0.000000000000000000 ) ) ;
#49465 = DIRECTION ( 'NONE',  ( 1.000000000000000000, 0.000000000000000000, 0.000000000000000000 ) ) ;
#49466 = ORIENTED_EDGE ( 'NONE', *, *, #7557, .F. ) ;
#49467 = FACE_OUTER_BOUND ( 'NONE', #28404, .T. ) ;
#49468 = FACE_OUTER_BOUND ( 'NONE', #14291, .T. ) ;
#49469 = EDGE_LOOP ( 'NONE', ( #13115, #44495, #31396, #20447 ) ) ;
#49470 = CARTESIAN_POINT ( 'NONE',  ( 1.091055626815043311, 3.346456692913386100, 1.870389530743258755 ) ) ;
#49471 = EDGE_CURVE ( 'NONE', #31195, #26854, #24913, .T. ) ;
#49472 = VERTEX_POINT ( 'NONE', #19999 ) ;
#49473 = DIRECTION ( 'NONE',  ( 0.9998717552508121775, 0.01601477604151182663, 0.000000000000000000 ) ) ;
#49474 = DIRECTION ( 'NONE',  ( 0.000000000000000000, -0.000000000000000000, -1.000000000000000000 ) ) ;
#49475 = VECTOR ( 'NONE', #6071, 39.37007874015748143 ) ;
#49476 = DIRECTION ( 'NONE',  ( -1.000000000000000000, -0.000000000000000000, -0.000000000000000000 ) ) ;
#49477 = EDGE_CURVE ( 'NONE', #47284, #41751, #32678, .T. ) ;
#49478 = VECTOR ( 'NONE', #30416, 39.37007874015748143 ) ;
#49479 = CARTESIAN_POINT ( 'NONE',  ( -0.3486774197067339376, 0.000000000000000000, -8.878505979408855953E-16 ) ) ;
#49480 = DIRECTION ( 'NONE',  ( -0.000000000000000000, 1.000000000000000000, -0.000000000000000000 ) ) ;
#49481 = ORIENTED_EDGE ( 'NONE', *, *, #19037, .T. ) ;
#49482 = EDGE_CURVE ( 'NONE', #42262, #12924, #23312, .T. ) ;
#49483 = CARTESIAN_POINT ( 'NONE',  ( 0.8182917201112819283, 0.000000000000000000, -0.6692913385826764205 ) ) ;
#49484 = ORIENTED_EDGE ( 'NONE', *, *, #2496, .T. ) ;
#49485 = ORIENTED_EDGE ( 'NONE', *, *, #11801, .T. ) ;
#49486 = DIRECTION ( 'NONE',  ( 0.000000000000000000, -1.000000000000000000, 0.000000000000000000 ) ) ;
#49487 = EDGE_CURVE ( 'NONE', #39685, #26900, #33253, .T. ) ;
#49488 = ORIENTED_EDGE ( 'NONE', *, *, #44797, .T. ) ;
#49489 = DIRECTION ( 'NONE',  ( -0.000000000000000000, 0.000000000000000000, 1.000000000000000000 ) ) ;
#49490 = VECTOR ( 'NONE', #40917, 39.37007874015748143 ) ;
#49491 = LINE ( 'NONE', #14167, #50721 ) ;
#49492 = EDGE_CURVE ( 'NONE', #25584, #23451, #47594, .T. ) ;
#49493 = ORIENTED_EDGE ( 'NONE', *, *, #7780, .F. ) ;
#49494 = DIRECTION ( 'NONE',  ( 0.000000000000000000, 0.000000000000000000, 1.000000000000000000 ) ) ;
#49495 = CARTESIAN_POINT ( 'NONE',  ( -0.07591351300297340121, 0.000000000000000000, -0.03937007874015908959 ) ) ;
#49496 = DIRECTION ( 'NONE',  ( 1.734723475976806848E-16, -0.000000000000000000, 1.000000000000000000 ) ) ;
#49497 = ORIENTED_EDGE ( 'NONE', *, *, #44539, .T. ) ;
#49498 = EDGE_LOOP ( 'NONE', ( #48874, #26542, #4046, #13587 ) ) ;
#49499 = CARTESIAN_POINT ( 'NONE',  ( 2.926032761125787029, 0.000000000000000000, 0.3963580683592521914 ) ) ;
#49500 = FACE_BOUND ( 'NONE', #19494, .T. ) ;
#49501 = ORIENTED_EDGE ( 'NONE', *, *, #13789, .T. ) ;
#49502 = CARTESIAN_POINT ( 'NONE',  ( -0.8182917201112819283, 3.267716535433071279, -0.3543307086614175816 ) ) ;
#49503 = DIRECTION ( 'NONE',  ( -1.000000000000000000, 0.000000000000000000, -0.000000000000000000 ) ) ;
#49504 = ORIENTED_EDGE ( 'NONE', *, *, #24053, .F. ) ;
#49505 = ORIENTED_EDGE ( 'NONE', *, *, #1555, .F. ) ;
#49506 = DIRECTION ( 'NONE',  ( 0.000000000000000000, 0.000000000000000000, 1.000000000000000000 ) ) ;
#49507 = CARTESIAN_POINT ( 'NONE',  ( 0.7423782071083087075, 3.267716535433071279, -1.259842519685035134 ) ) ;
#49508 = ORIENTED_EDGE ( 'NONE', *, *, #34789, .T. ) ;
#49509 = ORIENTED_EDGE ( 'NONE', *, *, #10366, .T. ) ;
#49510 = ORIENTED_EDGE ( 'NONE', *, *, #11410, .T. ) ;
#49511 = CARTESIAN_POINT ( 'NONE',  ( 1.015142113812069979, 3.346456692913386100, 2.047244094488179567 ) ) ;
#49512 = AXIS2_PLACEMENT_3D ( 'NONE', #39215, #27586, #19082 ) ;
#49513 = CARTESIAN_POINT ( 'NONE',  ( 0.000000000000000000, 3.267716535433071279, -0.3149606299212596716 ) ) ;
#49514 = VECTOR ( 'NONE', #25992, 39.37007874015748143 ) ;
#49515 = CARTESIAN_POINT ( 'NONE',  ( 2.118006771444148839, 0.000000000000000000, 0.3034726681826900307 ) ) ;
#49516 = CARTESIAN_POINT ( 'NONE',  ( 0.1067246931122726866, 0.02962905676920215767, 0.000000000000000000 ) ) ;
#49517 = EDGE_LOOP ( 'NONE', ( #20261, #12371, #34952, #30960 ) ) ;
#49518 = ORIENTED_EDGE ( 'NONE', *, *, #20544, .F. ) ;
#49519 = EDGE_CURVE ( 'NONE', #1584, #33429, #35510, .T. ) ;
#49520 = DIRECTION ( 'NONE',  ( 0.000000000000000000, 0.000000000000000000, -1.000000000000000000 ) ) ;
#49521 = CARTESIAN_POINT ( 'NONE',  ( -1.439733046521776139, 3.267716535433071279, 0.6299212598425164567 ) ) ;
#49522 = EDGE_CURVE ( 'NONE', #38248, #34706, #47338, .T. ) ;
#49523 = DIRECTION ( 'NONE',  ( -0.000000000000000000, 1.000000000000000000, -0.000000000000000000 ) ) ;
#49524 = CIRCLE ( 'NONE', #20705, 2.165354330708661568 ) ;
#49525 = LINE ( 'NONE', #2337, #32583 ) ;
#49526 = ADVANCED_FACE ( 'NONE', ( #131 ), #15881, .F. ) ;
#49527 = CARTESIAN_POINT ( 'NONE',  ( -0.8952071785065479625, 5.905511811023623991, 1.972340328593135794 ) ) ;
#49528 = VECTOR ( 'NONE', #42205, 39.37007874015748143 ) ;
#49529 = CARTESIAN_POINT ( 'NONE',  ( -2.258024766633058622, 3.346456692913386100, -0.3543307086614173040 ) ) ;
#49530 = CARTESIAN_POINT ( 'NONE',  ( 0.000000000000000000, 3.267716535433071279, 0.1181102362204705658 ) ) ;
#49531 = ORIENTED_EDGE ( 'NONE', *, *, #11349, .T. ) ;
#49532 = CARTESIAN_POINT ( 'NONE',  ( -0.5756566573089004768, 1.710292258889409833, 2.896516654582634853 ) ) ;
#49533 = CARTESIAN_POINT ( 'NONE',  ( 0.7423782071083084855, 0.000000000000000000, -1.889763779527552812 ) ) ;
#49534 = VERTEX_POINT ( 'NONE', #906 ) ;
#49535 = ORIENTED_EDGE ( 'NONE', *, *, #16474, .T. ) ;
#49536 = LINE ( 'NONE', #14981, #32808 ) ;
#49537 = EDGE_CURVE ( 'NONE', #15306, #32210, #40418, .T. ) ;
#49538 = ORIENTED_EDGE ( 'NONE', *, *, #24100, .T. ) ;
#49539 = EDGE_CURVE ( 'NONE', #43566, #17400, #25791, .T. ) ;
#49540 = EDGE_CURVE ( 'NONE', #28392, #30339, #1672, .T. ) ;
#49541 = ORIENTED_EDGE ( 'NONE', *, *, #13638, .F. ) ;
#49542 = CARTESIAN_POINT ( 'NONE',  ( 1.312248418042880171, 6.692913385826772199, -1.722429524498088949 ) ) ;
#49543 = ORIENTED_EDGE ( 'NONE', *, *, #3046, .T. ) ;
#49544 = CIRCLE ( 'NONE', #22400, 1.850107469027523432 ) ;
#49545 = LINE ( 'NONE', #11114, #42486 ) ;
#49546 = CARTESIAN_POINT ( 'NONE',  ( 0.1968503937007870241, 3.267716535433071279, -1.889763779527552146 ) ) ;
#49547 = VECTOR ( 'NONE', #16669, 39.37007874015748143 ) ;
#49548 = ORIENTED_EDGE ( 'NONE', *, *, #4519, .T. ) ;
#49549 = ORIENTED_EDGE ( 'NONE', *, *, #28992, .F. ) ;
#49550 = VECTOR ( 'NONE', #33548, 39.37007874015748143 ) ;
#49551 = CARTESIAN_POINT ( 'NONE',  ( 2.378961647330872786, 3.346456692913386100, 0.3149606299212573401 ) ) ;
#49552 = ORIENTED_EDGE ( 'NONE', *, *, #17468, .T. ) ;
#49553 = ORIENTED_EDGE ( 'NONE', *, *, #44940, .F. ) ;
#49554 = FACE_OUTER_BOUND ( 'NONE', #41213, .T. ) ;
#49555 = FACE_OUTER_BOUND ( 'NONE', #42574, .T. ) ;
#49557 = DIRECTION ( 'NONE',  ( 0.000000000000000000, -1.000000000000000000, 0.000000000000000000 ) ) ;
#49556 = VECTOR ( 'NONE', #7949, 39.37007874015748143 ) ;
#49558 = LINE ( 'NONE', #36981, #45788 ) ;
#49559 = CIRCLE ( 'NONE', #5092, 3.033577403570481668 ) ;
#49560 = ORIENTED_EDGE ( 'NONE', *, *, #13164, .T. ) ;
#49561 = LINE ( 'NONE', #41865, #21344 ) ;
#49562 = LINE ( 'NONE', #14238, #34927 ) ;
#49563 = CARTESIAN_POINT ( 'NONE',  ( -1.636583440222564301, 3.267716535433071279, -1.417869535855831975 ) ) ;
#49564 = ORIENTED_EDGE ( 'NONE', *, *, #43846, .F. ) ;
#49565 = DIRECTION ( 'NONE',  ( 3.169619151431853688E-17, 0.9659258262890662028, -0.2588190451025280114 ) ) ;
#49566 = CARTESIAN_POINT ( 'NONE',  ( -2.576863348864732117, 1.679095609600309347, 1.442554885838411849 ) ) ;
#49567 = CARTESIAN_POINT ( 'NONE',  ( 1.882988517681383200, 1.574803149606302854, 1.069164917025817507 ) ) ;
#49568 = EDGE_LOOP ( 'NONE', ( #23295, #28183, #22794, #30912 ) ) ;
#49569 = VERTEX_POINT ( 'NONE', #36792 ) ;
#49570 =( LENGTH_UNIT ( ) NAMED_UNIT ( * ) SI_UNIT ( $, .METRE. ) );
#49571 = CARTESIAN_POINT ( 'NONE',  ( 0.4696143004045484348, 3.346456692913386100, 2.165354330708650910 ) ) ;
#49572 = CARTESIAN_POINT ( 'NONE',  ( 1.955086072690433996, 1.651253202320272839, 2.212843190815307004 ) ) ;
#49573 = DIRECTION ( 'NONE',  ( 1.734723475976806848E-16, -0.000000000000000000, 1.000000000000000000 ) ) ;
#49574 = ORIENTED_EDGE ( 'NONE', *, *, #18548, .T. ) ;
#49575 = ORIENTED_EDGE ( 'NONE', *, *, #39730, .T. ) ;
#49576 = EDGE_CURVE ( 'NONE', #19974, #35899, #14054, .T. ) ;
#49577 = DIRECTION ( 'NONE',  ( 0.000000000000000000, 0.000000000000000000, 1.000000000000000000 ) ) ;
#49578 = ORIENTED_EDGE ( 'NONE', *, *, #1412, .F. ) ;
#49579 = CARTESIAN_POINT ( 'NONE',  ( -2.142325647309101022, 3.346456692913386100, 0.3149606299212578953 ) ) ;
#49580 = DIRECTION ( 'NONE',  ( 0.000000000000000000, 0.000000000000000000, 1.000000000000000000 ) ) ;
#49581 = EDGE_CURVE ( 'NONE', #25112, #31964, #33938, .T. ) ;
#49582 = AXIS2_PLACEMENT_3D ( 'NONE', #32902, #48329, #32641 ) ;
#49583 = AXIS2_PLACEMENT_3D ( 'NONE', #37755, #49059, #25865 ) ;
#49584 = ADVANCED_FACE ( 'NONE', ( #9677 ), #45517, .F. ) ;
#49585 = EDGE_CURVE ( 'NONE', #31796, #10769, #41424, .T. ) ;
#49586 = FACE_OUTER_BOUND ( 'NONE', #16886, .T. ) ;
#49587 = FACE_OUTER_BOUND ( 'NONE', #1661, .T. ) ;
#49589 = DIRECTION ( 'NONE',  ( -3.469446951953613696E-16, 0.000000000000000000, -1.000000000000000000 ) ) ;
#49588 = VECTOR ( 'NONE', #36914, 39.37007874015748143 ) ;
#49590 = ORIENTED_EDGE ( 'NONE', *, *, #31042, .T. ) ;
#49591 = PLANE ( 'NONE',  #43996 ) ;
#49592 = CARTESIAN_POINT ( 'NONE',  ( 1.636583440222563857, 0.000000000000000000, 0.7480314960629872445 ) ) ;
#49593 = VECTOR ( 'NONE', #39389, 39.37007874015748143 ) ;
#49594 = CARTESIAN_POINT ( 'NONE',  ( -0.3486774197067339376, 3.346456692913386100, -8.878505979408855953E-16 ) ) ;
#49595 = ORIENTED_EDGE ( 'NONE', *, *, #14770, .F. ) ;
#49596 = AXIS2_PLACEMENT_3D ( 'NONE', #38, #39540, #31037 ) ;
#49597 = DIRECTION ( 'NONE',  ( -1.000000000000000000, 0.000000000000000000, -0.000000000000000000 ) ) ;
#49598 = LINE ( 'NONE', #1383, #1430 ) ;
#49599 = EDGE_CURVE ( 'NONE', #17328, #31017, #13299, .T. ) ;
#49600 = DIRECTION ( 'NONE',  ( 1.000000000000000000, 0.000000000000000000, 0.000000000000000000 ) ) ;
#49601 = EDGE_LOOP ( 'NONE', ( #41387, #36393, #37244, #35921 ) ) ;
#49602 = DIRECTION ( 'NONE',  ( -0.5877852522924802425, 0.000000000000000000, 0.8090169943749422332 ) ) ;
#49603 = EDGE_CURVE ( 'NONE', #11339, #23728, #25929, .T. ) ;
#49604 = ORIENTED_EDGE ( 'NONE', *, *, #12323, .T. ) ;
#49605 = CARTESIAN_POINT ( 'NONE',  ( -2.182111253630085290, 3.346456692913386100, 0.9448818897637749625 ) ) ;
#49606 = CARTESIAN_POINT ( 'NONE',  ( 1.363819533518803251, 0.000000000000000000, 1.220472440944875281 ) ) ;
#49607 = VERTEX_POINT ( 'NONE', #5799 ) ;
#49608 = LINE ( 'NONE', #2668, #21252 ) ;
#49609 = LINE ( 'NONE', #49858, #40832 ) ;
#49610 = LINE ( 'NONE', #7306, #43689 ) ;
#49611 = DIRECTION ( 'NONE',  ( 1.000000000000000000, -0.000000000000000000, 0.000000000000000000 ) ) ;
#49612 = ADVANCED_FACE ( 'NONE', ( #21547 ), #41677, .F. ) ;
#49613 = ORIENTED_EDGE ( 'NONE', *, *, #24096, .T. ) ;
#49614 = VERTEX_POINT ( 'NONE', #37561 ) ;
#49615 = CARTESIAN_POINT ( 'NONE',  ( 0.000000000000000000, 1.574803149606302854, 0.000000000000000000 ) ) ;
#49616 = LINE ( 'NONE', #15803, #43596 ) ;
#49617 = ORIENTED_EDGE ( 'NONE', *, *, #10693, .T. ) ;
#49618 = PLANE ( 'NONE',  #34137 ) ;
#49619 = CARTESIAN_POINT ( 'NONE',  ( -1.439733046521776139, 3.267716535433071279, 4.995077429881866871E-16 ) ) ;
#49620 = LINE ( 'NONE', #22553, #4682 ) ;
#49621 = ADVANCED_FACE ( 'NONE', ( #37051 ), #22059, .T. ) ;
#49622 = EDGE_LOOP ( 'NONE', ( #45295, #43752, #22427, #28964, #14417, #3740, #34750, #12100, #37159, #45070, #28516, #25818, #27156 ) ) ;
#49623 = VECTOR ( 'NONE', #20913, 39.37007874015748143 ) ;
#49624 = VERTEX_POINT ( 'NONE', #18183 ) ;
#49625 = PLANE ( 'NONE',  #50970 ) ;
#49626 = DIRECTION ( 'NONE',  ( 0.000000000000000000, 0.000000000000000000, -1.000000000000000000 ) ) ;
#49627 = DIRECTION ( 'NONE',  ( 1.000000000000000000, 0.000000000000000000, -3.469446951953613696E-16 ) ) ;
#49628 = VERTEX_POINT ( 'NONE', #37815 ) ;
#49629 = LINE ( 'NONE', #23825, #29816 ) ;
#49630 = AXIS2_PLACEMENT_3D ( 'NONE', #28066, #5094, #40474 ) ;
#49631 = DIRECTION ( 'NONE',  ( 1.734723475976806848E-16, 0.000000000000000000, 1.000000000000000000 ) ) ;
#49632 = VERTEX_POINT ( 'NONE', #10438 ) ;
#49633 = CARTESIAN_POINT ( 'NONE',  ( -0.2727639067037607723, 3.346456692913386100, -1.732283464566922726 ) ) ;
#49634 = VERTEX_POINT ( 'NONE', #13807 ) ;
#49635 = CIRCLE ( 'NONE', #36490, 2.165354330708661568 ) ;
#49636 = ORIENTED_EDGE ( 'NONE', *, *, #146, .F. ) ;
#49637 = DIRECTION ( 'NONE',  ( -0.000000000000000000, 0.000000000000000000, 1.000000000000000000 ) ) ;
#49638 = CARTESIAN_POINT ( 'NONE',  ( -1.946505901478385203, 5.905511811023623991, 0.9915739042680188353 ) ) ;
#49639 = VECTOR ( 'NONE', #30268, 39.37007874015748143 ) ;
#49640 = AXIS2_PLACEMENT_3D ( 'NONE', #33838, #49520, #38217 ) ;
#49641 = DIRECTION ( 'NONE',  ( 0.000000000000000000, 0.000000000000000000, -1.000000000000000000 ) ) ;
#49642 = ORIENTED_EDGE ( 'NONE', *, *, #30990, .F. ) ;
#49643 = LINE ( 'NONE', #50390, #46690 ) ;
#49644 = DIRECTION ( 'NONE',  ( -0.9998717552508122886, -0.01601477604151182316, 0.000000000000000000 ) ) ;
#49645 = VERTEX_POINT ( 'NONE', #29550 ) ;
#49646 = APPLICATION_CONTEXT ( 'automotive_design' ) ;
#49647 = ORIENTED_EDGE ( 'NONE', *, *, #5096, .F. ) ;
#49648 = DIRECTION ( 'NONE',  ( -0.7071067811865483499, -1.442222014787672788E-15, -0.7071067811865465735 ) ) ;
#49649 = CARTESIAN_POINT ( 'NONE',  ( 0.000000000000000000, 3.267716535433071279, 0.000000000000000000 ) ) ;
#49650 = EDGE_CURVE ( 'NONE', #38652, #16487, #33058, .T. ) ;
#49651 = DIRECTION ( 'NONE',  ( 0.9998717552508121775, 0.01601477604151182663, 0.000000000000000000 ) ) ;
#49652 = ADVANCED_FACE ( 'NONE', ( #40921 ), #2441, .F. ) ;
#49653 = CARTESIAN_POINT ( 'NONE',  ( -2.055928985459924085, -8.304408758680925473E-17, 0.7197570096327614575 ) ) ;
#49654 = CARTESIAN_POINT ( 'NONE',  ( -1.955094182356980070, 1.555721577805774691, 2.212836105613017246 ) ) ;
#49655 = VERTEX_POINT ( 'NONE', #45772 ) ;
#49656 = PLANE ( 'NONE',  #246 ) ;
#49657 = CARTESIAN_POINT ( 'NONE',  ( -2.454875160333845674, 0.000000000000000000, -0.1574803149606298636 ) ) ;
#49658 = VERTEX_POINT ( 'NONE', #17930 ) ;
#49659 = DIRECTION ( 'NONE',  ( 1.734723475976806848E-16, -0.000000000000000000, 1.000000000000000000 ) ) ;
#49660 = DIRECTION ( 'NONE',  ( -0.000000000000000000, 1.000000000000000000, -0.000000000000000000 ) ) ;
#49661 = ORIENTED_EDGE ( 'NONE', *, *, #29233, .T. ) ;
#49662 = PLANE ( 'NONE',  #31222 ) ;
#49663 = CARTESIAN_POINT ( 'NONE',  ( -0.6031363173298939229, 0.006153551727561678598, 1.747108239936284946 ) ) ;
#49664 = DIRECTION ( 'NONE',  ( 0.000000000000000000, 0.000000000000000000, 1.000000000000000000 ) ) ;
#49665 = VECTOR ( 'NONE', #5035, 39.37007874015748143 ) ;
#49666 = ORIENTED_EDGE ( 'NONE', *, *, #34, .T. ) ;
#49667 = CARTESIAN_POINT ( 'NONE',  ( 0.5455278134075212115, 3.267716535433071279, 0.3149606299212576177 ) ) ;
#49668 = ORIENTED_EDGE ( 'NONE', *, *, #35594, .F. ) ;
#49669 = CARTESIAN_POINT ( 'NONE',  ( -1.387661672111458078, 6.692913385826772199, -1.663104731517941692 ) ) ;
#49670 = CARTESIAN_POINT ( 'NONE',  ( -2.160407304981126320, 1.574879494900809584, -0.1462862061266896330 ) ) ;
#49671 = VECTOR ( 'NONE', #44653, 39.37007874015748143 ) ;
#49672 = AXIS2_PLACEMENT_3D ( 'NONE', #5120, #17261, #12615 ) ;
#49673 = CARTESIAN_POINT ( 'NONE',  ( 0.8182917201112824834, 3.346456692913386100, 1.417322834645662777 ) ) ;
#49674 = DIRECTION ( 'NONE',  ( 1.000000000000000000, -0.000000000000000000, 0.000000000000000000 ) ) ;
#49675 = EDGE_CURVE ( 'NONE', #6064, #12848, #25628, .T. ) ;
#49676 = VERTEX_POINT ( 'NONE', #9933 ) ;
#49677 = ORIENTED_EDGE ( 'NONE', *, *, #5295, .T. ) ;
#49678 = AXIS2_PLACEMENT_3D ( 'NONE', #26764, #42514, #3276 ) ;
#49679 = CARTESIAN_POINT ( 'NONE',  ( -2.058792518696834772, 0.5252116753648516934, 0.6171970515808470337 ) ) ;
#49680 = DIRECTION ( 'NONE',  ( -3.986037398843765983E-20, -1.000000000000000000, -1.160734090543304660E-16 ) ) ;
#49681 = DIRECTION ( 'NONE',  ( 1.000000000000000000, 0.000000000000000000, 0.000000000000000000 ) ) ;
#49682 = ORIENTED_EDGE ( 'NONE', *, *, #30457, .T. ) ;
#49683 = ADVANCED_FACE ( 'NONE', ( #49379 ), #26181, .F. ) ;
#49684 = CARTESIAN_POINT ( 'NONE',  ( -2.623503965249869729, 0.000000000000000000, 1.355882097269835107 ) ) ;
#49685 = EDGE_CURVE ( 'NONE', #42744, #46569, #9422, .T. ) ;
#49686 = ORIENTED_EDGE ( 'NONE', *, *, #45721, .T. ) ;
#49687 = CARTESIAN_POINT ( 'NONE',  ( 0.4696143004045479352, 3.267716535433071279, -0.7874015748031473194 ) ) ;
#49688 = ADVANCED_FACE ( 'NONE', ( #19179 ), #7071, .F. ) ;
#49689 = DIRECTION ( 'NONE',  ( -4.943042645790397723E-17, 1.000000000000000000, -1.156482317317871478E-16 ) ) ;
#49690 = ORIENTED_EDGE ( 'NONE', *, *, #40385, .T. ) ;
#49691 = EDGE_CURVE ( 'NONE', #17741, #48287, #27182, .T. ) ;
#49692 = CARTESIAN_POINT ( 'NONE',  ( -0.2727639067037602727, 3.346456692913386100, 1.535433070866133898 ) ) ;
#49693 = VERTEX_POINT ( 'NONE', #50623 ) ;
#49694 = ORIENTED_EDGE ( 'NONE', *, *, #1373, .F. ) ;
#49695 = EDGE_CURVE ( 'NONE', #17488, #18703, #38819, .T. ) ;
#49696 = ORIENTED_EDGE ( 'NONE', *, *, #788, .F. ) ;
#49697 = EDGE_LOOP ( 'NONE', ( #39793, #32487, #19524, #14639 ) ) ;
#49698 = CARTESIAN_POINT ( 'NONE',  ( 0.5455278134075217666, 3.267716535433071279, 1.889763779527550369 ) ) ;
#49699 = CONICAL_SURFACE ( 'NONE', #43978, 3.483074324928249421, 1.244861948955335196 ) ;
#49700 = VERTEX_POINT ( 'NONE', #22816 ) ;
#49701 = VECTOR ( 'NONE', #42594, 39.37007874015748143 ) ;
#49702 = DIRECTION ( 'NONE',  ( -3.986037398843765983E-20, -1.000000000000000000, -1.160734090543304660E-16 ) ) ;
#49703 = CARTESIAN_POINT ( 'NONE',  ( -0.8942052331142552601, 3.346456692913386100, -1.907064071829739582 ) ) ;
#49704 = VECTOR ( 'NONE', #19236, 39.37007874015748143 ) ;
#49705 = EDGE_CURVE ( 'NONE', #39500, #5813, #22314, .T. ) ;
#49706 = AXIS2_PLACEMENT_3D ( 'NONE', #16365, #20220, #11027 ) ;
#49707 = DIRECTION ( 'NONE',  ( -6.394449067488487880E-17, -1.000000000000000000, -9.687176266499690201E-17 ) ) ;
#49708 = EDGE_CURVE ( 'NONE', #12597, #4458, #10939, .T. ) ;
#49709 = DIRECTION ( 'NONE',  ( -0.000000000000000000, 1.000000000000000000, -0.000000000000000000 ) ) ;
#49710 = CARTESIAN_POINT ( 'NONE',  ( 1.091055626815042423, 3.346456692913386100, -2.086614173228339641 ) ) ;
#49711 = EDGE_CURVE ( 'NONE', #48287, #32550, #14818, .T. ) ;
#49712 = ORIENTED_EDGE ( 'NONE', *, *, #26693, .F. ) ;
#49713 = CARTESIAN_POINT ( 'NONE',  ( 1.287906020515830141, 3.346456692913386100, -0.6299212598425181220 ) ) ;
#49714 = LINE ( 'NONE', #37904, #24216 ) ;
#49715 = LINE ( 'NONE', #49968, #38368 ) ;
#49716 = CARTESIAN_POINT ( 'NONE',  ( -0.07591351300297333182, 0.000000000000000000, 2.362204724409437961 ) ) ;
#49717 = EDGE_LOOP ( 'NONE', ( #25480, #18714, #2730, #6321 ) ) ;
#49718 = CARTESIAN_POINT ( 'NONE',  ( 0.2727639067037609943, 3.346456692913386100, 2.165354330708650910 ) ) ;
#49719 = DIRECTION ( 'NONE',  ( 1.734723475976806848E-16, -0.000000000000000000, 1.000000000000000000 ) ) ;
#49720 = ORIENTED_EDGE ( 'NONE', *, *, #164, .T. ) ;
#49721 = CARTESIAN_POINT ( 'NONE',  ( 1.363819533518803695, 3.346456692913386100, 1.535433070866133898 ) ) ;
#49722 = DIRECTION ( 'NONE',  ( -1.000000000000000000, 0.000000000000000000, 0.000000000000000000 ) ) ;
#49723 = EDGE_LOOP ( 'NONE', ( #25613, #15677, #4188, #37190 ) ) ;
#49724 = B_SPLINE_CURVE_WITH_KNOTS ( 'NONE', 3,
 ( #8035, #27644, #3915, #31536 ),
 .UNSPECIFIED., .F., .F.,
 ( 4, 4 ),
 ( 0.001238008921875009350, 0.04698876036832783792 ),
 .UNSPECIFIED. ) ;
#49725 = EDGE_LOOP ( 'NONE', ( #39946, #29743, #46982, #26145, #26417, #30987, #41899, #30189, #42310, #22238, #9554 ) ) ;
#49726 = CARTESIAN_POINT ( 'NONE',  ( -2.216785221661266014, 1.578142628253058843, -1.001018901021909269 ) ) ;
#49727 = CARTESIAN_POINT ( 'NONE',  ( -0.4536155966250730032, 0.5249316497054298258, -1.828623345641975595 ) ) ;
#49728 = LINE ( 'NONE', #37918, #23744 ) ;
#49729 = FACE_OUTER_BOUND ( 'NONE', #5999, .T. ) ;
#49730 = DIRECTION ( 'NONE',  ( 0.000000000000000000, 0.000000000000000000, -1.000000000000000000 ) ) ;
#49731 = VERTEX_POINT ( 'NONE', #46774 ) ;
#49732 = DIRECTION ( 'NONE',  ( -1.000000000000000000, 0.000000000000000000, -0.000000000000000000 ) ) ;
#49733 = VECTOR ( 'NONE', #21939, 39.37007874015748143 ) ;
#49734 = VERTEX_POINT ( 'NONE', #42677 ) ;
#49735 = ORIENTED_EDGE ( 'NONE', *, *, #25935, .F. ) ;
#49736 = CARTESIAN_POINT ( 'NONE',  ( -1.647545174055839556, 0.001531214329375737114, 0.5870650656849111249 ) ) ;
#49737 = ORIENTED_EDGE ( 'NONE', *, *, #6982, .T. ) ;
#49738 = DIRECTION ( 'NONE',  ( 1.000000000000000000, -0.000000000000000000, 0.000000000000000000 ) ) ;
#49739 = CONICAL_SURFACE ( 'NONE', #34133, 3.033577403570480779, 1.554780866114618743 ) ;
#49740 = LINE ( 'NONE', #14681, #17808 ) ;
#49741 = ORIENTED_EDGE ( 'NONE', *, *, #40791, .F. ) ;
#49742 = CIRCLE ( 'NONE', #19296, 2.106299212598425008 ) ;
#49743 = LINE ( 'NONE', #38434, #28889 ) ;
#49744 = EDGE_CURVE ( 'NONE', #1426, #36108, #9318, .T. ) ;
#49745 = DIRECTION ( 'NONE',  ( 1.000000000000000000, -0.000000000000000000, 0.000000000000000000 ) ) ;
#49746 = EDGE_CURVE ( 'NONE', #47219, #50807, #39063, .T. ) ;
#49747 = EDGE_CURVE ( 'NONE', #18734, #26436, #21343, .T. ) ;
#49748 = PLANE ( 'NONE',  #34596 ) ;
#49749 = VERTEX_POINT ( 'NONE', #26930 ) ;
#49750 = ORIENTED_EDGE ( 'NONE', *, *, #17457, .T. ) ;
#49751 = CARTESIAN_POINT ( 'NONE',  ( -1.363819533518803473, 3.346456692913386100, 1.732283464566920950 ) ) ;
#49752 = FACE_BOUND ( 'NONE', #50295, .T. ) ;
#49753 = VERTEX_POINT ( 'NONE', #2685 ) ;
#49754 = LINE ( 'NONE', #30947, #26201 ) ;
#49755 = CARTESIAN_POINT ( 'NONE',  ( 0.1067246931122726866, 0.02962905676920215767, 0.000000000000000000 ) ) ;
#49756 = ORIENTED_EDGE ( 'NONE', *, *, #6673, .T. ) ;
#49757 = ORIENTED_EDGE ( 'NONE', *, *, #41376, .T. ) ;
#49758 = CARTESIAN_POINT ( 'NONE',  ( 2.623503965249849301, 1.455362298632098428, 1.355882097269874187 ) ) ;
#49759 = FACE_OUTER_BOUND ( 'NONE', #43669, .T. ) ;
#49760 = ORIENTED_EDGE ( 'NONE', *, *, #4398, .T. ) ;
#49761 = ORIENTED_EDGE ( 'NONE', *, *, #23479, .F. ) ;
#49762 = ADVANCED_FACE ( 'NONE', ( #11194 ), #38323, .F. ) ;
#49763 = ORIENTED_EDGE ( 'NONE', *, *, #788, .T. ) ;
#49764 = CARTESIAN_POINT ( 'NONE',  ( -2.101362156354032784, 1.641436391382051774, -0.5301003916084159329 ) ) ;
#49765 = LINE ( 'NONE', #14454, #18393 ) ;
#49766 = ADVANCED_FACE ( 'NONE', ( #18438 ), #2940, .F. ) ;
#49767 = DIRECTION ( 'NONE',  ( -3.469446951953613696E-16, 0.000000000000000000, -1.000000000000000000 ) ) ;
#49768 = LINE ( 'NONE', #49272, #41209 ) ;
#49769 = EDGE_CURVE ( 'NONE', #44152, #10179, #31322, .T. ) ;
#49770 = VERTEX_POINT ( 'NONE', #11693 ) ;
#49771 = ORIENTED_EDGE ( 'NONE', *, *, #34363, .F. ) ;
#49772 = LINE ( 'NONE', #9825, #15082 ) ;
#49773 = DIRECTION ( 'NONE',  ( -0.000000000000000000, 1.000000000000000000, -0.000000000000000000 ) ) ;
#49774 = VECTOR ( 'NONE', #22208, 39.37007874015748143 ) ;
#49775 = EDGE_CURVE ( 'NONE', #35273, #5175, #3191, .T. ) ;
#49776 = ADVANCED_FACE ( 'NONE', ( #30312 ), #15066, .F. ) ;
#49777 = DIRECTION ( 'NONE',  ( -1.000000000000000000, -0.000000000000000000, -0.000000000000000000 ) ) ;
#49778 = VECTOR ( 'NONE', #36070, 39.37007874015748854 ) ;
#49779 = PLANE ( 'NONE',  #5373 ) ;
#49780 = VECTOR ( 'NONE', #21401, 39.37007874015748143 ) ;
#49781 = LINE ( 'NONE', #29184, #47 ) ;
#49782 = VECTOR ( 'NONE', #10534, 39.37007874015748143 ) ;
#49783 = DIRECTION ( 'NONE',  ( -0.000000000000000000, 1.000000000000000000, -0.000000000000000000 ) ) ;
#49784 = CARTESIAN_POINT ( 'NONE',  ( -1.636583440222564301, 3.346456692913386100, -0.3149606299212592275 ) ) ;
#49785 = VECTOR ( 'NONE', #2025, 39.37007874015748143 ) ;
#49786 = VERTEX_POINT ( 'NONE', #46029 ) ;
#49787 = LINE ( 'NONE', #37974, #37428 ) ;
#49788 = LINE ( 'NONE', #30217, #38477 ) ;
#49789 = ORIENTED_EDGE ( 'NONE', *, *, #45686, .T. ) ;
#49790 = ORIENTED_EDGE ( 'NONE', *, *, #49938, .T. ) ;
#49791 = DIRECTION ( 'NONE',  ( 1.000000000000000000, 0.000000000000000000, 0.000000000000000000 ) ) ;
#49792 = VERTEX_POINT ( 'NONE', #10691 ) ;
#49793 = VERTEX_POINT ( 'NONE', #23068 ) ;
#49794 = CARTESIAN_POINT ( 'NONE',  ( 1.387241876633648285, 6.692913385826772199, 1.662624236931697919 ) ) ;
#49795 = VERTEX_POINT ( 'NONE', #3445 ) ;
#49796 = CARTESIAN_POINT ( 'NONE',  ( 2.311075683235107814, 1.679301259607557384, 0.2633944203403243423 ) ) ;
#49797 = DIRECTION ( 'NONE',  ( 1.000000000000000000, 0.000000000000000000, 0.000000000000000000 ) ) ;
#49798 = ORIENTED_EDGE ( 'NONE', *, *, #38910, .T. ) ;
#49799 = EDGE_CURVE ( 'NONE', #23841, #13784, #24453, .T. ) ;
#49800 = VERTEX_POINT ( 'NONE', #35959 ) ;
#49801 = PLANE ( 'NONE',  #37036 ) ;
#49802 = AXIS2_PLACEMENT_3D ( 'NONE', #14522, #7282, #49580 ) ;
#49803 = EDGE_CURVE ( 'NONE', #14060, #35430, #20019, .T. ) ;
#49804 = VERTEX_POINT ( 'NONE', #19930 ) ;
#49805 = ORIENTED_EDGE ( 'NONE', *, *, #46841, .F. ) ;
#49806 = VECTOR ( 'NONE', #2390, 39.37007874015748143 ) ;
#49807 = CARTESIAN_POINT ( 'NONE',  ( -1.636583440222564301, 3.267716535433071279, -0.5118110236220466680 ) ) ;
#49808 = FACE_OUTER_BOUND ( 'NONE', #4449, .T. ) ;
#49809 = DIRECTION ( 'NONE',  ( 1.734723475976806848E-16, -0.000000000000000000, 1.000000000000000000 ) ) ;
#49810 = LINE ( 'NONE', #49311, #1403 ) ;
#49811 = EDGE_CURVE ( 'NONE', #44866, #23296, #16078, .T. ) ;
#49812 = CIRCLE ( 'NONE', #1221, 2.244934639244525076 ) ;
#49813 = VECTOR ( 'NONE', #27469, 39.37007874015748143 ) ;
#49814 = ORIENTED_EDGE ( 'NONE', *, *, #11731, .T. ) ;
#49815 = CARTESIAN_POINT ( 'NONE',  ( 1.091055626815043311, 0.000000000000000000, 1.889763779527550369 ) ) ;
#49816 = CARTESIAN_POINT ( 'NONE',  ( -1.014069264286641570, 0.000000000000000000, 1.062992125984251635 ) ) ;
#49817 = DIRECTION ( 'NONE',  ( -1.000000000000000000, 0.000000000000000000, 0.000000000000000000 ) ) ;
#49818 = ORIENTED_EDGE ( 'NONE', *, *, #50553, .F. ) ;
#49819 = LINE ( 'NONE', #45457, #32318 ) ;
#49820 = CARTESIAN_POINT ( 'NONE',  ( -2.607957063720690805, 1.678602264015800261, 1.384773081428535058 ) ) ;
#49821 = CIRCLE ( 'NONE', #34221, 2.164630168518208109 ) ;
#49822 = ORIENTED_EDGE ( 'NONE', *, *, #48117, .T. ) ;
#49823 = ORIENTED_EDGE ( 'NONE', *, *, #34174, .T. ) ;
#49824 = LINE ( 'NONE', #17876, #5786 ) ;
#49825 = EDGE_CURVE ( 'NONE', #46902, #26706, #39315, .T. ) ;
#49826 = CARTESIAN_POINT ( 'NONE',  ( -2.047277537895663801, 1.675111054312220515, 0.7169459839182066307 ) ) ;
#49827 = CARTESIAN_POINT ( 'NONE',  ( 1.909347346926324684, 0.000000000000000000, 1.102362204724403938 ) ) ;
#49828 = ORIENTED_EDGE ( 'NONE', *, *, #26258, .T. ) ;
#49829 = ORIENTED_EDGE ( 'NONE', *, *, #26645, .F. ) ;
#49830 = DIRECTION ( 'NONE',  ( -1.000000000000000000, 0.000000000000000000, 1.734723475976806848E-16 ) ) ;
#49831 = EDGE_CURVE ( 'NONE', #2103, #32862, #12455, .T. ) ;
#49832 = CARTESIAN_POINT ( 'NONE',  ( 0.4696143004045479352, 3.267716535433071279, -1.417322834645664331 ) ) ;
#49833 = ORIENTED_EDGE ( 'NONE', *, *, #9787, .F. ) ;
#49834 = DIRECTION ( 'NONE',  ( -0.000000000000000000, 1.000000000000000000, -0.000000000000000000 ) ) ;
#49835 = CARTESIAN_POINT ( 'NONE',  ( -0.3486774197067340486, 3.267716535433071279, -2.077238655036873549 ) ) ;
#49836 = DIRECTION ( 'NONE',  ( 1.734723475976806848E-16, 0.000000000000000000, 1.000000000000000000 ) ) ;
#49837 = DIRECTION ( 'NONE',  ( -0.01601477604151182663, 0.9998717552508123996, -0.000000000000000000 ) ) ;
#49838 = CARTESIAN_POINT ( 'NONE',  ( -1.841876542352477886, 1.049866565877818347, -0.8407752412313899137 ) ) ;
#49839 = EDGE_LOOP ( 'NONE', ( #41156, #48427, #35738, #47239 ) ) ;
#49840 = VECTOR ( 'NONE', #4162, 39.37007874015748143 ) ;
#49841 = DIRECTION ( 'NONE',  ( -3.469446951953613696E-16, 0.000000000000000000, -1.000000000000000000 ) ) ;
#49842 = CARTESIAN_POINT ( 'NONE',  ( 1.720314620805546646, 0.000000000000000000, 0.2826945007888405637 ) ) ;
#49843 = VECTOR ( 'NONE', #40454, 39.37007874015748143 ) ;
#49844 = AXIS2_PLACEMENT_3D ( 'NONE', #23980, #997, #36116 ) ;
#49845 = DIRECTION ( 'NONE',  ( 1.734723475976806848E-16, -0.000000000000000000, 1.000000000000000000 ) ) ;
#49846 = AXIS2_PLACEMENT_3D ( 'NONE', #25398, #9914, #45249 ) ;
#49847 = ORIENTED_EDGE ( 'NONE', *, *, #30498, .T. ) ;
#49848 = FACE_OUTER_BOUND ( 'NONE', #42849, .T. ) ;
#49849 = CARTESIAN_POINT ( 'NONE',  ( -2.353647019958005071, 1.172985819482486924, -0.9842519685039374799 ) ) ;
#49850 = DIRECTION ( 'NONE',  ( 0.000000000000000000, 0.000000000000000000, -1.000000000000000000 ) ) ;
#49851 = ORIENTED_EDGE ( 'NONE', *, *, #27233, .T. ) ;
#49852 = CARTESIAN_POINT ( 'NONE',  ( 1.091055626815042645, 0.000000000000000000, -0.5118110236220471121 ) ) ;
#49853 = AXIS2_PLACEMENT_3D ( 'NONE', #27736, #19735, #19231 ) ;
#49854 = ORIENTED_EDGE ( 'NONE', *, *, #48721, .F. ) ;
#49855 = DIRECTION ( 'NONE',  ( 1.000000000000000000, 0.000000000000000000, 0.000000000000000000 ) ) ;
#49856 = ORIENTED_EDGE ( 'NONE', *, *, #23323, .F. ) ;
#49857 = CARTESIAN_POINT ( 'NONE',  ( -0.07591351300297277671, 0.000000000000000000, 1.102362204724404160 ) ) ;
#49858 = CARTESIAN_POINT ( 'NONE',  ( 0.8182917201112817063, 3.346456692913386100, -1.417322834645664331 ) ) ;
#49859 = CARTESIAN_POINT ( 'NONE',  ( -0.8182917201112819283, 3.346456692913386100, -0.6692913385826760875 ) ) ;
#49860 = CARTESIAN_POINT ( 'NONE',  ( 0.000000000000000000, 3.267716535433071279, 0.6299212598425161236 ) ) ;
#49861 = B_SPLINE_CURVE_WITH_KNOTS ( 'NONE', 3,
 ( #38824, #14824, #19692, #30826 ),
 .UNSPECIFIED., .F., .F.,
 ( 4, 4 ),
 ( 2.002016001276121705E-07, 0.002500200811381732800 ),
 .UNSPECIFIED. ) ;
#49862 = EDGE_CURVE ( 'NONE', #26872, #17017, #6381, .T. ) ;
#49863 = ORIENTED_EDGE ( 'NONE', *, *, #12508, .T. ) ;
#49864 = ORIENTED_EDGE ( 'NONE', *, *, #325, .T. ) ;
#49865 = DIRECTION ( 'NONE',  ( 1.558091277195102803E-17, -1.000000000000000000, 1.150229170499808965E-16 ) ) ;
#49866 = LINE ( 'NONE', #45763, #36218 ) ;
#49867 = EDGE_CURVE ( 'NONE', #47312, #11113, #8585, .T. ) ;
#49868 = ORIENTED_EDGE ( 'NONE', *, *, #18050, .F. ) ;
#49869 = PLANE ( 'NONE',  #9400 ) ;
#49870 = CARTESIAN_POINT ( 'NONE',  ( 1.957708528393553582, 1.673641438755806732, -1.233304704937915330 ) ) ;
#49871 = CARTESIAN_POINT ( 'NONE',  ( 2.151809081513405442, 6.692913385826772199, 0.2418202932658665705 ) ) ;
#49872 = EDGE_CURVE ( 'NONE', #48423, #24715, #327, .T. ) ;
#49873 = ORIENTED_EDGE ( 'NONE', *, *, #15233, .F. ) ;
#49874 = ORIENTED_EDGE ( 'NONE', *, *, #11572, .F. ) ;
#49875 = CARTESIAN_POINT ( 'NONE',  ( 0.5905511811023627100, 0.000000000000000000, 0.000000000000000000 ) ) ;
#49876 = CARTESIAN_POINT ( 'NONE',  ( -0.5433905323321888137, 1.526322510227913654, 2.902372092969472739 ) ) ;
#49877 = CARTESIAN_POINT ( 'NONE',  ( 1.363819533518803251, 3.346456692913386100, 0.4724409448818871482 ) ) ;
#49878 = EDGE_CURVE ( 'NONE', #24641, #10066, #24594, .T. ) ;
#49879 = ORIENTED_EDGE ( 'NONE', *, *, #6521, .T. ) ;
#49880 = SURFACE_SIDE_STYLE ('',( #34195 ) ) ;
#49881 = LINE ( 'NONE', #41429, #41692 ) ;
#49882 = AXIS2_PLACEMENT_3D ( 'NONE', #1753, #44352, #4872 ) ;
#49883 = ORIENTED_EDGE ( 'NONE', *, *, #29311, .F. ) ;
#49884 = CIRCLE ( 'NONE', #4597, 0.3937007874015748254 ) ;
#49885 = DIRECTION ( 'NONE',  ( -1.000000000000000000, 0.000000000000000000, 0.000000000000000000 ) ) ;
#49886 = ORIENTED_EDGE ( 'NONE', *, *, #16485, .F. ) ;
#49887 = VERTEX_POINT ( 'NONE', #40348 ) ;
#49888 = FACE_OUTER_BOUND ( 'NONE', #38075, .T. ) ;
#49889 = DIRECTION ( 'NONE',  ( 0.000000000000000000, -1.000000000000000000, 0.000000000000000000 ) ) ;
#49890 = VECTOR ( 'NONE', #33924, 39.37007874015748854 ) ;
#49891 = LINE ( 'NONE', #14582, #8247 ) ;
#49892 = ADVANCED_FACE ( 'NONE', ( #8331 ), #32095, .F. ) ;
#49893 = AXIS2_PLACEMENT_3D ( 'NONE', #33699, #42432, #46034 ) ;
#49894 = DIRECTION ( 'NONE',  ( 1.734723475976806848E-16, 0.000000000000000000, 1.000000000000000000 ) ) ;
#49895 = PLANE ( 'NONE',  #24659 ) ;
#49896 = ORIENTED_EDGE ( 'NONE', *, *, #29869, .F. ) ;
#49897 = VECTOR ( 'NONE', #42161, 39.37007874015748143 ) ;
#49898 = EDGE_CURVE ( 'NONE', #9086, #14000, #43937, .T. ) ;
#49899 = VERTEX_POINT ( 'NONE', #16596 ) ;
#49900 = CARTESIAN_POINT ( 'NONE',  ( -0.1876863054094430605, 0.000000000000000000, -1.901365838955026533 ) ) ;
#49901 = CARTESIAN_POINT ( 'NONE',  ( 0.000000000000000000, 0.000000000000000000, -1.181102362204723200 ) ) ;
#49902 = DIRECTION ( 'NONE',  ( -0.000000000000000000, 1.000000000000000000, -0.000000000000000000 ) ) ;
#49903 = LINE ( 'NONE', #27206, #21221 ) ;
#49904 = CARTESIAN_POINT ( 'NONE',  ( -1.979793062125317471, 1.556934451446513545, 2.191257344206539504 ) ) ;
#49905 = EDGE_LOOP ( 'NONE', ( #8092, #29982, #7746, #22414 ) ) ;
#49906 = FACE_OUTER_BOUND ( 'NONE', #13010, .T. ) ;
#49907 = EDGE_CURVE ( 'NONE', #15732, #14052, #43431, .T. ) ;
#49908 = FACE_OUTER_BOUND ( 'NONE', #9801, .T. ) ;
#49909 = VERTEX_POINT ( 'NONE', #44199 ) ;
#49910 = CARTESIAN_POINT ( 'NONE',  ( 1.909347346926324684, 0.000000000000000000, -0.03937007874015936021 ) ) ;
#49911 = CARTESIAN_POINT ( 'NONE',  ( 1.478089240774732582, 0.05159396975604255142, 1.241682111880268558 ) ) ;
#49912 = EDGE_LOOP ( 'NONE', ( #36463, #29540, #44696, #36632 ) ) ;
#49913 = CARTESIAN_POINT ( 'NONE',  ( 2.182111253630085290, 0.000000000000000000, 0.3149606299212573401 ) ) ;
#49914 = AXIS2_PLACEMENT_3D ( 'NONE', #27712, #612, #12480 ) ;
#49915 = LINE ( 'NONE', #9967, #1222 ) ;
#49916 = DIRECTION ( 'NONE',  ( 1.000000000000000000, -0.000000000000000000, 0.000000000000000000 ) ) ;
#49917 = PRESENTATION_LAYER_ASSIGNMENT (  '', '', ( #14516 ) ) ;
#49918 = AXIS2_PLACEMENT_3D ( 'NONE', #12094, #40486, #48436 ) ;
#49919 = VERTEX_POINT ( 'NONE', #587 ) ;
#49920 = CARTESIAN_POINT ( 'NONE',  ( 1.083598637574782364, 1.205361022782829114E-17, 2.747180975113346246 ) ) ;
#49921 = ORIENTED_EDGE ( 'NONE', *, *, #38239, .F. ) ;
#49922 = FACE_BOUND ( 'NONE', #29324, .T. ) ;
#49923 = AXIS2_PLACEMENT_3D ( 'NONE', #47073, #14873, #43230 ) ;
#49924 = LINE ( 'NONE', #37608, #9442 ) ;
#49925 = CARTESIAN_POINT ( 'NONE',  ( -0.2727639067037602172, 3.267716535433071279, 0.7874015748031456541 ) ) ;
#49926 = CARTESIAN_POINT ( 'NONE',  ( 0.4696143004045484903, 3.267716535433071279, 2.362204724409437961 ) ) ;
#49927 = CIRCLE ( 'NONE', #12051, 2.106299212598425008 ) ;
#49928 = VECTOR ( 'NONE', #20583, 39.37007874015748143 ) ;
#49929 = ORIENTED_EDGE ( 'NONE', *, *, #50747, .F. ) ;
#49930 = ORIENTED_EDGE ( 'NONE', *, *, #16695, .T. ) ;
#49931 = CARTESIAN_POINT ( 'NONE',  ( 0.5455278134075211005, 3.346456692913386100, 0.7480314960629872445 ) ) ;
#49932 = CARTESIAN_POINT ( 'NONE',  ( -2.102985103392958077, 3.346456692913386100, 0.1181102362204704270 ) ) ;
#49933 = CARTESIAN_POINT ( 'NONE',  ( -0.5455278134075214336, 3.346456692913386100, 2.204724409448808764 ) ) ;
#49934 = CARTESIAN_POINT ( 'NONE',  ( 1.636583440222563857, 0.000000000000000000, 0.6299212598425164567 ) ) ;
#49935 = EDGE_CURVE ( 'NONE', #46463, #25200, #67, .T. ) ;
#49936 = DIRECTION ( 'NONE',  ( -0.9998717552508122886, -0.01601477604151180928, 0.000000000000000000 ) ) ;
#49937 = ORIENTED_EDGE ( 'NONE', *, *, #35945, .T. ) ;
#49938 = EDGE_CURVE ( 'NONE', #31986, #19249, #23150, .T. ) ;
#49939 = ORIENTED_EDGE ( 'NONE', *, *, #43404, .T. ) ;
#49940 = DIRECTION ( 'NONE',  ( -0.01601477604151182663, 0.9998717552508123996, -0.000000000000000000 ) ) ;
#49941 = EDGE_CURVE ( 'NONE', #3939, #24556, #20711, .T. ) ;
#49942 = DIRECTION ( 'NONE',  ( 0.08963930890342654279, -1.156097046908844086E-16, 0.9959742939952397345 ) ) ;
#49943 = ORIENTED_EDGE ( 'NONE', *, *, #15259, .F. ) ;
#49944 = DIRECTION ( 'NONE',  ( -0.000000000000000000, 1.000000000000000000, -0.000000000000000000 ) ) ;
#49945 = VERTEX_POINT ( 'NONE', #43173 ) ;
#49946 = ORIENTED_EDGE ( 'NONE', *, *, #9436, .F. ) ;
#49947 = EDGE_CURVE ( 'NONE', #6064, #26089, #18863, .T. ) ;
#49948 = CIRCLE ( 'NONE', #45844, 1.850107469027523432 ) ;
#49949 = EDGE_LOOP ( 'NONE', ( #19310, #25510, #20779, #38061, #45128, #39327, #2194, #20135, #2667, #20056, #48349, #6130, #11999 ) ) ;
#49950 = ORIENTED_EDGE ( 'NONE', *, *, #43624, .T. ) ;
#49951 = LINE ( 'NONE', #46101, #44205 ) ;
#49952 = AXIS2_PLACEMENT_3D ( 'NONE', #2255, #13624, #5870 ) ;
#49953 = AXIS2_PLACEMENT_3D ( 'NONE', #48381, #1436, #33717 ) ;
#49954 = ORIENTED_EDGE ( 'NONE', *, *, #49746, .T. ) ;
#49955 = PLANE ( 'NONE',  #23760 ) ;
#49956 = AXIS2_PLACEMENT_3D ( 'NONE', #27937, #12973, #7816 ) ;
#49957 = CARTESIAN_POINT ( 'NONE',  ( -1.195183497228115035E-16, 3.346456692913386100, -1.574803149606293529 ) ) ;
#49958 = AXIS2_PLACEMENT_3D ( 'NONE', #12289, #43508, #32174 ) ;
#49959 = EDGE_CURVE ( 'NONE', #27610, #383, #8075, .T. ) ;
#49960 = CARTESIAN_POINT ( 'NONE',  ( 2.319222573356612749, 1.745048544795088308, -0.1534186080535354380 ) ) ;
#49961 = B_SPLINE_CURVE_WITH_KNOTS ( 'NONE', 3,
 ( #35382, #1176, #36145, #47203 ),
 .UNSPECIFIED., .F., .F.,
 ( 4, 4 ),
 ( 3.580237009053578663E-05, 0.004936055722876062785 ),
 .UNSPECIFIED. ) ;
#49962 = AXIS2_PLACEMENT_3D ( 'NONE', #4198, #39311, #11441 ) ;
#49963 = CARTESIAN_POINT ( 'NONE',  ( 1.025452293874513421, 0.4610579152940179615, -1.025452293874514087 ) ) ;
#49964 = LINE ( 'NONE', #41759, #7307 ) ;
#49965 = ORIENTED_EDGE ( 'NONE', *, *, #12871, .F. ) ;
#49966 = LINE ( 'NONE', #18774, #29937 ) ;
#49967 = CYLINDRICAL_SURFACE ( 'NONE', #38234, 2.165354330708661568 ) ;
#49968 = CARTESIAN_POINT ( 'NONE',  ( 9.902948977033107009E-17, 3.267716535433071279, -1.717887807185983406E-32 ) ) ;
#49969 = EDGE_CURVE ( 'NONE', #41613, #38443, #20854, .T. ) ;
#49970 = CARTESIAN_POINT ( 'NONE',  ( -1.046684505418381761, 0.4561333243160194950, 1.030376884852511665 ) ) ;
#49971 = ORIENTED_EDGE ( 'NONE', *, *, #34770, .T. ) ;
#49972 = LINE ( 'NONE', #15417, #5058 ) ;
#49973 = CARTESIAN_POINT ( 'NONE',  ( -1.740978969773838037, 0.000000000000000000, 0.09160132170885167124 ) ) ;
#49974 = VERTEX_POINT ( 'NONE', #13740 ) ;
#49975 = LINE ( 'NONE', #10779, #4028 ) ;
#49976 = CARTESIAN_POINT ( 'NONE',  ( -0.8942052331142552601, 3.267716535433071279, -1.972094414217999914 ) ) ;
#49977 = ORIENTED_EDGE ( 'NONE', *, *, #2960, .F. ) ;
#49978 = ADVANCED_FACE ( 'NONE', ( #33626 ), #41361, .T. ) ;
#49979 = CARTESIAN_POINT ( 'NONE',  ( 0.5550072188453405442, 1.618366210323673338, -2.196007637835879045 ) ) ;
#49980 = EDGE_LOOP ( 'NONE', ( #9206, #36236, #3434, #35129 ) ) ;
#49981 = DIRECTION ( 'NONE',  ( -0.000000000000000000, 1.000000000000000000, -0.000000000000000000 ) ) ;
#49982 = EDGE_CURVE ( 'NONE', #19986, #49275, #40649, .T. ) ;
#49983 = PLANE ( 'NONE',  #33334 ) ;
#49984 = LINE ( 'NONE', #30160, #6444 ) ;
#49985 = CARTESIAN_POINT ( 'NONE',  ( -1.985260859929297572, 3.267716535433071279, 0.9448818897637749625 ) ) ;
#49986 = FACE_OUTER_BOUND ( 'NONE', #9982, .T. ) ;
#49987 = ORIENTED_EDGE ( 'NONE', *, *, #2313, .T. ) ;
#49988 = VECTOR ( 'NONE', #36060, 39.37007874015748143 ) ;
#49989 = LINE ( 'NONE', #2289, #42985 ) ;
#49990 = VECTOR ( 'NONE', #17003, 39.37007874015748143 ) ;
#49991 = ORIENTED_EDGE ( 'NONE', *, *, #27297, .T. ) ;
#49992 = ORIENTED_EDGE ( 'NONE', *, *, #4765, .T. ) ;
#49993 = PLANE ( 'NONE',  #9755 ) ;
#49994 = VERTEX_POINT ( 'NONE', #17607 ) ;
#49995 = CARTESIAN_POINT ( 'NONE',  ( 0.7423782071083085965, 0.000000000000000000, -0.8267716535433055070 ) ) ;
#49997 = B_SPLINE_CURVE_WITH_KNOTS ( 'NONE', 3,
 ( #29127, #21396, #48710, #13392 ),
 .UNSPECIFIED., .F., .F.,
 ( 4, 4 ),
 ( 0.05160696124554316894, 0.05353638449097523899 ),
 .UNSPECIFIED. ) ;
#49996 = CARTESIAN_POINT ( 'NONE',  ( -0.8182917201112819283, 0.000000000000000000, -1.102362204724405492 ) ) ;
#49998 = ORIENTED_EDGE ( 'NONE', *, *, #3074, .F. ) ;
#49999 = EDGE_CURVE ( 'NONE', #12958, #16898, #25828, .T. ) ;
#50000 = LINE ( 'NONE', #26547, #22308 ) ;
#50001 = CARTESIAN_POINT ( 'NONE',  ( -0.2431224069213027139, 5.905511811023623991, 2.152304290637670814 ) ) ;
#50002 = EDGE_CURVE ( 'NONE', #23085, #11914, #44723, .T. ) ;
#50003 = EDGE_CURVE ( 'NONE', #36675, #12460, #32870, .T. ) ;
#50004 = LINE ( 'NONE', #22434, #45291 ) ;
#50005 = ADVANCED_FACE ( 'NONE', ( #10117 ), #49699, .T. ) ;
#50006 = ORIENTED_EDGE ( 'NONE', *, *, #42804, .F. ) ;
#50007 = EDGE_LOOP ( 'NONE', ( #28833, #30889, #35251, #42430 ) ) ;
#50008 = CARTESIAN_POINT ( 'NONE',  ( 0.2727639067037602172, 0.000000000000000000, -2.047244094488182231 ) ) ;
#50009 = FACE_BOUND ( 'NONE', #4948, .T. ) ;
#50010 = ORIENTED_EDGE ( 'NONE', *, *, #25687, .F. ) ;
#50011 = LINE ( 'NONE', #3829, #28658 ) ;
#50012 = B_SPLINE_CURVE_WITH_KNOTS ( 'NONE', 3,
 ( #39450, #27565, #8719, #31708 ),
 .UNSPECIFIED., .F., .F.,
 ( 4, 4 ),
 ( 4.932109407666375322E-07, 0.04440089579718710378 ),
 .UNSPECIFIED. ) ;
#50013 = FACE_OUTER_BOUND ( 'NONE', #39546, .T. ) ;
#50014 = VERTEX_POINT ( 'NONE', #33880 ) ;
#50015 = ORIENTED_EDGE ( 'NONE', *, *, #35304, .T. ) ;
#50016 = CARTESIAN_POINT ( 'NONE',  ( -1.091055626815042645, 0.000000000000000000, -0.3149606299212593941 ) ) ;
#50017 = PLANE ( 'NONE',  #19585 ) ;
#50018 = ORIENTED_EDGE ( 'NONE', *, *, #23407, .F. ) ;
#50019 = ORIENTED_EDGE ( 'NONE', *, *, #12029, .T. ) ;
#50020 = DIRECTION ( 'NONE',  ( -1.000000000000000000, 0.000000000000000000, -0.000000000000000000 ) ) ;
#50021 = CARTESIAN_POINT ( 'NONE',  ( -1.806430656824982384, 0.5249316497054298258, 0.5351997120806747388 ) ) ;
#50022 = VECTOR ( 'NONE', #39317, 39.37007874015748143 ) ;
#50023 = ADVANCED_FACE ( 'NONE', ( #29224 ), #40687, .T. ) ;
#50024 = CARTESIAN_POINT ( 'NONE',  ( 0.1968503937007874405, 3.267716535433071279, -6.829619984160658046E-17 ) ) ;
#50025 = EDGE_LOOP ( 'NONE', ( #32452, #30571, #13665, #7621 ) ) ;
#50026 = VERTEX_POINT ( 'NONE', #5218 ) ;
#50028 = VECTOR ( 'NONE', #33721, 39.37007874015748143 ) ;
#50027 = DIRECTION ( 'NONE',  ( -0.000000000000000000, 1.000000000000000000, -0.000000000000000000 ) ) ;
#50029 = LINE ( 'NONE', #9826, #30411 ) ;
#50030 = CARTESIAN_POINT ( 'NONE',  ( -1.985260859929297572, 3.267716535433071279, 6.887757239314511260E-16 ) ) ;
#50031 = LINE ( 'NONE', #14716, #43275 ) ;
#50032 = EDGE_CURVE ( 'NONE', #39171, #29717, #44957, .T. ) ;
#50033 = LINE ( 'NONE', #14718, #24828 ) ;
#50034 = EDGE_CURVE ( 'NONE', #22389, #29512, #9095, .T. ) ;
#50035 = CARTESIAN_POINT ( 'NONE',  ( 0.8668862056626265300, 0.04180443457634609727, -1.686684286392636789 ) ) ;
#50036 = ADVANCED_FACE ( 'NONE', ( #28962 ), #10163, .T. ) ;
#50037 = CARTESIAN_POINT ( 'NONE',  ( 0.5455278134075212115, 0.000000000000000000, -1.259842519685035134 ) ) ;
#50038 = B_SPLINE_CURVE_WITH_KNOTS ( 'NONE', 3,
 ( #1559, #39771, #32296, #17312 ),
 .UNSPECIFIED., .F., .F.,
 ( 4, 4 ),
 ( 2.075011166194589347E-07, 0.002500489532013033724 ),
 .UNSPECIFIED. ) ;
#50039 = ORIENTED_EDGE ( 'NONE', *, *, #11293, .T. ) ;
#50040 = PLANE ( 'NONE',  #8551 ) ;
#50041 = CARTESIAN_POINT ( 'NONE',  ( 2.209387264600206180, 0.9904353868938117200, -1.399436384156840463 ) ) ;
#50042 = AXIS2_PLACEMENT_3D ( 'NONE', #43705, #44481, #35987 ) ;
#50043 = VERTEX_POINT ( 'NONE', #37242 ) ;
#50044 = ORIENTED_EDGE ( 'NONE', *, *, #47536, .T. ) ;
#50045 = CARTESIAN_POINT ( 'NONE',  ( 0.8182917201112824834, 3.346456692913386100, 1.535433070866133898 ) ) ;
#50046 = DIRECTION ( 'NONE',  ( -0.4738686624730094610, -1.160734090543304907E-16, 0.8805955318567322276 ) ) ;
#50047 = EDGE_LOOP ( 'NONE', ( #45382, #17422, #50433, #29439 ) ) ;
#50048 = ORIENTED_EDGE ( 'NONE', *, *, #37509, .F. ) ;
#50049 = CARTESIAN_POINT ( 'NONE',  ( -0.8069532150559466377, 6.692913385826772199, -2.010061882867142824 ) ) ;
#50050 = ORIENTED_EDGE ( 'NONE', *, *, #3167, .T. ) ;
#50051 = EDGE_CURVE ( 'NONE', #21463, #20848, #37498, .T. ) ;
#50052 = LINE ( 'NONE', #2358, #6229 ) ;
#50053 = CARTESIAN_POINT ( 'NONE',  ( 2.164823134740037069, 1.574803149606302854, -0.04796011690015113127 ) ) ;
#50054 = CIRCLE ( 'NONE', #1461, 1.850107469027523432 ) ;
#50055 = CIRCLE ( 'NONE', #29470, 2.106299212598425008 ) ;
#50056 = EDGE_CURVE ( 'NONE', #370, #11074, #40597, .T. ) ;
#50057 = EDGE_CURVE ( 'NONE', #5904, #17741, #1859, .T. ) ;
#50058 = ORIENTED_EDGE ( 'NONE', *, *, #44222, .F. ) ;
#50059 = B_SPLINE_CURVE_WITH_KNOTS ( 'NONE', 3,
 ( #50995, #23947, #27554, #26798 ),
 .UNSPECIFIED., .F., .F.,
 ( 4, 4 ),
 ( 0.04063207013448753152, 0.04124740858473308069 ),
 .UNSPECIFIED. ) ;
#50060 = CARTESIAN_POINT ( 'NONE',  ( 0.8182917201112819283, 0.000000000000000000, 0.1574803149606286423 ) ) ;
#50061 = EDGE_CURVE ( 'NONE', #14069, #49887, #9611, .T. ) ;
#50063 = ORIENTED_EDGE ( 'NONE', *, *, #30976, .F. ) ;
#50062 = EDGE_CURVE ( 'NONE', #17057, #10877, #40852, .T. ) ;
#50064 = VERTEX_POINT ( 'NONE', #36985 ) ;
#50065 = LINE ( 'NONE', #42104, #43756 ) ;
#50066 = DIRECTION ( 'NONE',  ( -1.000000000000000000, 0.000000000000000000, 1.734723475976806848E-16 ) ) ;
#50067 = DIRECTION ( 'NONE',  ( 1.734723475976806848E-16, -0.000000000000000000, 1.000000000000000000 ) ) ;
#50068 = CARTESIAN_POINT ( 'NONE',  ( 0.000000000000000000, 7.874015748031496287, 0.000000000000000000 ) ) ;
#50069 = VECTOR ( 'NONE', #33312, 39.37007874015748143 ) ;
#50070 = VERTEX_POINT ( 'NONE', #41113 ) ;
#50071 = DIRECTION ( 'NONE',  ( 1.000000000000000000, 0.000000000000000000, 0.000000000000000000 ) ) ;
#50072 = PLANE ( 'NONE',  #17611 ) ;
#50073 = CARTESIAN_POINT ( 'NONE',  ( -1.743434144314990553, 0.0004760342511857242553, -0.01934991164580179140 ) ) ;
#50074 = EDGE_LOOP ( 'NONE', ( #6000, #6560, #28441, #46815 ) ) ;
#50075 = AXIS2_PLACEMENT_3D ( 'NONE', #45149, #37441, #17809 ) ;
#50076 = CARTESIAN_POINT ( 'NONE',  ( 2.182111253630085290, 3.346456692913386100, 0.4330708661417287386 ) ) ;
#50077 = ORIENTED_EDGE ( 'NONE', *, *, #179, .F. ) ;
#50078 = ORIENTED_EDGE ( 'NONE', *, *, #7025, .T. ) ;
#50079 = DIRECTION ( 'NONE',  ( 1.000000000000000000, 0.000000000000000000, 0.000000000000000000 ) ) ;
#50080 = AXIS2_PLACEMENT_3D ( 'NONE', #9006, #28870, #40756 ) ;
#50081 = CARTESIAN_POINT ( 'NONE',  ( -1.712496953225537411, 3.267716535433071279, 5.941417334598190051E-16 ) ) ;
#50082 = LINE ( 'NONE', #42372, #7193 ) ;
#50083 = CARTESIAN_POINT ( 'NONE',  ( -0.3486774197067340486, 0.000000000000000000, -0.8267716535433049518 ) ) ;
#50084 = EDGE_LOOP ( 'NONE', ( #1202, #6883, #28319, #27739 ) ) ;
#50085 = EDGE_LOOP ( 'NONE', ( #12408, #29677, #14278, #42038 ) ) ;
#50086 = DIRECTION ( 'NONE',  ( -0.01601477604151182663, 0.9998717552508123996, -0.000000000000000000 ) ) ;
#50087 = CARTESIAN_POINT ( 'NONE',  ( 2.322368699764507216, 1.646673738916892837, -0.1535599007534338978 ) ) ;
#50088 = ORIENTED_EDGE ( 'NONE', *, *, #26281, .T. ) ;
#50089 = CARTESIAN_POINT ( 'NONE',  ( -1.399962034674500755, 1.689509322587608109, -2.010607907135041117 ) ) ;
#50090 = FACE_OUTER_BOUND ( 'NONE', #27467, .T. ) ;
#50091 = ADVANCED_FACE ( 'NONE', ( #5984 ), #6246, .T. ) ;
#50092 = VECTOR ( 'NONE', #7933, 39.37007874015748854 ) ;
#50093 = CARTESIAN_POINT ( 'NONE',  ( -2.137893032918561254, 1.681902701049137638, 1.641967526060646554 ) ) ;
#50094 = ADVANCED_FACE ( 'NONE', ( #38753 ), #7261, .F. ) ;
#50095 = FACE_OUTER_BOUND ( 'NONE', #23785, .T. ) ;
#50096 = DIRECTION ( 'NONE',  ( 1.000000000000000000, 0.000000000000000000, 0.000000000000000000 ) ) ;
#50097 = ORIENTED_EDGE ( 'NONE', *, *, #16294, .T. ) ;
#50098 = LINE ( 'NONE', #3154, #29970 ) ;
#50099 = DIRECTION ( 'NONE',  ( -0.01601477604151182663, 0.9998717552508123996, -0.000000000000000000 ) ) ;
#50100 = VERTEX_POINT ( 'NONE', #23004 ) ;
#50102 = CARTESIAN_POINT ( 'NONE',  ( -0.1729294490429659770, 1.708950541169384163, -2.470410437739172682 ) ) ;
#50101 = VECTOR ( 'NONE', #27920, 39.37007874015748143 ) ;
#50103 = FACE_OUTER_BOUND ( 'NONE', #10465, .T. ) ;
#50104 = CARTESIAN_POINT ( 'NONE',  ( 1.785493683324574254, 0.000000000000000000, -1.119626681005672530 ) ) ;
#50105 = ORIENTED_EDGE ( 'NONE', *, *, #31221, .F. ) ;
#50106 = AXIS2_PLACEMENT_3D ( 'NONE', #8984, #16481, #24985 ) ;
#50107 = DIRECTION ( 'NONE',  ( -1.000000000000000000, 0.000000000000000000, 1.734723475976806848E-16 ) ) ;
#50108 = ORIENTED_EDGE ( 'NONE', *, *, #12850, .F. ) ;
#50109 = LINE ( 'NONE', #26655, #37784 ) ;
#50111 = ORIENTED_EDGE ( 'NONE', *, *, #43442, .T. ) ;
#50110 = EDGE_CURVE ( 'NONE', #32403, #49887, #10629, .T. ) ;
#50112 = AXIS2_PLACEMENT_3D ( 'NONE', #15420, #26772, #31415 ) ;
#50113 = LINE ( 'NONE', #31046, #13001 ) ;
#50114 = FACE_OUTER_BOUND ( 'NONE', #24059, .T. ) ;
#50115 = EDGE_CURVE ( 'NONE', #41705, #1977, #41002, .T. ) ;
#50116 = DIRECTION ( 'NONE',  ( -0.000000000000000000, 1.000000000000000000, -0.000000000000000000 ) ) ;
#50117 = FACE_OUTER_BOUND ( 'NONE', #45816, .T. ) ;
#50118 = EDGE_CURVE ( 'NONE', #45493, #7930, #2878, .T. ) ;
#50119 = ORIENTED_EDGE ( 'NONE', *, *, #37001, .T. ) ;
#50120 = VERTEX_POINT ( 'NONE', #18371 ) ;
#50121 = ORIENTED_EDGE ( 'NONE', *, *, #37012, .T. ) ;
#50122 = LINE ( 'NONE', #31056, #46328 ) ;
#50123 = CARTESIAN_POINT ( 'NONE',  ( 2.182111253630085290, 3.346456692913386100, 0.6299212598425161236 ) ) ;
#50124 = ADVANCED_FACE ( 'NONE', ( #14500 ), #28321, .T. ) ;
#50125 = ORIENTED_EDGE ( 'NONE', *, *, #33792, .F. ) ;
#50126 = CARTESIAN_POINT ( 'NONE',  ( -2.748374859398606596, 5.118110236220475784, -0.3226306186023585321 ) ) ;
#50127 = DIRECTION ( 'NONE',  ( -1.000000000000000000, -0.000000000000000000, -0.000000000000000000 ) ) ;
#50128 = DIRECTION ( 'NONE',  ( 0.7071067811865469066, 0.7071067811865481278, -4.088782444488994004E-17 ) ) ;
#50129 = VERTEX_POINT ( 'NONE', #26367 ) ;
#50130 = VERTEX_POINT ( 'NONE', #38255 ) ;
#50131 = LINE ( 'NONE', #14817, #16400 ) ;
#50132 = CARTESIAN_POINT ( 'NONE',  ( 0.5455278134075216556, 3.346456692913386100, 1.692913385826762873 ) ) ;
#50133 = DIRECTION ( 'NONE',  ( 1.734723475976806848E-16, -0.000000000000000000, 1.000000000000000000 ) ) ;
#50134 = EDGE_LOOP ( 'NONE', ( #43580, #45519, #4433, #33023 ) ) ;
#50135 = FACE_BOUND ( 'NONE', #35013, .T. ) ;
#50136 = VERTEX_POINT ( 'NONE', #7004 ) ;
#50137 = LINE ( 'NONE', #9683, #45486 ) ;
#50138 = ORIENTED_EDGE ( 'NONE', *, *, #24809, .F. ) ;
#50140 = VERTEX_POINT ( 'NONE', #26861 ) ;
#50139 = AXIS2_PLACEMENT_3D ( 'NONE', #42840, #7487, #19849 ) ;
#50141 = CARTESIAN_POINT ( 'NONE',  ( 0.8182917201112821504, 3.267716535433071279, -1.419509857074483539E-16 ) ) ;
#50142 = CARTESIAN_POINT ( 'NONE',  ( 0.2156685157584266599, 5.905511811023624880, -2.945280361644574629 ) ) ;
#50143 = VECTOR ( 'NONE', #27431, 39.37007874015748143 ) ;
#50144 = VECTOR ( 'NONE', #25153, 39.37007874015748143 ) ;
#50145 = DIRECTION ( 'NONE',  ( -3.469446951953613696E-16, 0.000000000000000000, -1.000000000000000000 ) ) ;
#50146 = LINE ( 'NONE', #11462, #7153 ) ;
#50148 = CARTESIAN_POINT ( 'NONE',  ( -1.472219874544909546, 1.205361022782829114E-17, 2.560030851058948898 ) ) ;
#50147 = VECTOR ( 'NONE', #7774, 39.37007874015748143 ) ;
#50149 = ORIENTED_EDGE ( 'NONE', *, *, #10716, .T. ) ;
#50150 = AXIS2_PLACEMENT_3D ( 'NONE', #40888, #6284, #25896 ) ;
#50151 = ORIENTED_EDGE ( 'NONE', *, *, #398, .T. ) ;
#50152 = CARTESIAN_POINT ( 'NONE',  ( 0.8182917201112824834, 3.267716535433071279, 2.047244094488179567 ) ) ;
#50153 = CARTESIAN_POINT ( 'NONE',  ( -1.091055626815042645, 0.000000000000000000, -0.9448818897637760728 ) ) ;
#50154 = B_SPLINE_CURVE_WITH_KNOTS ( 'NONE', 3,
 ( #44026, #44289, #31401, #8673 ),
 .UNSPECIFIED., .F., .F.,
 ( 4, 4 ),
 ( 2.558111634305129087E-07, 0.01955996689373667996 ),
 .UNSPECIFIED. ) ;
#50155 = PLANE ( 'NONE',  #11593 ) ;
#50156 = EDGE_CURVE ( 'NONE', #19452, #19800, #22751, .T. ) ;
#50157 = DIRECTION ( 'NONE',  ( 0.01601477604151182663, -0.9998717552508123996, 0.000000000000000000 ) ) ;
#50158 = DIRECTION ( 'NONE',  ( 1.000000000000000000, 0.000000000000000000, 0.000000000000000000 ) ) ;
#50159 = ORIENTED_EDGE ( 'NONE', *, *, #44996, .F. ) ;
#50160 = EDGE_CURVE ( 'NONE', #21917, #17338, #15255, .T. ) ;
#50161 = CARTESIAN_POINT ( 'NONE',  ( -0.07591351300297333182, 0.000000000000000000, -1.417322834645664331 ) ) ;
#50162 = CARTESIAN_POINT ( 'NONE',  ( -0.07591351300297333182, 3.267716535433071279, -0.4724409448818883694 ) ) ;
#50163 = EDGE_CURVE ( 'NONE', #14001, #29095, #34625, .T. ) ;
#50164 = ORIENTED_EDGE ( 'NONE', *, *, #28622, .F. ) ;
#50165 = CARTESIAN_POINT ( 'NONE',  ( -0.3136974817027967100, 1.714375164834789356, -2.936457595020224520 ) ) ;
#50166 = LINE ( 'NONE', #34726, #11304 ) ;
#50167 = CARTESIAN_POINT ( 'NONE',  ( -1.152114531865843006, 1.205361022782829114E-17, 1.393499336327983729 ) ) ;
#50168 = CARTESIAN_POINT ( 'NONE',  ( 0.4696143004045482128, 3.267716535433071279, -1.629301903132388492E-16 ) ) ;
#50169 = DIRECTION ( 'NONE',  ( -3.469446951953613696E-16, 0.000000000000000000, -1.000000000000000000 ) ) ;
#50170 = ORIENTED_EDGE ( 'NONE', *, *, #5982, .T. ) ;
#50171 = FACE_OUTER_BOUND ( 'NONE', #33618, .T. ) ;
#50172 = VERTEX_POINT ( 'NONE', #3632 ) ;
#50173 = FACE_BOUND ( 'NONE', #9151, .T. ) ;
#50174 = VECTOR ( 'NONE', #26695, 39.37007874015748143 ) ;
#50175 = DIRECTION ( 'NONE',  ( 0.000000000000000000, 0.000000000000000000, 1.000000000000000000 ) ) ;
#50176 = EDGE_CURVE ( 'NONE', #28842, #16345, #45961, .T. ) ;
#50177 = DIRECTION ( 'NONE',  ( 1.000000000000000000, -0.000000000000000000, 0.000000000000000000 ) ) ;
#50178 = VECTOR ( 'NONE', #28495, 39.37007874015748143 ) ;
#50179 = ORIENTED_EDGE ( 'NONE', *, *, #2198, .F. ) ;
#50180 = ORIENTED_EDGE ( 'NONE', *, *, #5102, .F. ) ;
#50181 = CARTESIAN_POINT ( 'NONE',  ( -0.3486774197067340486, 3.346456692913386100, -1.771653543307081025 ) ) ;
#50182 = CARTESIAN_POINT ( 'NONE',  ( -0.2727639067037607723, 0.000000000000000000, -0.7874015748031470974 ) ) ;
#50183 = EDGE_CURVE ( 'NONE', #19363, #1340, #49562, .T. ) ;
#50184 = LINE ( 'NONE', #15626, #19260 ) ;
#50185 = CARTESIAN_POINT ( 'NONE',  ( 2.378961647330872786, 3.267716535433070391, 0.5584465239797037350 ) ) ;
#50186 = VECTOR ( 'NONE', #1124, 39.37007874015748143 ) ;
#50187 = CARTESIAN_POINT ( 'NONE',  ( -1.345337514773770282, 0.1411726943947604063, 0.7317238754971241432 ) ) ;
#50188 = FACE_OUTER_BOUND ( 'NONE', #19627, .T. ) ;
#50189 = VERTEX_POINT ( 'NONE', #49816 ) ;
#50190 = ORIENTED_EDGE ( 'NONE', *, *, #5171, .T. ) ;
#50191 = DIRECTION ( 'NONE',  ( -3.986037398843765983E-20, -1.000000000000000000, -1.160734090543304660E-16 ) ) ;
#50192 = LINE ( 'NONE', #38134, #45410 ) ;
#50193 = ORIENTED_EDGE ( 'NONE', *, *, #25140, .T. ) ;
#50194 = DIRECTION ( 'NONE',  ( 0.000000000000000000, 0.000000000000000000, -1.000000000000000000 ) ) ;
#50195 = ORIENTED_EDGE ( 'NONE', *, *, #44697, .F. ) ;
#50196 = VERTEX_POINT ( 'NONE', #30751 ) ;
#50197 = ADVANCED_FACE ( 'NONE', ( #46462 ), #10375, .F. ) ;
#50198 = SHAPE_REPRESENTATION ( 'MAT-026', ( #33360, #11881, #32511, #22622, #348, #29206, #16838 ), #23415 ) ;
#50199 = VECTOR ( 'NONE', #17292, 39.37007874015748143 ) ;
#50200 = EDGE_LOOP ( 'NONE', ( #50801, #7123, #37729 ) ) ;
#50201 = VERTEX_POINT ( 'NONE', #34382 ) ;
#50202 = LINE ( 'NONE', #11013, #25276 ) ;
#50203 = PLANE ( 'NONE',  #40285 ) ;
#50204 = B_SPLINE_CURVE_WITH_KNOTS ( 'NONE', 3,
 ( #14969, #38472, #46425, #51028 ),
 .UNSPECIFIED., .F., .F.,
 ( 4, 4 ),
 ( 0.006151689351068225821, 0.007368043917412105820 ),
 .UNSPECIFIED. ) ;
#50205 = DIRECTION ( 'NONE',  ( 1.156482317317871478E-16, -0.000000000000000000, 1.000000000000000000 ) ) ;
#50206 = VECTOR ( 'NONE', #39774, 39.37007874015748143 ) ;
#50207 = CARTESIAN_POINT ( 'NONE',  ( 2.322368699764507216, 1.646673738916892837, -0.1535599007534338978 ) ) ;
#50208 = CARTESIAN_POINT ( 'NONE',  ( -0.1184164328040565317, 2.755905511811024056, -0.3547750388873516791 ) ) ;
#50209 = DIRECTION ( 'NONE',  ( 1.000000000000000000, 0.000000000000000000, 0.000000000000000000 ) ) ;
#50210 = EDGE_LOOP ( 'NONE', ( #15055, #28337, #35040, #45398 ) ) ;
#50211 = EDGE_CURVE ( 'NONE', #5100, #46567, #38004, .T. ) ;
#50212 = CARTESIAN_POINT ( 'NONE',  ( -1.091055626815042645, 3.346456692913386100, -7.512581982576723358E-16 ) ) ;
#50213 = LINE ( 'NONE', #11532, #20067 ) ;
#50214 = CARTESIAN_POINT ( 'NONE',  ( 1.287906020515829919, 0.000000000000000000, -1.771653543307081691 ) ) ;
#50215 = CARTESIAN_POINT ( 'NONE',  ( 2.926032761125787029, 0.000000000000000000, 0.3963580683592521914 ) ) ;
#50216 = ADVANCED_FACE ( 'NONE', ( #2625 ), #50072, .F. ) ;
#50217 = ORIENTED_EDGE ( 'NONE', *, *, #32043, .F. ) ;
#50218 = CARTESIAN_POINT ( 'NONE',  ( 0.8182917201112818173, 3.267716535433071279, -1.419509857074483292E-16 ) ) ;
#50219 = ADVANCED_FACE ( 'NONE', ( #26616 ), #42359, .F. ) ;
#50220 = CARTESIAN_POINT ( 'NONE',  ( 1.363819533518803251, 3.267716535433071279, 1.417322834645662777 ) ) ;
#50221 = EDGE_LOOP ( 'NONE', ( #24214, #31241, #46298, #29503 ) ) ;
#50222 = DIRECTION ( 'NONE',  ( -1.000000000000000000, -0.000000000000000000, -0.000000000000000000 ) ) ;
#50223 = EDGE_CURVE ( 'NONE', #21800, #7708, #12664, .T. ) ;
#50224 = CARTESIAN_POINT ( 'NONE',  ( -0.8182917201112814842, 0.000000000000000000, 1.732283464566921172 ) ) ;
#50225 = CYLINDRICAL_SURFACE ( 'NONE', #9255, 2.164630168518208109 ) ;
#50226 = VERTEX_POINT ( 'NONE', #8522 ) ;
#50227 = DIRECTION ( 'NONE',  ( 0.000000000000000000, 0.000000000000000000, -1.000000000000000000 ) ) ;
#50228 = PLANE ( 'NONE',  #34934 ) ;
#50229 = DIRECTION ( 'NONE',  ( 1.000000000000000000, 0.000000000000000000, 0.000000000000000000 ) ) ;
#50230 = CARTESIAN_POINT ( 'NONE',  ( 2.721588343797282317, 1.761660892206633910, -1.145422814530317579 ) ) ;
#50231 = ADVANCED_FACE ( 'NONE', ( #31769 ), #16266, .T. ) ;
#50232 = DIRECTION ( 'NONE',  ( -3.469446951953613696E-16, 0.000000000000000000, -1.000000000000000000 ) ) ;
#50233 = VECTOR ( 'NONE', #8910, 39.37007874015748143 ) ;
#50234 = ORIENTED_EDGE ( 'NONE', *, *, #38710, .F. ) ;
#50235 = CARTESIAN_POINT ( 'NONE',  ( -1.712496953225537188, 0.000000000000000000, 1.102362204724404160 ) ) ;
#50236 = EDGE_LOOP ( 'NONE', ( #5752, #363, #30835, #7312 ) ) ;
#50237 = ORIENTED_EDGE ( 'NONE', *, *, #13904, .T. ) ;
#50238 = CARTESIAN_POINT ( 'NONE',  ( 0.3734705886643994721, 0.000000000000000000, -0.02018660888377523527 ) ) ;
#50239 = ORIENTED_EDGE ( 'NONE', *, *, #20108, .T. ) ;
#50240 = EDGE_CURVE ( 'NONE', #49090, #41090, #47220, .T. ) ;
#50241 = CARTESIAN_POINT ( 'NONE',  ( -1.330356682269850044, 1.588168657012911877, -1.747353411991260819 ) ) ;
#50242 = CARTESIAN_POINT ( 'NONE',  ( -0.8942052331142552601, 0.000000000000000000, 2.204724409448808764 ) ) ;
#50243 = VERTEX_POINT ( 'NONE', #28386 ) ;
#50244 = B_SPLINE_CURVE_WITH_KNOTS ( 'NONE', 3,
 ( #17352, #17603, #49051, #41354 ),
 .UNSPECIFIED., .F., .F.,
 ( 4, 4 ),
 ( 0.001655661513764574181, 0.004155744767597255133 ),
 .UNSPECIFIED. ) ;
#50245 = AXIS2_PLACEMENT_3D ( 'NONE', #22958, #14708, #38711 ) ;
#50246 = DIRECTION ( 'NONE',  ( 1.000000000000000000, -0.000000000000000000, 0.000000000000000000 ) ) ;
#50247 = AXIS2_PLACEMENT_3D ( 'NONE', #20723, #36482, #9623 ) ;
#50248 = ADVANCED_FACE ( 'NONE', ( #44136 ), #47207, .F. ) ;
#50249 = CARTESIAN_POINT ( 'NONE',  ( -0.9360721529196992519, 0.000000000000000000, 1.470771056236103158 ) ) ;
#50250 = LINE ( 'NONE', #22683, #790 ) ;
#50251 = ORIENTED_EDGE ( 'NONE', *, *, #28903, .T. ) ;
#50252 = ORIENTED_EDGE ( 'NONE', *, *, #1597, .F. ) ;
#50253 = CARTESIAN_POINT ( 'NONE',  ( -1.220415235146723454, 0.5160455853568216567, -1.535490276664301046 ) ) ;
#50254 = FACE_BOUND ( 'NONE', #11680, .T. ) ;
#50255 = ORIENTED_EDGE ( 'NONE', *, *, #12688, .F. ) ;
#50256 = AXIS2_PLACEMENT_3D ( 'NONE', #8826, #40335, #22990 ) ;
#50257 = EDGE_CURVE ( 'NONE', #42367, #27577, #3888, .T. ) ;
#50258 = CARTESIAN_POINT ( 'NONE',  ( 0.5455278134075215446, 3.267716535433071279, -9.463399047163226878E-17 ) ) ;
#50259 = ORIENTED_EDGE ( 'NONE', *, *, #38082, .F. ) ;
#50260 = VERTEX_POINT ( 'NONE', #36151 ) ;
#50261 = PLANE ( 'NONE',  #37338 ) ;
#50262 = CARTESIAN_POINT ( 'NONE',  ( -2.258024766633058622, 3.346456692913386100, -0.1574803149606298636 ) ) ;
#50263 = EDGE_CURVE ( 'NONE', #5669, #50863, #47719, .T. ) ;
#50264 = ORIENTED_EDGE ( 'NONE', *, *, #40326, .F. ) ;
#50265 = CARTESIAN_POINT ( 'NONE',  ( -2.454875160333845674, 3.208895926198073845, -0.2895261247332783228 ) ) ;
#50267 = EDGE_CURVE ( 'NONE', #45778, #24752, #8779, .T. ) ;
#50266 = EDGE_LOOP ( 'NONE', ( #12513, #44059, #34126, #44438 ) ) ;
#50268 = CARTESIAN_POINT ( 'NONE',  ( 1.700185224778670401, 1.636708331897141377, -1.557456981387029149 ) ) ;
#50269 = FACE_OUTER_BOUND ( 'NONE', #13616, .T. ) ;
#50270 = DIRECTION ( 'NONE',  ( -3.469446951953613696E-16, 0.000000000000000000, -1.000000000000000000 ) ) ;
#50271 = ORIENTED_EDGE ( 'NONE', *, *, #45690, .F. ) ;
#50272 = ORIENTED_EDGE ( 'NONE', *, *, #25551, .F. ) ;
#50273 = DIRECTION ( 'NONE',  ( -3.469446951953613696E-16, 0.000000000000000000, -1.000000000000000000 ) ) ;
#50274 = CARTESIAN_POINT ( 'NONE',  ( -0.8942052331142549271, 3.267716535433071279, 3.102397620449222481E-16 ) ) ;
#50275 = PLANE ( 'NONE',  #3572 ) ;
#50276 = FACE_OUTER_BOUND ( 'NONE', #7790, .T. ) ;
#50277 = CARTESIAN_POINT ( 'NONE',  ( -2.882374421599337655, 1.575897850148979318, -0.6410571176358736967 ) ) ;
#50278 = ADVANCED_FACE ( 'NONE', ( #781 ), #27619, .F. ) ;
#50279 = VECTOR ( 'NONE', #30589, 39.37007874015748143 ) ;
#50280 = VECTOR ( 'NONE', #46766, 39.37007874015748854 ) ;
#50281 = DIRECTION ( 'NONE',  ( -1.000000000000000000, -0.000000000000000000, -0.000000000000000000 ) ) ;
#50282 = EDGE_CURVE ( 'NONE', #6857, #26667, #45591, .T. ) ;
#50283 = DIRECTION ( 'NONE',  ( -0.01601477604151182663, 0.9998717552508123996, -0.000000000000000000 ) ) ;
#50284 = ORIENTED_EDGE ( 'NONE', *, *, #49146, .T. ) ;
#50285 = CARTESIAN_POINT ( 'NONE',  ( -2.030479360727985849, 0.8677437501918828788, -1.240380476265474208 ) ) ;
#50286 = DIRECTION ( 'NONE',  ( -0.8268442224656336048, 0.000000000000000000, -0.5624310017906212211 ) ) ;
#50287 = CIRCLE ( 'NONE', #43723, 1.743387098533651480 ) ;
#50288 = VERTEX_POINT ( 'NONE', #11877 ) ;
#50289 = ORIENTED_EDGE ( 'NONE', *, *, #1144, .F. ) ;
#50290 = DIRECTION ( 'NONE',  ( 1.000000000000000000, 0.000000000000000000, -3.469446951953613696E-16 ) ) ;
#50291 = DIRECTION ( 'NONE',  ( 5.500355109725808462E-17, -1.000000000000000000, -1.022137253806221654E-16 ) ) ;
#50292 = ORIENTED_EDGE ( 'NONE', *, *, #28284, .T. ) ;
#50293 = ORIENTED_EDGE ( 'NONE', *, *, #31089, .T. ) ;
#50294 = LINE ( 'NONE', #18101, #33709 ) ;
#50295 = EDGE_LOOP ( 'NONE', ( #4168, #38073, #7205 ) ) ;
#50296 = CARTESIAN_POINT ( 'NONE',  ( -0.3486774197067339376, 3.267716535433071279, 2.077238655036873549 ) ) ;
#50297 = CARTESIAN_POINT ( 'NONE',  ( 1.626841099230391219, 0.01754038748813176174, 1.234417208607474059 ) ) ;
#50298 = ADVANCED_FACE ( 'NONE', ( #50809 ), #11628, .T. ) ;
#50299 = EDGE_LOOP ( 'NONE', ( #7373, #4593, #10816, #39313 ) ) ;
#50300 = B_SPLINE_CURVE_WITH_KNOTS ( 'NONE', 3,
 ( #17656, #45497, #33672, #14033 ),
 .UNSPECIFIED., .F., .F.,
 ( 4, 4 ),
 ( 0.1211775127643062722, 0.1625894504277921315 ),
 .UNSPECIFIED. ) ;
#50301 = CARTESIAN_POINT ( 'NONE',  ( 2.589735824746187909, 0.9850668145931131825, 0.4004656049141078200 ) ) ;
#50302 = VERTEX_POINT ( 'NONE', #35637 ) ;
#50303 = VERTEX_POINT ( 'NONE', #4393 ) ;
#50304 = FACE_OUTER_BOUND ( 'NONE', #34987, .T. ) ;
#50305 = CARTESIAN_POINT ( 'NONE',  ( 1.006250229852934774, 3.346456692913386100, 1.850393700787392293 ) ) ;
#50306 = PLANE ( 'NONE',  #21902 ) ;
#50307 = EDGE_CURVE ( 'NONE', #37535, #11433, #47466, .T. ) ;
#50308 = VECTOR ( 'NONE', #45420, 39.37007874015748143 ) ;
#50309 = ORIENTED_EDGE ( 'NONE', *, *, #36287, .F. ) ;
#50310 = VECTOR ( 'NONE', #27558, 39.37007874015748143 ) ;
#50311 = EDGE_CURVE ( 'NONE', #49770, #2009, #20027, .T. ) ;
#50312 = DIRECTION ( 'NONE',  ( -0.000000000000000000, -1.000000000000000000, -0.000000000000000000 ) ) ;
#50313 = DIRECTION ( 'NONE',  ( -3.469446951953613696E-16, 0.000000000000000000, -1.000000000000000000 ) ) ;
#50314 = EDGE_CURVE ( 'NONE', #39361, #3322, #27876, .T. ) ;
#50315 = ORIENTED_EDGE ( 'NONE', *, *, #16107, .T. ) ;
#50316 = CARTESIAN_POINT ( 'NONE',  ( 0.5455278134075211005, 3.346456692913386100, 0.4330708661417287386 ) ) ;
#50317 = EDGE_CURVE ( 'NONE', #3630, #2069, #34095, .T. ) ;
#50318 = ORIENTED_EDGE ( 'NONE', *, *, #16341, .T. ) ;
#50319 = VERTEX_POINT ( 'NONE', #4142 ) ;
#50320 = VECTOR ( 'NONE', #8138, 39.37007874015748143 ) ;
#50321 = CARTESIAN_POINT ( 'NONE',  ( 1.091055626815042645, 3.346456692913386100, 0.3149606299212578953 ) ) ;
#50322 = VECTOR ( 'NONE', #26019, 39.37007874015748143 ) ;
#50323 = DIRECTION ( 'NONE',  ( -0.000000000000000000, 1.000000000000000000, -0.000000000000000000 ) ) ;
#50324 = FACE_OUTER_BOUND ( 'NONE', #42599, .T. ) ;
#50325 = PLANE ( 'NONE',  #16472 ) ;
#50326 = VERTEX_POINT ( 'NONE', #24011 ) ;
#50327 = ORIENTED_EDGE ( 'NONE', *, *, #35026, .T. ) ;
#50328 = FILL_AREA_STYLE ('',( #30265 ) ) ;
#50329 = DIRECTION ( 'NONE',  ( -1.000000000000000000, -0.000000000000000000, -0.000000000000000000 ) ) ;
#50330 = VERTEX_POINT ( 'NONE', #20128 ) ;
#50331 = CARTESIAN_POINT ( 'NONE',  ( -2.454875160333845674, 3.242921367653845977, -0.03937007874015881204 ) ) ;
#50332 = DIRECTION ( 'NONE',  ( 1.042246309067994810E-16, 1.000000000000000000, 7.572362681945316160E-17 ) ) ;
#50333 = EDGE_CURVE ( 'NONE', #3555, #36460, #35894, .T. ) ;
#50334 = EDGE_CURVE ( 'NONE', #3322, #45259, #25039, .T. ) ;
#50335 = DIRECTION ( 'NONE',  ( -0.000000000000000000, 1.000000000000000000, -0.000000000000000000 ) ) ;
#50336 = DIRECTION ( 'NONE',  ( -0.5364534550056021533, 0.000000000000000000, -0.8439299085898972486 ) ) ;
#50337 = CARTESIAN_POINT ( 'NONE',  ( -0.07591351300297277671, 3.267716535433071279, 2.047244094488179567 ) ) ;
#50338 = ORIENTED_EDGE ( 'NONE', *, *, #3894, .T. ) ;
#50339 = ADVANCED_FACE ( 'NONE', ( #29424 ), #1799, .F. ) ;
#50340 = CARTESIAN_POINT ( 'NONE',  ( -0.6214413264104944323, 3.267716535433071279, 2.156057715732900533E-16 ) ) ;
#50341 = VECTOR ( 'NONE', #22573, 39.37007874015748143 ) ;
#50342 = CARTESIAN_POINT ( 'NONE',  ( -1.363819533518803029, 0.000000000000000000, 0.7874015748031456541 ) ) ;
#50343 = VECTOR ( 'NONE', #14595, 39.37007874015748143 ) ;
#50344 = ORIENTED_EDGE ( 'NONE', *, *, #23738, .F. ) ;
#50345 = DIRECTION ( 'NONE',  ( 0.9195277725514544587, 0.000000000000000000, -0.3930250316539147803 ) ) ;
#50346 = B_SPLINE_CURVE_WITH_KNOTS ( 'NONE', 3,
 ( #36727, #16335, #13234, #9350 ),
 .UNSPECIFIED., .F., .F.,
 ( 4, 4 ),
 ( 7.000820791675995278E-07, 0.002501003665680686262 ),
 .UNSPECIFIED. ) ;
#50347 = CARTESIAN_POINT ( 'NONE',  ( -0.7381027496704858359, 1.609316782724114825, -2.859439394060923512 ) ) ;
#50348 = CARTESIAN_POINT ( 'NONE',  ( 1.500384305870146040, 1.742635665041250670, 2.543203386703559943 ) ) ;
#50349 = VERTEX_POINT ( 'NONE', #45396 ) ;
#50350 = CARTESIAN_POINT ( 'NONE',  ( 0.000000000000000000, 3.267716535433071279, -0.8267716535433055070 ) ) ;
#50351 = VECTOR ( 'NONE', #25404, 39.37007874015748143 ) ;
#50352 = EDGE_LOOP ( 'NONE', ( #15647, #14096, #23001, #42004 ) ) ;
#50353 = LINE ( 'NONE', #42403, #44355 ) ;
#50354 = VECTOR ( 'NONE', #36662, 39.37007874015748143 ) ;
#50355 = ORIENTED_EDGE ( 'NONE', *, *, #33162, .F. ) ;
#50356 = DIRECTION ( 'NONE',  ( -3.469446951953613696E-16, 0.000000000000000000, -1.000000000000000000 ) ) ;
#50357 = EDGE_LOOP ( 'NONE', ( #28069, #18757, #3049, #48941 ) ) ;
#50358 = VECTOR ( 'NONE', #28041, 39.37007874015748143 ) ;
#50359 = DIRECTION ( 'NONE',  ( 1.000000000000000000, 0.000000000000000000, 0.000000000000000000 ) ) ;
#50360 = CARTESIAN_POINT ( 'NONE',  ( -0.2727639067037602727, 3.267716535433071279, 0.9055118110236167750 ) ) ;
#50361 = DIRECTION ( 'NONE',  ( -0.9195277725514544587, -4.558310254684937226E-17, 0.3930250316539147803 ) ) ;
#50362 = ORIENTED_EDGE ( 'NONE', *, *, #40220, .F. ) ;
#50363 = ORIENTED_EDGE ( 'NONE', *, *, #27459, .T. ) ;
#50364 = VERTEX_POINT ( 'NONE', #44640 ) ;
#50365 = DIRECTION ( 'NONE',  ( -0.000000000000000000, 1.000000000000000000, -0.000000000000000000 ) ) ;
#50366 = LINE ( 'NONE', #3182, #14729 ) ;
#50367 = VERTEX_POINT ( 'NONE', #45143 ) ;
#50368 = CARTESIAN_POINT ( 'NONE',  ( -3.927031490892378253E-16, 0.000000000000000000, -1.889763779527552146 ) ) ;
#50369 = CARTESIAN_POINT ( 'NONE',  ( -0.6808484915247774438, 0.01701463086705359146, 1.674057048625058552 ) ) ;
#50370 = CARTESIAN_POINT ( 'NONE',  ( 0.5455278134075217666, 3.267716535433071279, 1.574803149606291974 ) ) ;
#50371 = ORIENTED_EDGE ( 'NONE', *, *, #6634, .F. ) ;
#50372 = VERTEX_POINT ( 'NONE', #9294 ) ;
#50373 = EDGE_CURVE ( 'NONE', #12621, #17781, #28902, .T. ) ;
#50374 = LINE ( 'NONE', #22815, #50143 ) ;
#50375 = CARTESIAN_POINT ( 'NONE',  ( 0.000000000000000000, 3.267716535433071279, 2.047244094488179567 ) ) ;
#50376 = DIRECTION ( 'NONE',  ( -1.000000000000000000, 0.000000000000000000, -0.000000000000000000 ) ) ;
#50377 = EDGE_CURVE ( 'NONE', #22430, #8249, #24989, .T. ) ;
#50378 = ORIENTED_EDGE ( 'NONE', *, *, #17558, .T. ) ;
#50379 = CARTESIAN_POINT ( 'NONE',  ( 2.491402175429653809, 1.458524810485662959, -1.585592796919505609 ) ) ;
#50380 = EDGE_CURVE ( 'NONE', #8962, #34698, #10060, .T. ) ;
#50381 = FACE_OUTER_BOUND ( 'NONE', #21410, .T. ) ;
#50382 = ORIENTED_EDGE ( 'NONE', *, *, #1372, .T. ) ;
#50383 = CARTESIAN_POINT ( 'NONE',  ( 3.937007874015748143, 4.960629921259846142, -1.023622047244094224 ) ) ;
#50384 = ORIENTED_EDGE ( 'NONE', *, *, #13263, .T. ) ;
#50385 = VERTEX_POINT ( 'NONE', #48741 ) ;
#50386 = CARTESIAN_POINT ( 'NONE',  ( 4.268512490100411402E-16, 3.346456692913386100, 1.259842519685033357 ) ) ;
#50387 = DIRECTION ( 'NONE',  ( -0.9839295885986321100, 0.000000000000000000, 0.1785568947986229116 ) ) ;
#50388 = AXIS2_PLACEMENT_3D ( 'NONE', #35728, #12237, #9126 ) ;
#50389 = LINE ( 'NONE', #16090, #39606 ) ;
#50390 = CARTESIAN_POINT ( 'NONE',  ( 1.015142113812069313, 0.000000000000000000, -0.6692913385826764205 ) ) ;
#50391 = CARTESIAN_POINT ( 'NONE',  ( 1.015142113812069313, 3.267716535433071279, 0.2755905511810994302 ) ) ;
#50392 = ORIENTED_EDGE ( 'NONE', *, *, #4105, .T. ) ;
#50393 = VECTOR ( 'NONE', #25789, 39.37007874015748143 ) ;
#50394 = AXIS2_PLACEMENT_3D ( 'NONE', #1733, #33246, #14634 ) ;
#50395 = EDGE_CURVE ( 'NONE', #42867, #32098, #17301, .T. ) ;
#50396 = VERTEX_POINT ( 'NONE', #48489 ) ;
#50397 = PLANE ( 'NONE',  #36823 ) ;
#50398 = CARTESIAN_POINT ( 'NONE',  ( -1.062992125984251413, 0.5905511811023621549, 1.229331597148917955E-16 ) ) ;
#50399 = VECTOR ( 'NONE', #23340, 39.37007874015748143 ) ;
#50400 = EDGE_CURVE ( 'NONE', #35952, #28312, #35409, .T. ) ;
#50401 = B_SPLINE_CURVE_WITH_KNOTS ( 'NONE', 3,
 ( #21152, #28630, #25275, #36388 ),
 .UNSPECIFIED., .F., .F.,
 ( 4, 4 ),
 ( 2.472323665191410711E-07, 0.002500445596068602040 ),
 .UNSPECIFIED. ) ;
#50402 = EDGE_CURVE ( 'NONE', #49284, #39633, #21426, .T. ) ;
#50403 = DIRECTION ( 'NONE',  ( 0.01601477604151182663, -0.9998717552508123996, 0.000000000000000000 ) ) ;
#50404 = CARTESIAN_POINT ( 'NONE',  ( 0.8446807076687119498, 1.721431058233622746, 2.110586427442081803 ) ) ;
#50405 = VERTEX_POINT ( 'NONE', #41303 ) ;
#50406 = DIRECTION ( 'NONE',  ( 1.000000000000000000, 0.000000000000000000, -3.469446951953613696E-16 ) ) ;
#50407 = EDGE_CURVE ( 'NONE', #6760, #26747, #1288, .T. ) ;
#50408 = LINE ( 'NONE', #30847, #43791 ) ;
#50409 = ORIENTED_EDGE ( 'NONE', *, *, #24415, .F. ) ;
#50410 = PLANE ( 'NONE',  #28141 ) ;
#50411 = LINE ( 'NONE', #18972, #32773 ) ;
#50412 = LINE ( 'NONE', #3483, #41145 ) ;
#50413 = DIRECTION ( 'NONE',  ( 1.734723475976806848E-16, 0.000000000000000000, 1.000000000000000000 ) ) ;
#50414 = DIRECTION ( 'NONE',  ( -0.01601477604151182663, 0.9998717552508123996, -0.000000000000000000 ) ) ;
#50415 = LINE ( 'NONE', #2983, #6263 ) ;
#50416 = ORIENTED_EDGE ( 'NONE', *, *, #33273, .T. ) ;
#50417 = DIRECTION ( 'NONE',  ( 1.000000000000000000, -0.000000000000000000, 0.000000000000000000 ) ) ;
#50418 = ORIENTED_EDGE ( 'NONE', *, *, #29697, .F. ) ;
#50419 = FACE_BOUND ( 'NONE', #10511, .T. ) ;
#50420 = CARTESIAN_POINT ( 'NONE',  ( -0.8182917201112814842, 0.000000000000000000, 0.9055118110236167750 ) ) ;
#50421 = CARTESIAN_POINT ( 'NONE',  ( 0.000000000000000000, 3.267716535433071279, 0.9448818897637749625 ) ) ;
#50422 = VECTOR ( 'NONE', #39182, 39.37007874015748143 ) ;
#50423 = ORIENTED_EDGE ( 'NONE', *, *, #20895, .T. ) ;
#50424 = EDGE_LOOP ( 'NONE', ( #25469, #39743, #8453, #43233 ) ) ;
#50425 = CARTESIAN_POINT ( 'NONE',  ( -1.017106836739562814, 0.007823009827427474319, -1.483652934538973067 ) ) ;
#50426 = DIRECTION ( 'NONE',  ( 0.5128992774058948045, 0.000000000000000000, 0.8584487936018727616 ) ) ;
#50427 = AXIS2_PLACEMENT_3D ( 'NONE', #28268, #32423, #36291 ) ;
#50428 = DIRECTION ( 'NONE',  ( -0.000000000000000000, 1.000000000000000000, -0.000000000000000000 ) ) ;
#50429 = LINE ( 'NONE', #23365, #42517 ) ;
#50430 = DIRECTION ( 'NONE',  ( -0.000000000000000000, 0.000000000000000000, 1.000000000000000000 ) ) ;
#50431 = CARTESIAN_POINT ( 'NONE',  ( 0.07982360342473591996, 1.709180471932028711, 0.000000000000000000 ) ) ;
#50432 = AXIS2_PLACEMENT_3D ( 'NONE', #28420, #48271, #1062 ) ;
#50433 = ORIENTED_EDGE ( 'NONE', *, *, #43850, .F. ) ;
#50434 = CARTESIAN_POINT ( 'NONE',  ( 2.947574761915768171, 1.447536563168191126, -0.1816379373804911657 ) ) ;
#50435 = CARTESIAN_POINT ( 'NONE',  ( -0.07591351300297277671, 3.346456692913386100, 2.047244094488179567 ) ) ;
#50436 = FACE_OUTER_BOUND ( 'NONE', #33664, .T. ) ;
#50437 = EDGE_CURVE ( 'NONE', #13112, #9880, #17049, .T. ) ;
#50438 = EDGE_LOOP ( 'NONE', ( #32431, #3174, #29728, #20754 ) ) ;
#50439 = EDGE_CURVE ( 'NONE', #13554, #38641, #36923, .T. ) ;
#50440 = FACE_OUTER_BOUND ( 'NONE', #459, .T. ) ;
#50441 = EDGE_LOOP ( 'NONE', ( #6509, #16086, #2288, #3768 ) ) ;
#50442 = ORIENTED_EDGE ( 'NONE', *, *, #24521, .F. ) ;
#50443 = EDGE_CURVE ( 'NONE', #16466, #25584, #1548, .T. ) ;
#50444 = VERTEX_POINT ( 'NONE', #44894 ) ;
#50445 = VERTEX_POINT ( 'NONE', #20649 ) ;
#50446 = LINE ( 'NONE', #7645, #29401 ) ;
#50447 = B_SPLINE_CURVE_WITH_KNOTS ( 'NONE', 3,
 ( #38651, #38894, #15410, #23655 ),
 .UNSPECIFIED., .F., .F.,
 ( 4, 4 ),
 ( 3.432544043846355379E-07, 0.04340872033644440492 ),
 .UNSPECIFIED. ) ;
#50448 = LINE ( 'NONE', #46600, #18027 ) ;
#50449 = DIRECTION ( 'NONE',  ( -3.469446951953613696E-16, 0.000000000000000000, -1.000000000000000000 ) ) ;
#50450 = CIRCLE ( 'NONE', #13408, 2.164630168518208109 ) ;
#50451 = EDGE_CURVE ( 'NONE', #31614, #11498, #20911, .T. ) ;
#50452 = CARTESIAN_POINT ( 'NONE',  ( 2.118566926156530084, 0.5221770508638550190, -0.8519995351685487606 ) ) ;
#50453 = AXIS2_PLACEMENT_3D ( 'NONE', #16205, #31962, #40217 ) ;
#50454 = FACE_OUTER_BOUND ( 'NONE', #43224, .T. ) ;
#50455 = CARTESIAN_POINT ( 'NONE',  ( 1.516362329707282797, 1.735719643385797095, -2.003368222229618745 ) ) ;
#50456 = EDGE_LOOP ( 'NONE', ( #31712, #19507, #4297, #8143, #33715 ) ) ;
#50457 = CARTESIAN_POINT ( 'NONE',  ( 2.706338173250262269, 2.755905511811027164, -1.181102362204724088 ) ) ;
#50458 = DIRECTION ( 'NONE',  ( -8.032339854997315857E-17, 1.000000000000000000, -1.007223559679407077E-16 ) ) ;
#50459 = ADVANCED_FACE ( 'NONE', ( #36407 ), #5160, .F. ) ;
#50460 = VECTOR ( 'NONE', #44963, 39.37007874015748143 ) ;
#50461 = LINE ( 'NONE', #28038, #35881 ) ;
#50462 = LINE ( 'NONE', #19523, #29814 ) ;
#50463 = AXIS2_PLACEMENT_3D ( 'NONE', #7525, #39018, #11400 ) ;
#50464 = AXIS2_PLACEMENT_3D ( 'NONE', #16121, #39870, #36263 ) ;
#50465 = ORIENTED_EDGE ( 'NONE', *, *, #8752, .F. ) ;
#50466 = CARTESIAN_POINT ( 'NONE',  ( -0.8942052331142552601, 0.000000000000000000, -1.456692913385822186 ) ) ;
#50467 = PLANE ( 'NONE',  #30250 ) ;
#50468 = ORIENTED_EDGE ( 'NONE', *, *, #6348, .F. ) ;
#50469 = CARTESIAN_POINT ( 'NONE',  ( -1.909347346926325129, 3.267716535433071279, -0.8893194486674343979 ) ) ;
#50470 = CARTESIAN_POINT ( 'NONE',  ( 1.472697644137372697, 1.731489898814932316, 1.760436233057293354 ) ) ;
#50471 = VECTOR ( 'NONE', #11283, 39.37007874015748143 ) ;
#50472 = DIRECTION ( 'NONE',  ( 0.000000000000000000, 1.160734090543304660E-16, -1.000000000000000000 ) ) ;
#50473 = ORIENTED_EDGE ( 'NONE', *, *, #6, .F. ) ;
#50474 = DIRECTION ( 'NONE',  ( 1.000000000000000000, 0.000000000000000000, -3.469446951953613696E-16 ) ) ;
#50475 = DIRECTION ( 'NONE',  ( -0.01601477604151182663, 0.9998717552508123996, -0.000000000000000000 ) ) ;
#50476 = DIRECTION ( 'NONE',  ( -0.000000000000000000, 1.000000000000000000, -0.000000000000000000 ) ) ;
#50477 = DIRECTION ( 'NONE',  ( 1.734723475976806848E-16, 0.000000000000000000, 1.000000000000000000 ) ) ;
#50478 = CARTESIAN_POINT ( 'NONE',  ( -0.1184164328040565317, -0.6299212598425202314, -0.3547750388873516791 ) ) ;
#50479 = EDGE_LOOP ( 'NONE', ( #37030, #7434, #25279, #4816 ) ) ;
#50480 = ORIENTED_EDGE ( 'NONE', *, *, #50838, .F. ) ;
#50481 = ORIENTED_EDGE ( 'NONE', *, *, #22724, .T. ) ;
#50482 = CARTESIAN_POINT ( 'NONE',  ( -1.909347346926324906, 0.000000000000000000, -1.102362204724405492 ) ) ;
#50483 = ORIENTED_EDGE ( 'NONE', *, *, #5162, .F. ) ;
#50484 = CARTESIAN_POINT ( 'NONE',  ( 2.579472588755252050E-16, 0.000000000000000000, 2.106299212598425008 ) ) ;
#50485 = PLANE ( 'NONE',  #20304 ) ;
#50486 = VERTEX_POINT ( 'NONE', #29683 ) ;
#50487 = CARTESIAN_POINT ( 'NONE',  ( -0.2727639067037607723, 3.346456692913386100, -1.417322834645664331 ) ) ;
#50488 =( BOUNDED_CURVE ( )  B_SPLINE_CURVE ( 3, ( #12050, #30660, #35292, #11035 ),
 .UNSPECIFIED., .F., .F. ) 
 B_SPLINE_CURVE_WITH_KNOTS ( ( 4, 4 ),
 ( 3.094356967441856732, 3.141592653589793116 ),
 .UNSPECIFIED. ) 
 CURVE ( )  GEOMETRIC_REPRESENTATION_ITEM ( )  RATIONAL_B_SPLINE_CURVE ( ( 1.000000000000000000, 0.9998140744722292528, 0.9998140744722292528, 1.000000000000000000 ) ) 
 REPRESENTATION_ITEM ( '' )  );
#50489 = CARTESIAN_POINT ( 'NONE',  ( 0.000000000000000000, 3.267716535433071279, -8.878505979408855953E-16 ) ) ;
#50490 = B_SPLINE_CURVE_WITH_KNOTS ( 'NONE', 3,
 ( #43209, #27465, #46066, #22596 ),
 .UNSPECIFIED., .F., .F.,
 ( 4, 4 ),
 ( 4.753383040819987272E-07, 0.002500476700147301855 ),
 .UNSPECIFIED. ) ;
#50491 = VECTOR ( 'NONE', #35764, 39.37007874015748143 ) ;
#50492 = EDGE_CURVE ( 'NONE', #42344, #11143, #1033, .T. ) ;
#50493 = ORIENTED_EDGE ( 'NONE', *, *, #20631, .F. ) ;
#50495 = ORIENTED_EDGE ( 'NONE', *, *, #48463, .T. ) ;
#50494 = ADVANCED_FACE ( 'NONE', ( #48235 ), #12918, .F. ) ;
#50496 = DIRECTION ( 'NONE',  ( 1.734723475976806848E-16, -0.000000000000000000, 1.000000000000000000 ) ) ;
#50497 = FACE_BOUND ( 'NONE', #12342, .T. ) ;
#50498 = ORIENTED_EDGE ( 'NONE', *, *, #48452, .T. ) ;
#50499 = EDGE_CURVE ( 'NONE', #33697, #3514, #37455, .T. ) ;
#50500 = VECTOR ( 'NONE', #4918, 39.37007874015748143 ) ;
#50501 = AXIS2_PLACEMENT_3D ( 'NONE', #41508, #45355, #5632 ) ;
#50502 = DIRECTION ( 'NONE',  ( -1.000000000000000000, 0.000000000000000000, 0.000000000000000000 ) ) ;
#50504 = ORIENTED_EDGE ( 'NONE', *, *, #47909, .T. ) ;
#50503 = EDGE_CURVE ( 'NONE', #50302, #24946, #26311, .T. ) ;
#50505 = VERTEX_POINT ( 'NONE', #2820 ) ;
#50506 = CARTESIAN_POINT ( 'NONE',  ( 1.363819533518803251, 3.346456692913386100, 0.9055118110236164419 ) ) ;
#50507 = VECTOR ( 'NONE', #17134, 39.37007874015748143 ) ;
#50508 = CARTESIAN_POINT ( 'NONE',  ( 2.889674983507178219, 0.000000000000000000, -0.6090712660037610471 ) ) ;
#50509 = ORIENTED_EDGE ( 'NONE', *, *, #32634, .T. ) ;
#50510 = DIRECTION ( 'NONE',  ( -1.000000000000000000, -1.908195823574487557E-16, 0.000000000000000000 ) ) ;
#50511 = EDGE_LOOP ( 'NONE', ( #5917, #15447, #8762, #36573 ) ) ;
#50512 = CARTESIAN_POINT ( 'NONE',  ( -1.636583440222563635, 3.346456692913386100, 0.6299212598425164567 ) ) ;
#50513 = CARTESIAN_POINT ( 'NONE',  ( 0.07982360342473591996, 1.709180471932028711, 0.000000000000000000 ) ) ;
#50514 = EDGE_CURVE ( 'NONE', #5952, #14945, #13294, .T. ) ;
#50515 = DIRECTION ( 'NONE',  ( -3.469446951953613696E-16, 0.000000000000000000, -1.000000000000000000 ) ) ;
#50516 = ORIENTED_EDGE ( 'NONE', *, *, #5343, .T. ) ;
#50517 = EDGE_LOOP ( 'NONE', ( #41245, #23954, #33066, #29902 ) ) ;
#50518 = FACE_OUTER_BOUND ( 'NONE', #17334, .T. ) ;
#50519 = PLANE ( 'NONE',  #42750 ) ;
#50520 = CARTESIAN_POINT ( 'NONE',  ( 1.363819533518803251, 0.000000000000000000, 0.2755905511810996522 ) ) ;
#50521 = ADVANCED_FACE ( 'NONE', ( #35268 ), #45904, .F. ) ;
#50522 = CARTESIAN_POINT ( 'NONE',  ( -2.182111253630085734, 3.346456692913386100, -0.9448818897637762948 ) ) ;
#50523 = DIRECTION ( 'NONE',  ( -0.000000000000000000, -1.000000000000000000, -0.000000000000000000 ) ) ;
#50524 = LINE ( 'NONE', #4113, #14449 ) ;
#50525 = EDGE_CURVE ( 'NONE', #25220, #16985, #4050, .T. ) ;
#50526 = CARTESIAN_POINT ( 'NONE',  ( 1.979793062125284608, 5.905511811023623991, 2.191257344206569257 ) ) ;
#50527 = ORIENTED_EDGE ( 'NONE', *, *, #11516, .F. ) ;
#50528 = DIRECTION ( 'NONE',  ( 1.000000000000000000, 0.000000000000000000, 0.000000000000000000 ) ) ;
#50529 = CARTESIAN_POINT ( 'NONE',  ( -1.882988517681399188, 6.692913385826772199, 1.069164917025788863 ) ) ;
#50530 = CIRCLE ( 'NONE', #17654, 2.165354330708661568 ) ;
#50531 = ORIENTED_EDGE ( 'NONE', *, *, #43632, .T. ) ;
#50532 = EDGE_CURVE ( 'NONE', #619, #50396, #28357, .T. ) ;
#50533 = VECTOR ( 'NONE', #12779, 39.37007874015748143 ) ;
#50534 = ORIENTED_EDGE ( 'NONE', *, *, #28531, .F. ) ;
#50536 = AXIS2_PLACEMENT_3D ( 'NONE', #26013, #21387, #37650 ) ;
#50535 = DIRECTION ( 'NONE',  ( -1.000000000000000000, 0.000000000000000000, -0.000000000000000000 ) ) ;
#50537 = DIRECTION ( 'NONE',  ( 0.000000000000000000, 1.160734090543304660E-16, -1.000000000000000000 ) ) ;
#50538 = EDGE_LOOP ( 'NONE', ( #40196, #40538, #8473, #41841, #6472, #21139, #28677, #21370, #41478, #36810, #31309 ) ) ;
#50539 = VECTOR ( 'NONE', #47749, 39.37007874015748143 ) ;
#50540 = CARTESIAN_POINT ( 'NONE',  ( 0.8446807076687119498, 1.721431058233622746, 2.110586427442081803 ) ) ;
#50541 = ORIENTED_EDGE ( 'NONE', *, *, #2326, .F. ) ;
#50542 = DIRECTION ( 'NONE',  ( 1.734723475976806848E-16, -0.000000000000000000, 1.000000000000000000 ) ) ;
#50543 = ORIENTED_EDGE ( 'NONE', *, *, #19177, .T. ) ;
#50544 = CARTESIAN_POINT ( 'NONE',  ( -0.6214413264104939882, 3.346456692913386100, 1.102362204724404160 ) ) ;
#50545 = DIRECTION ( 'NONE',  ( 1.734723475976806848E-16, -0.000000000000000000, 1.000000000000000000 ) ) ;
#50546 = VERTEX_POINT ( 'NONE', #30187 ) ;
#50547 = CARTESIAN_POINT ( 'NONE',  ( 1.560669927219590303, 3.267716535433071279, -1.299212598425193210 ) ) ;
#50548 = ORIENTED_EDGE ( 'NONE', *, *, #46831, .F. ) ;
#50549 = VERTEX_POINT ( 'NONE', #31391 ) ;
#50550 = CARTESIAN_POINT ( 'NONE',  ( 1.295932559091726111, 1.640989118791050583, -2.653223575520714750 ) ) ;
#50551 = FACE_OUTER_BOUND ( 'NONE', #11291, .T. ) ;
#50552 = CARTESIAN_POINT ( 'NONE',  ( -1.909347346926324462, 3.267716535433071279, 3.312189666507127188E-16 ) ) ;
#50553 = EDGE_CURVE ( 'NONE', #25411, #1622, #42059, .T. ) ;
#50554 = VERTEX_POINT ( 'NONE', #10567 ) ;
#50555 = CARTESIAN_POINT ( 'NONE',  ( 1.966928503432568975, 3.346456692913386100, 0.9055118110236164419 ) ) ;
#50556 = CARTESIAN_POINT ( 'NONE',  ( 1.930379001735549993, 1.749335058599799320, 2.234429108645952677 ) ) ;
#50557 = ADVANCED_FACE ( 'NONE', ( #37947 ), #38202, .F. ) ;
#50558 = ADVANCED_FACE ( 'NONE', ( #14693 ), #3771, .F. ) ;
#50559 = ORIENTED_EDGE ( 'NONE', *, *, #45120, .T. ) ;
#50560 = DIRECTION ( 'NONE',  ( -0.000000000000000000, -1.000000000000000000, -0.000000000000000000 ) ) ;
#50561 = AXIS2_PLACEMENT_3D ( 'NONE', #50948, #19756, #49503 ) ;
#50562 = VECTOR ( 'NONE', #23771, 39.37007874015748143 ) ;
#50563 = EDGE_LOOP ( 'NONE', ( #6733, #49720, #20534, #23759 ) ) ;
#50564 = VECTOR ( 'NONE', #32366, 39.37007874015748143 ) ;
#50565 = ORIENTED_EDGE ( 'NONE', *, *, #20568, .T. ) ;
#50566 = VECTOR ( 'NONE', #12245, 39.37007874015748143 ) ;
#50567 = ORIENTED_EDGE ( 'NONE', *, *, #45756, .F. ) ;
#50568 = DIRECTION ( 'NONE',  ( 0.000000000000000000, 0.000000000000000000, 1.000000000000000000 ) ) ;
#50569 = VECTOR ( 'NONE', #49283, 39.37007874015748143 ) ;
#50570 = CARTESIAN_POINT ( 'NONE',  ( -1.091055626815042645, 0.000000000000000000, -1.574803149606293529 ) ) ;
#50571 = CARTESIAN_POINT ( 'NONE',  ( -0.8182917201112819283, 0.000000000000000000, -1.299212598425193210 ) ) ;
#50572 = LINE ( 'NONE', #15268, #33810 ) ;
#50573 = ORIENTED_EDGE ( 'NONE', *, *, #50317, .T. ) ;
#50574 = EDGE_LOOP ( 'NONE', ( #23033, #25383, #47325, #19773, #18377, #50929, #44329, #27190, #50493, #40924, #23538, #11702, #12354, #50193, #1564, #18722, #25703, #25107, #4945, #42679, #14456, #34308, #14624, #48070, #25258, #1217, #14314, #25273, #38848, #32103, #16412, #47604, #44498, #34614, #18857, #41227, #45048, #26245, #32157, #16080, #43291, #35508, #987, #14799, #16819, #20801, #30190, #2479, #15396, #51013, #24064, #43295, #39219, #32198, #21338, #5104, #30605, #26043, #16441, #17382, #49822, #38451, #25829, #22134, #38816, #48773, #35978, #26065, #7415, #3183, #32812, #47781, #9924, #17345, #85, #29084, #32148, #40589, #28650, #10436, #4423, #4377, #45949, #21096, #19623, #40670, #11879, #44454, #47059, #29285, #45886, #42092, #38932, #9815, #24197, #29027, #49044, #2706, #12965, #48646, #11201, #5443, #848, #11560, #10815, #50465, #30365, #47910, #4119, #19610, #33054, #13061, #48064, #14995, #5728, #7860, #38131, #32711, #12732, #29751, #40428, #40759, #24218, #25089, #45137, #144, #48500, #12473, #31996, #44076, #44278, #7021, #35440, #41693, #579, #43636, #48783, #18874, #33459, #50593, #44245, #10423, #26135, #10547, #4692, #42856, #7893, #14031, #39012, #34962, #27672, #26802, #10249, #30184, #32778, #15695, #42273 ) ) ;
#50575 = VECTOR ( 'NONE', #3860, 39.37007874015748143 ) ;
#50576 = LINE ( 'NONE', #23513, #15588 ) ;
#50577 = LINE ( 'NONE', #15272, #11924 ) ;
#50578 = VERTEX_POINT ( 'NONE', #4029 ) ;
#50579 = DIRECTION ( 'NONE',  ( -0.000000000000000000, 1.000000000000000000, -0.000000000000000000 ) ) ;
#50580 = CARTESIAN_POINT ( 'NONE',  ( 2.032117719318057958, 0.000000000000000000, 0.6430507823692680480 ) ) ;
#50581 = EDGE_CURVE ( 'NONE', #18289, #48175, #23376, .T. ) ;
#50582 = CARTESIAN_POINT ( 'NONE',  ( -0.2727639067037607723, 3.267716535433071279, -1.732283464566922726 ) ) ;
#50583 = DIRECTION ( 'NONE',  ( -0.9998717552508122886, -0.01601477604151182316, 0.000000000000000000 ) ) ;
#50584 = DIRECTION ( 'NONE',  ( -0.000000000000000000, 1.000000000000000000, -0.000000000000000000 ) ) ;
#50585 = VERTEX_POINT ( 'NONE', #31647 ) ;
#50586 = CARTESIAN_POINT ( 'NONE',  ( -1.363819533518803473, 3.346456692913386100, 1.732283464566920950 ) ) ;
#50587 = FACE_OUTER_BOUND ( 'NONE', #49517, .T. ) ;
#50588 = EDGE_CURVE ( 'NONE', #3179, #5174, #22193, .T. ) ;
#50589 = ORIENTED_EDGE ( 'NONE', *, *, #38435, .T. ) ;
#50590 = DIRECTION ( 'NONE',  ( 1.000000000000000000, 0.000000000000000000, 0.000000000000000000 ) ) ;
#50591 = CARTESIAN_POINT ( 'NONE',  ( 1.956098637639549720, 1.739232450405700847, -1.232242025355393844 ) ) ;
#50592 = CYLINDRICAL_SURFACE ( 'NONE', #36239, 2.165354330708661568 ) ;
#50594 = EDGE_CURVE ( 'NONE', #39889, #44367, #18571, .T. ) ;
#50593 = ORIENTED_EDGE ( 'NONE', *, *, #48266, .T. ) ;
#50595 = VECTOR ( 'NONE', #2205, 39.37007874015748143 ) ;
#50596 = ADVANCED_FACE ( 'NONE', ( #50013 ), #27249, .T. ) ;
#50597 = VERTEX_POINT ( 'NONE', #19505 ) ;
#50598 = CIRCLE ( 'NONE', #11124, 2.164630168518208109 ) ;
#50599 = DIRECTION ( 'NONE',  ( 0.000000000000000000, -1.000000000000000000, 0.000000000000000000 ) ) ;
#50600 = VERTEX_POINT ( 'NONE', #37696 ) ;
#50601 = DIRECTION ( 'NONE',  ( 0.01601477604151182663, -0.9998717552508123996, 0.000000000000000000 ) ) ;
#50602 = AXIS2_PLACEMENT_3D ( 'NONE', #24711, #40462, #5081 ) ;
#50603 = ORIENTED_EDGE ( 'NONE', *, *, #532, .F. ) ;
#50604 = EDGE_CURVE ( 'NONE', #15792, #12349, #27502, .T. ) ;
#50605 = CARTESIAN_POINT ( 'NONE',  ( 0.7423782071083087075, 0.000000000000000000, -0.6299212598425181220 ) ) ;
#50606 = LINE ( 'NONE', #34676, #31332 ) ;
#50607 = LINE ( 'NONE', #31050, #49897 ) ;
#50608 = EDGE_LOOP ( 'NONE', ( #35912, #1540, #16571, #4219 ) ) ;
#50609 = ORIENTED_EDGE ( 'NONE', *, *, #36503, .F. ) ;
#50610 = ORIENTED_EDGE ( 'NONE', *, *, #50110, .F. ) ;
#50611 = CARTESIAN_POINT ( 'NONE',  ( 2.139229417893225627, 0.000000000000000000, -0.3394403656973398742 ) ) ;
#50612 = VECTOR ( 'NONE', #7011, 39.37007874015748143 ) ;
#50613 = CARTESIAN_POINT ( 'NONE',  ( 0.08119777152254364916, 1.623385212329073957, 0.000000000000000000 ) ) ;
#50614 = ORIENTED_EDGE ( 'NONE', *, *, #33906, .T. ) ;
#50615 = ORIENTED_EDGE ( 'NONE', *, *, #38294, .F. ) ;
#50616 = LINE ( 'NONE', #46521, #13268 ) ;
#50617 = DIRECTION ( 'NONE',  ( 1.734723475976806848E-16, 0.000000000000000000, 1.000000000000000000 ) ) ;
#50618 = CARTESIAN_POINT ( 'NONE',  ( -2.950847925457031007, 1.574821451496988933, -0.08326053095501942392 ) ) ;
#50619 = EDGE_CURVE ( 'NONE', #20464, #33352, #7894, .T. ) ;
#50620 = VERTEX_POINT ( 'NONE', #21054 ) ;
#50621 = ORIENTED_EDGE ( 'NONE', *, *, #14472, .F. ) ;
#50622 = DIRECTION ( 'NONE',  ( -3.469446951953613696E-16, 0.000000000000000000, -1.000000000000000000 ) ) ;
#50623 = CARTESIAN_POINT ( 'NONE',  ( -2.100227814008681193, 5.905511811023623991, -2.076109931251944207 ) ) ;
#50624 = DIRECTION ( 'NONE',  ( -2.214792131866782686E-16, 0.6427876096865404731, 0.7660444431189771253 ) ) ;
#50625 = ADVANCED_FACE ( 'NONE', ( #32169 ), #403, .F. ) ;
#50626 = EDGE_CURVE ( 'NONE', #33537, #48962, #12285, .T. ) ;
#50627 = EDGE_LOOP ( 'NONE', ( #11371, #32601, #19675, #13527 ) ) ;
#50628 = CARTESIAN_POINT ( 'NONE',  ( -1.091055626815042645, 3.267716535433071279, 2.186531193194249045 ) ) ;
#50629 = ORIENTED_EDGE ( 'NONE', *, *, #33020, .T. ) ;
#50630 = EDGE_CURVE ( 'NONE', #49614, #28289, #15172, .T. ) ;
#50631 = CARTESIAN_POINT ( 'NONE',  ( -0.6808484915247774438, 0.01701463086705359146, 1.674057048625058552 ) ) ;
#50632 = ORIENTED_EDGE ( 'NONE', *, *, #20606, .F. ) ;
#50633 = VERTEX_POINT ( 'NONE', #48370 ) ;
#50634 = LINE ( 'NONE', #19695, #39420 ) ;
#50635 = LINE ( 'NONE', #34701, #42363 ) ;
#50636 = DIRECTION ( 'NONE',  ( -0.000000000000000000, -1.000000000000000000, -0.000000000000000000 ) ) ;
#50637 = DIRECTION ( 'NONE',  ( -0.01601477604151182663, 0.9998717552508123996, -0.000000000000000000 ) ) ;
#50638 = CARTESIAN_POINT ( 'NONE',  ( -0.5455278134075214336, 3.267716535433071279, 9.463399047163225645E-17 ) ) ;
#50639 = ORIENTED_EDGE ( 'NONE', *, *, #2015, .T. ) ;
#50640 = VECTOR ( 'NONE', #47225, 39.37007874015748143 ) ;
#50641 = VECTOR ( 'NONE', #8284, 39.37007874015748143 ) ;
#50642 = ORIENTED_EDGE ( 'NONE', *, *, #27134, .F. ) ;
#50643 = CARTESIAN_POINT ( 'NONE',  ( 0.1968503937007877735, 3.346456692913386100, 1.377952755905504256 ) ) ;
#50644 = DIRECTION ( 'NONE',  ( -0.7071067811865483499, 0.7071067811865466846, 8.177564888978005264E-17 ) ) ;
#50645 = VECTOR ( 'NONE', #23110, 39.37007874015748143 ) ;
#50646 = EDGE_CURVE ( 'NONE', #19878, #17854, #40724, .T. ) ;
#50647 = LINE ( 'NONE', #15345, #43240 ) ;
#50648 = LINE ( 'NONE', #46802, #48379 ) ;
#50649 = CARTESIAN_POINT ( 'NONE',  ( -1.636583440222564301, 0.000000000000000000, -1.771653543307080581 ) ) ;
#50650 = VECTOR ( 'NONE', #43541, 39.37007874015748143 ) ;
#50651 = VERTEX_POINT ( 'NONE', #43504 ) ;
#50652 = DIRECTION ( 'NONE',  ( 0.000000000000000000, 1.000000000000000000, 0.000000000000000000 ) ) ;
#50653 = DIRECTION ( 'NONE',  ( -3.469446951953613696E-16, 0.000000000000000000, -1.000000000000000000 ) ) ;
#50654 = ADVANCED_FACE ( 'NONE', ( #24157 ), #31914, .F. ) ;
#50655 = ORIENTED_EDGE ( 'NONE', *, *, #18107, .F. ) ;
#50656 = CARTESIAN_POINT ( 'NONE',  ( -0.1515599155143076138, 1.705474441417569320, -2.232975473887063966 ) ) ;
#50657 = ADVANCED_FACE ( 'NONE', ( #17181 ), #661, .T. ) ;
#50658 = LINE ( 'NONE', #7859, #44281 ) ;
#50659 = CARTESIAN_POINT ( 'NONE',  ( 0.1067246931122726866, 0.02962905676920215767, 0.000000000000000000 ) ) ;
#50660 = EDGE_CURVE ( 'NONE', #14380, #43306, #28792, .T. ) ;
#50661 = LINE ( 'NONE', #27219, #41582 ) ;
#50662 = DIRECTION ( 'NONE',  ( -0.9998717552508122886, -0.01601477604151180928, 0.000000000000000000 ) ) ;
#50663 = DIRECTION ( 'NONE',  ( 1.000000000000000000, -0.000000000000000000, 0.000000000000000000 ) ) ;
#50664 = ORIENTED_EDGE ( 'NONE', *, *, #30172, .T. ) ;
#50665 = FACE_OUTER_BOUND ( 'NONE', #25047, .T. ) ;
#50666 = VERTEX_POINT ( 'NONE', #39900 ) ;
#50667 = CARTESIAN_POINT ( 'NONE',  ( 0.4696143004045478797, 3.267716535433071279, -0.3543307086614173040 ) ) ;
#50668 = CARTESIAN_POINT ( 'NONE',  ( 0.1067246931122726866, 0.02962905676920215767, 0.000000000000000000 ) ) ;
#50669 = LINE ( 'NONE', #23874, #31773 ) ;
#50670 = ORIENTED_EDGE ( 'NONE', *, *, #20099, .T. ) ;
#50671 = ORIENTED_EDGE ( 'NONE', *, *, #79, .T. ) ;
#50672 = DIRECTION ( 'NONE',  ( 1.000000000000000000, 0.000000000000000000, 0.000000000000000000 ) ) ;
#50673 = VECTOR ( 'NONE', #39153, 39.37007874015748143 ) ;
#50674 = LINE ( 'NONE', #15378, #50960 ) ;
#50675 = AXIS2_PLACEMENT_3D ( 'NONE', #4137, #31763, #35887 ) ;
#50676 = CARTESIAN_POINT ( 'NONE',  ( -1.166969139818015977, 3.267716535433071279, -1.417322834645664109 ) ) ;
#50677 = CARTESIAN_POINT ( 'NONE',  ( 0.6651440564695696445, 1.049866565877818347, 1.912327270024466008 ) ) ;
#50678 = EDGE_CURVE ( 'NONE', #2997, #47957, #31117, .T. ) ;
#50679 = DIRECTION ( 'NONE',  ( -0.3090169943749447312, 0.000000000000000000, -0.9510565162951544194 ) ) ;
#50680 = AXIS2_PLACEMENT_3D ( 'NONE', #38052, #18418, #22798 ) ;
#50681 = PLANE ( 'NONE',  #21523 ) ;
#50682 = VERTEX_POINT ( 'NONE', #8158 ) ;
#50683 = ORIENTED_EDGE ( 'NONE', *, *, #46676, .F. ) ;
#50684 = CARTESIAN_POINT ( 'NONE',  ( -2.734482843737247038, 1.578211097029592169, -1.115254632218712016 ) ) ;
#50685 = CIRCLE ( 'NONE', #26850, 2.164630168518208109 ) ;
#50686 = EDGE_CURVE ( 'NONE', #50319, #2087, #28529, .T. ) ;
#50687 = CARTESIAN_POINT ( 'NONE',  ( -0.6214413264104945434, 0.000000000000000000, -0.4724409448818886470 ) ) ;
#50688 = AXIS2_PLACEMENT_3D ( 'NONE', #37610, #38363, #9975 ) ;
#50689 = ORIENTED_EDGE ( 'NONE', *, *, #49361, .T. ) ;
#50690 = ADVANCED_FACE ( 'NONE', ( #47607 ), #40168, .T. ) ;
#50691 = CARTESIAN_POINT ( 'NONE',  ( -1.350373579275921276, 0.006290961278228680842, 1.139832270491418553 ) ) ;
#50692 = VERTEX_POINT ( 'NONE', #20276 ) ;
#50693 = VERTEX_POINT ( 'NONE', #24674 ) ;
#50694 = ORIENTED_EDGE ( 'NONE', *, *, #7625, .F. ) ;
#50695 = ORIENTED_EDGE ( 'NONE', *, *, #30682, .F. ) ;
#50696 = CARTESIAN_POINT ( 'NONE',  ( 1.287906020515830141, 0.000000000000000000, -0.8267716535433055070 ) ) ;
#50697 = ORIENTED_EDGE ( 'NONE', *, *, #45690, .T. ) ;
#50698 = LINE ( 'NONE', #18767, #24617 ) ;
#50699 = PLANE ( 'NONE',  #42554 ) ;
#50700 = FACE_OUTER_BOUND ( 'NONE', #47572, .T. ) ;
#50701 = CARTESIAN_POINT ( 'NONE',  ( 0.7423782071083087075, 0.000000000000000000, -6.146657985744592735E-16 ) ) ;
#50702 = DIRECTION ( 'NONE',  ( -1.000000000000000000, 0.000000000000000000, -0.000000000000000000 ) ) ;
#50703 = CARTESIAN_POINT ( 'NONE',  ( -0.07591351300297333182, 0.000000000000000000, -1.732283464566922726 ) ) ;
#50704 = CIRCLE ( 'NONE', #28506, 2.246510896728926010 ) ;
#50705 = VERTEX_POINT ( 'NONE', #13308 ) ;
#50706 = LINE ( 'NONE', #7409, #50471 ) ;
#50707 = LINE ( 'NONE', #23147, #48896 ) ;
#50708 = AXIS2_PLACEMENT_3D ( 'NONE', #33067, #10580, #42069 ) ;
#50709 = CARTESIAN_POINT ( 'NONE',  ( -0.6214413264104945434, 3.346456692913386100, -0.6692913385826760875 ) ) ;
#50710 = VECTOR ( 'NONE', #1154, 39.37007874015748143 ) ;
#50711 = CARTESIAN_POINT ( 'NONE',  ( -1.030301126714985971, 0.000000000000000000, -1.501813316714599500 ) ) ;
#50712 = ORIENTED_EDGE ( 'NONE', *, *, #36314, .F. ) ;
#50713 = DIRECTION ( 'NONE',  ( -1.000000000000000000, -0.000000000000000000, -0.000000000000000000 ) ) ;
#50714 = ADVANCED_FACE ( 'NONE', ( #16418 ), #4277, .F. ) ;
#50715 = LINE ( 'NONE', #50974, #19506 ) ;
#50716 = VERTEX_POINT ( 'NONE', #8661 ) ;
#50717 = CARTESIAN_POINT ( 'NONE',  ( -1.636583440222564301, 3.267716535433071279, 2.839019714148967077E-16 ) ) ;
#50718 = VECTOR ( 'NONE', #48216, 39.37007874015748143 ) ;
#50719 = CARTESIAN_POINT ( 'NONE',  ( 1.112246780768851195, 0.5224230866457337807, 1.957537375840811888 ) ) ;
#50720 = EDGE_CURVE ( 'NONE', #739, #180, #4792, .T. ) ;
#50721 = VECTOR ( 'NONE', #22177, 39.37007874015748143 ) ;
#50722 = ADVANCED_FACE ( 'NONE', ( #40427 ), #36294, .F. ) ;
#50723 = PRODUCT ( 'Stand', 'Stand', '', ( #27884 ) ) ;
#50724 = DIRECTION ( 'NONE',  ( 0.000000000000000000, 1.160734090543304660E-16, -1.000000000000000000 ) ) ;
#50725 = EDGE_LOOP ( 'NONE', ( #23748, #30689, #28490, #37191 ) ) ;
#50726 = LINE ( 'NONE', #696, #38001 ) ;
#50727 = CARTESIAN_POINT ( 'NONE',  ( 1.833433833923351353, 0.000000000000000000, 1.574803149606291974 ) ) ;
#50728 = DIRECTION ( 'NONE',  ( 0.9510565162951500895, 0.000000000000000000, 0.3090169943749582204 ) ) ;
#50729 = DIRECTION ( 'NONE',  ( -0.9362348706397368714, 4.082259235907190839E-17, -0.3513748240813434620 ) ) ;
#50730 = VERTEX_POINT ( 'NONE', #20794 ) ;
#50731 = VERTEX_POINT ( 'NONE', #36551 ) ;
#50732 = ORIENTED_EDGE ( 'NONE', *, *, #48775, .F. ) ;
#50733 = CARTESIAN_POINT ( 'NONE',  ( 1.015142113812069313, 0.000000000000000000, 0.7874015748031454320 ) ) ;
#50734 = ORIENTED_EDGE ( 'NONE', *, *, #42795, .T. ) ;
#50735 = CARTESIAN_POINT ( 'NONE',  ( -2.165354330708661568, 1.574803149606301966, -1.520079223026944511E-17 ) ) ;
#50736 = EDGE_CURVE ( 'NONE', #5605, #24001, #45902, .T. ) ;
#50737 = LINE ( 'NONE', #4581, #47456 ) ;
#50738 = ORIENTED_EDGE ( 'NONE', *, *, #1309, .F. ) ;
#50739 = CARTESIAN_POINT ( 'NONE',  ( 0.000000000000000000, 0.000000000000000000, -0.7480314960629920185 ) ) ;
#50740 = EDGE_CURVE ( 'NONE', #1528, #13306, #6063, .T. ) ;
#50741 = EDGE_LOOP ( 'NONE', ( #1233, #26026, #17552, #22401 ) ) ;
#50742 = DIRECTION ( 'NONE',  ( 0.000000000000000000, 0.000000000000000000, -1.000000000000000000 ) ) ;
#50743 = VECTOR ( 'NONE', #6010, 39.37007874015748143 ) ;
#50744 = VERTEX_POINT ( 'NONE', #6584 ) ;
#50745 = EDGE_LOOP ( 'NONE', ( #36710, #32872, #226, #34076 ) ) ;
#50746 = VECTOR ( 'NONE', #32179, 39.37007874015748143 ) ;
#50747 = EDGE_CURVE ( 'NONE', #45160, #24001, #20230, .T. ) ;
#50748 = DIRECTION ( 'NONE',  ( 0.000000000000000000, 0.000000000000000000, -1.000000000000000000 ) ) ;
#50749 = ORIENTED_EDGE ( 'NONE', *, *, #21500, .F. ) ;
#50750 = EDGE_CURVE ( 'NONE', #34200, #36526, #38078, .T. ) ;
#50751 = AXIS2_PLACEMENT_3D ( 'NONE', #25096, #21226, #20967 ) ;
#50752 = DIRECTION ( 'NONE',  ( -0.000000000000000000, 1.000000000000000000, -0.000000000000000000 ) ) ;
#50753 = VECTOR ( 'NONE', #41527, 39.37007874015748143 ) ;
#50754 = VERTEX_POINT ( 'NONE', #41941 ) ;
#50755 = ORIENTED_EDGE ( 'NONE', *, *, #20041, .T. ) ;
#50756 = DIRECTION ( 'NONE',  ( 0.000000000000000000, 0.000000000000000000, 1.000000000000000000 ) ) ;
#50757 = CIRCLE ( 'NONE', #40927, 2.165354330708661568 ) ;
#50758 = FACE_OUTER_BOUND ( 'NONE', #2688, .T. ) ;
#50759 = ORIENTED_EDGE ( 'NONE', *, *, #21251, .T. ) ;
#50760 = DIRECTION ( 'NONE',  ( -0.9998717552508122886, -0.01601477604151182316, 0.000000000000000000 ) ) ;
#50761 = ORIENTED_EDGE ( 'NONE', *, *, #9783, .F. ) ;
#50762 = CARTESIAN_POINT ( 'NONE',  ( 0.000000000000000000, 3.267716535433071279, -1.102362204724405714 ) ) ;
#50763 = DIRECTION ( 'NONE',  ( 1.000000000000000000, -0.000000000000000000, 0.000000000000000000 ) ) ;
#50764 = CARTESIAN_POINT ( 'NONE',  ( -1.368795925040221295, 1.049866565877818347, 1.491914849825318967 ) ) ;
#50765 = ORIENTED_EDGE ( 'NONE', *, *, #22087, .F. ) ;
#50766 = ORIENTED_EDGE ( 'NONE', *, *, #41135, .F. ) ;
#50767 = B_SPLINE_CURVE_WITH_KNOTS ( 'NONE', 3,
 ( #33051, #28639, #5406, #20902 ),
 .UNSPECIFIED., .F., .F.,
 ( 4, 4 ),
 ( 0.0004892548405474798738, 0.0008567996338181287259 ),
 .UNSPECIFIED. ) ;
#50768 = CARTESIAN_POINT ( 'NONE',  ( 0.7423782071083085965, 3.267716535433071279, 0.4330708661417287386 ) ) ;
#50769 = CARTESIAN_POINT ( 'NONE',  ( 0.000000000000000000, 6.692913385826772199, 0.000000000000000000 ) ) ;
#50770 = CARTESIAN_POINT ( 'NONE',  ( -1.195183497228115035E-16, 0.000000000000000000, -1.574803149606293529 ) ) ;
#50771 = DIRECTION ( 'NONE',  ( 1.734723475976806848E-16, -0.000000000000000000, 1.000000000000000000 ) ) ;
#50772 = LINE ( 'NONE', #30467, #33068 ) ;
#50773 = CARTESIAN_POINT ( 'NONE',  ( -0.3136974817027967100, 1.714375164834789356, -2.936457595020224520 ) ) ;
#50774 = CIRCLE ( 'NONE', #31875, 2.106299212598425008 ) ;
#50775 = CARTESIAN_POINT ( 'NONE',  ( 0.08139965876239094178, 1.610780518492231694, 0.000000000000000000 ) ) ;
#50776 = EDGE_CURVE ( 'NONE', #27786, #15713, #13562, .T. ) ;
#50777 = ORIENTED_EDGE ( 'NONE', *, *, #6454, .F. ) ;
#50778 = CONICAL_SURFACE ( 'NONE', #10464, 2.246510896728926010, 0.01601546068027819014 ) ;
#50779 = CARTESIAN_POINT ( 'NONE',  ( 1.909347346926324684, 3.346456692913386100, 1.102362204724403938 ) ) ;
#50780 = ADVANCED_FACE ( 'NONE', ( #9432 ), #25055, .F. ) ;
#50781 = VECTOR ( 'NONE', #34964, 39.37007874015748143 ) ;
#50782 = ORIENTED_EDGE ( 'NONE', *, *, #50062, .T. ) ;
#50783 = ADVANCED_FACE ( 'NONE', ( #22327 ), #25941, .F. ) ;
#50784 = ORIENTED_EDGE ( 'NONE', *, *, #27590, .T. ) ;
#50785 = PLANE ( 'NONE',  #43981 ) ;
#50786 = CARTESIAN_POINT ( 'NONE',  ( 1.436585068920266606, 1.636014119286001156, -2.061015189343648579 ) ) ;
#50787 = SHAPE_REPRESENTATION ( 'Stand', ( #26741 ), #40758 ) ;
#50788 = VECTOR ( 'NONE', #3646, 39.37007874015748143 ) ;
#50789 = VERTEX_POINT ( 'NONE', #37322 ) ;
#50790 = ADVANCED_FACE ( 'NONE', ( #25681 ), #41436, .F. ) ;
#50791 = VECTOR ( 'NONE', #41922, 39.37007874015748143 ) ;
#50792 = DIRECTION ( 'NONE',  ( 0.9998717552508121775, 0.01601477604151182663, 0.000000000000000000 ) ) ;
#50793 = ORIENTED_EDGE ( 'NONE', *, *, #44421, .F. ) ;
#50794 = CARTESIAN_POINT ( 'NONE',  ( 1.735113842587030497, 0.05571068913886997875, 0.8778189866238004235 ) ) ;
#50795 = VERTEX_POINT ( 'NONE', #33949 ) ;
#50796 = DIRECTION ( 'NONE',  ( -0.1785568947986229116, 1.142151789626729957E-16, -0.9839295885986321100 ) ) ;
#50797 = LINE ( 'NONE', #35116, #40445 ) ;
#50798 = EDGE_CURVE ( 'NONE', #39562, #16142, #29994, .T. ) ;
#50799 = ORIENTED_EDGE ( 'NONE', *, *, #41995, .T. ) ;
#50800 = CARTESIAN_POINT ( 'NONE',  ( 0.000000000000000000, 3.267716535433071279, -1.889763779527552146 ) ) ;
#50801 = ORIENTED_EDGE ( 'NONE', *, *, #40546, .F. ) ;
#50802 = ORIENTED_EDGE ( 'NONE', *, *, #295, .T. ) ;
#50803 = EDGE_CURVE ( 'NONE', #35466, #20464, #17650, .T. ) ;
#50804 = CARTESIAN_POINT ( 'NONE',  ( -0.5756566573089004768, 1.527738838675063882, 2.896516654582634853 ) ) ;
#50805 = CARTESIAN_POINT ( 'NONE',  ( 1.181102362204724532, 0.000000000000000000, 1.062992125984251413 ) ) ;
#50806 = FACE_OUTER_BOUND ( 'NONE', #17526, .T. ) ;
#50807 = VERTEX_POINT ( 'NONE', #49638 ) ;
#50808 = LINE ( 'NONE', #23497, #6414 ) ;
#50809 = FACE_OUTER_BOUND ( 'NONE', #22254, .T. ) ;
#50810 = VECTOR ( 'NONE', #31358, 39.37007874015748143 ) ;
#50811 = B_SPLINE_CURVE_WITH_KNOTS ( 'NONE', 3,
 ( #38501, #10865, #50550, #42354 ),
 .UNSPECIFIED., .F., .F.,
 ( 4, 4 ),
 ( 2.220042605370945366E-07, 0.002500468061448395899 ),
 .UNSPECIFIED. ) ;
#50812 = ORIENTED_EDGE ( 'NONE', *, *, #48546, .T. ) ;
#50813 = DIRECTION ( 'NONE',  ( 0.000000000000000000, 0.000000000000000000, -1.000000000000000000 ) ) ;
#50814 = AXIS2_PLACEMENT_3D ( 'NONE', #31663, #36050, #32440 ) ;
#50815 = ORIENTED_EDGE ( 'NONE', *, *, #11220, .F. ) ;
#50816 = VERTEX_POINT ( 'NONE', #34203 ) ;
#50817 =( CONVERSION_BASED_UNIT ( 'INCH', #19125 ) LENGTH_UNIT ( ) NAMED_UNIT ( #20876 ) );
#50818 = EDGE_CURVE ( 'NONE', #12211, #29226, #12702, .T. ) ;
#50819 = VERTEX_POINT ( 'NONE', #41192 ) ;
#50820 = CARTESIAN_POINT ( 'NONE',  ( -2.793030215715272213, 1.577298709702483093, 0.9592557174602283077 ) ) ;
#50821 = DIRECTION ( 'NONE',  ( 1.558091277195270436E-17, -1.000000000000000000, -1.150229170499806500E-16 ) ) ;
#50822 = LINE ( 'NONE', #19882, #40994 ) ;
#50823 = CARTESIAN_POINT ( 'NONE',  ( 1.560669927219590525, 3.267716535433071279, -0.9842519685039348154 ) ) ;
#50824 = VERTEX_POINT ( 'NONE', #17687 ) ;
#50825 = ORIENTED_EDGE ( 'NONE', *, *, #20910, .T. ) ;
#50826 = CARTESIAN_POINT ( 'NONE',  ( -1.091055626815042645, 3.346456692913386100, 1.692913385826762873 ) ) ;
#50827 = VECTOR ( 'NONE', #16747, 39.37007874015748143 ) ;
#50828 = EDGE_LOOP ( 'NONE', ( #40274, #20145, #47639, #23158 ) ) ;
#50829 = FACE_OUTER_BOUND ( 'NONE', #35267, .T. ) ;
#50830 = LINE ( 'NONE', #28151, #21047 ) ;
#50831 = CARTESIAN_POINT ( 'NONE',  ( 2.531258147843939089E-16, 2.755905511811023612, 2.066929133858268042 ) ) ;
#50832 = CARTESIAN_POINT ( 'NONE',  ( -1.195183497228115035E-16, 0.000000000000000000, 0.6299212598425161236 ) ) ;
#50833 = CARTESIAN_POINT ( 'NONE',  ( -0.8182917201112814842, 3.346456692913386100, 0.7874015748031456541 ) ) ;
#50834 = VERTEX_POINT ( 'NONE', #33454 ) ;
#50835 = LINE ( 'NONE', #20421, #31665 ) ;
#50836 = ADVANCED_FACE ( 'NONE', ( #33195 ), #49139, .F. ) ;
#50837 = ORIENTED_EDGE ( 'NONE', *, *, #26092, .T. ) ;
#50838 = EDGE_CURVE ( 'NONE', #42285, #49284, #29176, .T. ) ;
#50839 = VERTEX_POINT ( 'NONE', #9944 ) ;
#50840 = CARTESIAN_POINT ( 'NONE',  ( 0.8182917201112817063, 3.346456692913386100, -2.244094488188969283 ) ) ;
#50841 = CARTESIAN_POINT ( 'NONE',  ( -1.439733046521776361, 0.000000000000000000, 0.4330708661417290162 ) ) ;
#50842 = DIRECTION ( 'NONE',  ( -3.469446951953613696E-16, 0.000000000000000000, -1.000000000000000000 ) ) ;
#50843 = ADVANCED_FACE ( 'NONE', ( #21817 ), #2197, .F. ) ;
#50844 = CIRCLE ( 'NONE', #30283, 2.164630168518208109 ) ;
#50845 = EDGE_LOOP ( 'NONE', ( #24558, #16063, #37473, #10062 ) ) ;
#50846 = VECTOR ( 'NONE', #51043, 39.37007874015748143 ) ;
#50847 = EDGE_CURVE ( 'NONE', #44818, #44681, #18952, .T. ) ;
#50848 = EDGE_LOOP ( 'NONE', ( #20992, #44743, #7883, #3624 ) ) ;
#50849 = CARTESIAN_POINT ( 'NONE',  ( -0.2727639067037608278, 3.346456692913386100, -0.03937007874015908959 ) ) ;
#50850 = VECTOR ( 'NONE', #27307, 39.37007874015748143 ) ;
#50851 = ORIENTED_EDGE ( 'NONE', *, *, #8243, .T. ) ;
#50852 = CARTESIAN_POINT ( 'NONE',  ( -0.3486774197067339376, 0.000000000000000000, -1.259842519685035134 ) ) ;
#50853 = ORIENTED_EDGE ( 'NONE', *, *, #35534, .T. ) ;
#50854 = CARTESIAN_POINT ( 'NONE',  ( 0.6506240732632109225, 1.652706090825650342, -2.172499238757989559 ) ) ;
#50855 = CARTESIAN_POINT ( 'NONE',  ( -0.07591351300297333182, 0.000000000000000000, 0.4724409448818869817 ) ) ;
#50856 = CARTESIAN_POINT ( 'NONE',  ( 0.000000000000000000, 3.267716535433071279, 0.000000000000000000 ) ) ;
#50857 = EDGE_CURVE ( 'NONE', #10410, #22692, #3454, .T. ) ;
#50858 = ORIENTED_EDGE ( 'NONE', *, *, #25989, .T. ) ;
#50859 = VERTEX_POINT ( 'NONE', #50142 ) ;
#50860 = ORIENTED_EDGE ( 'NONE', *, *, #34925, .T. ) ;
#50861 = FACE_OUTER_BOUND ( 'NONE', #28204, .T. ) ;
#50862 = CARTESIAN_POINT ( 'NONE',  ( -0.5455278134075213226, 3.267716535433071279, 9.463399047163221947E-17 ) ) ;
#50863 = VERTEX_POINT ( 'NONE', #7337 ) ;
#50864 = ORIENTED_EDGE ( 'NONE', *, *, #45196, .T. ) ;
#50865 = EDGE_CURVE ( 'NONE', #6703, #5399, #10952, .T. ) ;
#50866 = LINE ( 'NONE', #50126, #50280 ) ;
#50867 = CARTESIAN_POINT ( 'NONE',  ( -2.059323380196183439, 1.679060685761519567, -1.300380081340403837 ) ) ;
#50868 = DIRECTION ( 'NONE',  ( -0.000000000000000000, 1.000000000000000000, -0.000000000000000000 ) ) ;
#50869 = AXIS2_PLACEMENT_3D ( 'NONE', #46308, #14591, #42454 ) ;
#50870 = ORIENTED_EDGE ( 'NONE', *, *, #12547, .T. ) ;
#50871 = ORIENTED_EDGE ( 'NONE', *, *, #29359, .F. ) ;
#50872 = CARTESIAN_POINT ( 'NONE',  ( 0.7728391134718428646, 0.5249316475426863970, -1.718240423291419461 ) ) ;
#50873 = CARTESIAN_POINT ( 'NONE',  ( -0.5111094159775860790, 1.525631179887897204, 2.908230251890296714 ) ) ;
#50874 = EDGE_CURVE ( 'NONE', #43110, #6435, #31082, .T. ) ;
#50875 = CARTESIAN_POINT ( 'NONE',  ( 1.636583440222563857, 3.346456692913386100, 1.417869535855831975 ) ) ;
#50876 = B_SPLINE_CURVE_WITH_KNOTS ( 'NONE', 3,
 ( #21629, #10516, #49455, #29376 ),
 .UNSPECIFIED., .F., .F.,
 ( 4, 4 ),
 ( 4.515586042724347206E-07, 0.04476270047297285087 ),
 .UNSPECIFIED. ) ;
#50877 = ORIENTED_EDGE ( 'NONE', *, *, #21845, .T. ) ;
#50878 = DIRECTION ( 'NONE',  ( 1.734723475976806848E-16, -0.000000000000000000, 1.000000000000000000 ) ) ;
#50879 = DIRECTION ( 'NONE',  ( 1.000000000000000000, 0.000000000000000000, -3.469446951953613696E-16 ) ) ;
#50880 = VERTEX_POINT ( 'NONE', #10704 ) ;
#50881 = PLANE ( 'NONE',  #35667 ) ;
#50882 = ORIENTED_EDGE ( 'NONE', *, *, #11633, .T. ) ;
#50883 = EDGE_LOOP ( 'NONE', ( #22248, #22387, #50712, #47438 ) ) ;
#50884 = LINE ( 'NONE', #23571, #46828 ) ;
#50885 = DIRECTION ( 'NONE',  ( -0.000000000000000000, 1.000000000000000000, -0.000000000000000000 ) ) ;
#50886 = EDGE_CURVE ( 'NONE', #30308, #13787, #7582, .T. ) ;
#50887 = CARTESIAN_POINT ( 'NONE',  ( 0.000000000000000000, 3.267716535433071279, -1.574803149606293529 ) ) ;
#50888 = VECTOR ( 'NONE', #6551, 39.37007874015748143 ) ;
#50889 = AXIS2_PLACEMENT_3D ( 'NONE', #18795, #6667, #22668 ) ;
#50890 = CARTESIAN_POINT ( 'NONE',  ( 1.909347346926324684, 3.267716535433071279, 0.2755905511810994302 ) ) ;
#50891 = DIRECTION ( 'NONE',  ( -0.000000000000000000, 1.000000000000000000, -0.000000000000000000 ) ) ;
#50892 = ORIENTED_EDGE ( 'NONE', *, *, #41956, .F. ) ;
#50893 = ORIENTED_EDGE ( 'NONE', *, *, #1118, .F. ) ;
#50894 = EDGE_CURVE ( 'NONE', #9822, #14116, #50635, .T. ) ;
#50895 = VECTOR ( 'NONE', #20466, 39.37007874015748143 ) ;
#50896 = ORIENTED_EDGE ( 'NONE', *, *, #27981, .F. ) ;
#50897 = CARTESIAN_POINT ( 'NONE',  ( 0.4696143004045484903, 0.000000000000000000, 2.047244094488179567 ) ) ;
#50898 = CARTESIAN_POINT ( 'NONE',  ( 0.5455278134075211005, 3.346456692913386100, -0.1968503937007880511 ) ) ;
#50899 = EDGE_CURVE ( 'NONE', #4750, #8816, #23319, .T. ) ;
#50900 = CONICAL_SURFACE ( 'NONE', #32851, 3.033577403570480779, 1.554780866114618743 ) ;
#50901 = VECTOR ( 'NONE', #34822, 39.37007874015748854 ) ;
#50902 = DIRECTION ( 'NONE',  ( -3.469446951953613696E-16, 0.000000000000000000, -1.000000000000000000 ) ) ;
#50903 = CARTESIAN_POINT ( 'NONE',  ( 0.000000000000000000, 3.267716535433071279, 2.362204724409437961 ) ) ;
#50904 = ORIENTED_EDGE ( 'NONE', *, *, #8723, .T. ) ;
#50905 = CARTESIAN_POINT ( 'NONE',  ( -1.363819533518803029, 3.346456692913386100, 0.2755905511810996522 ) ) ;
#50906 = CIRCLE ( 'NONE', #36982, 2.106299212598425008 ) ;
#50907 = CARTESIAN_POINT ( 'NONE',  ( -1.636583440222564301, 0.000000000000000000, -0.6299212598425177889 ) ) ;
#50908 = EDGE_CURVE ( 'NONE', #35067, #552, #11457, .T. ) ;
#50909 = VERTEX_POINT ( 'NONE', #26439 ) ;
#50910 = CYLINDRICAL_SURFACE ( 'NONE', #45451, 2.165354330708661568 ) ;
#50911 = CARTESIAN_POINT ( 'NONE',  ( 0.5455278134075212115, 0.000000000000000000, -0.6299212598425181220 ) ) ;
#50912 = CARTESIAN_POINT ( 'NONE',  ( 4.268512490100411402E-16, 0.000000000000000000, 1.259842519685033357 ) ) ;
#50913 = ORIENTED_EDGE ( 'NONE', *, *, #5648, .F. ) ;
#50914 = PLANE ( 'NONE',  #40774 ) ;
#50915 = DIRECTION ( 'NONE',  ( -3.469446951953613696E-16, 0.000000000000000000, -1.000000000000000000 ) ) ;
#50916 = EDGE_CURVE ( 'NONE', #20081, #26402, #39076, .T. ) ;
#50917 = CARTESIAN_POINT ( 'NONE',  ( 2.106197740627111514, 0.000000000000000000, -0.7874015748031473194 ) ) ;
#50918 = EDGE_LOOP ( 'NONE', ( #46907, #13590, #40383, #33451 ) ) ;
#50919 = DIRECTION ( 'NONE',  ( 1.000000000000000000, 0.000000000000000000, -3.469446951953613696E-16 ) ) ;
#50920 = EDGE_LOOP ( 'NONE', ( #4320, #69, #48359, #6514 ) ) ;
#50921 = DIRECTION ( 'NONE',  ( 0.04486483035050446017, 0.000000000000000000, 0.9989930665413151445 ) ) ;
#50922 = LINE ( 'NONE', #30866, #35048 ) ;
#50923 = PLANE ( 'NONE',  #37581 ) ;
#50924 = VECTOR ( 'NONE', #27038, 39.37007874015748143 ) ;
#50925 = VERTEX_POINT ( 'NONE', #15329 ) ;
#50926 = ORIENTED_EDGE ( 'NONE', *, *, #45646, .F. ) ;
#50927 = DIRECTION ( 'NONE',  ( 1.000000000000000000, 0.000000000000000000, 0.000000000000000000 ) ) ;
#50928 = FACE_OUTER_BOUND ( 'NONE', #2352, .T. ) ;
#50929 = ORIENTED_EDGE ( 'NONE', *, *, #26066, .T. ) ;
#50930 = FACE_OUTER_BOUND ( 'NONE', #2292, .T. ) ;
#50931 = VECTOR ( 'NONE', #35617, 39.37007874015748143 ) ;
#50932 = CARTESIAN_POINT ( 'NONE',  ( -1.363819533518803251, 3.267716535433071279, 2.365849761790805487E-16 ) ) ;
#50933 = CARTESIAN_POINT ( 'NONE',  ( 0.4696143004045476577, 3.267716535433071279, -1.629301903132386767E-16 ) ) ;
#50934 = CARTESIAN_POINT ( 'NONE',  ( 0.000000000000000000, 3.267716535433071279, -1.259842519685035134 ) ) ;
#50935 = AXIS2_PLACEMENT_3D ( 'NONE', #35004, #7133, #46588 ) ;
#50936 = AXIS2_PLACEMENT_3D ( 'NONE', #43857, #11362, #27096 ) ;
#50937 = VERTEX_POINT ( 'NONE', #27194 ) ;
#50938 = ORIENTED_EDGE ( 'NONE', *, *, #49711, .T. ) ;
#50939 = CARTESIAN_POINT ( 'NONE',  ( 3.927031490892378253E-16, 0.000000000000000000, 2.007874015748021268 ) ) ;
#50940 = ADVANCED_FACE ( 'NONE', ( #42933 ), #22571, .F. ) ;
#50941 = VECTOR ( 'NONE', #9238, 39.37007874015748143 ) ;
#50942 = CARTESIAN_POINT ( 'NONE',  ( -1.195183497228115035E-16, 0.000000000000000000, 0.3149606299212576177 ) ) ;
#50943 = ORIENTED_EDGE ( 'NONE', *, *, #24129, .T. ) ;
#50944 = DIRECTION ( 'NONE',  ( -0.000000000000000000, 1.000000000000000000, -0.000000000000000000 ) ) ;
#50945 = ORIENTED_EDGE ( 'NONE', *, *, #41727, .T. ) ;
#50946 = ORIENTED_EDGE ( 'NONE', *, *, #39538, .T. ) ;
#50947 = VECTOR ( 'NONE', #4057, 39.37007874015748143 ) ;
#50948 = CARTESIAN_POINT ( 'NONE',  ( 0.5455278134075211005, 0.000000000000000000, -0.5118110236220467790 ) ) ;
#50949 = ADVANCED_FACE ( 'NONE', ( #3709 ), #38580, .F. ) ;
#50950 = VECTOR ( 'NONE', #23972, 39.37007874015748143 ) ;
#50951 = EDGE_CURVE ( 'NONE', #32762, #1805, #46436, .T. ) ;
#50952 = EDGE_CURVE ( 'NONE', #35538, #20069, #47030, .T. ) ;
#50953 = ORIENTED_EDGE ( 'NONE', *, *, #25389, .T. ) ;
#50954 = VERTEX_POINT ( 'NONE', #30322 ) ;
#50955 = PLANE ( 'NONE',  #35965 ) ;
#50956 = ORIENTED_EDGE ( 'NONE', *, *, #3290, .T. ) ;
#50957 = CARTESIAN_POINT ( 'NONE',  ( 2.889674983507178219, 1.448941827424379936, -0.6090712660037606030 ) ) ;
#50958 = CARTESIAN_POINT ( 'NONE',  ( -1.014069264286641570, 0.4724409448818898127, 1.172753172683044372E-16 ) ) ;
#50959 = FACE_OUTER_BOUND ( 'NONE', #21178, .T. ) ;
#50960 = VECTOR ( 'NONE', #46826, 39.37007874015748143 ) ;
#50961 = DIRECTION ( 'NONE',  ( 1.734723475976806848E-16, 0.000000000000000000, 1.000000000000000000 ) ) ;
#50962 = EDGE_CURVE ( 'NONE', #1213, #17158, #42185, .T. ) ;
#50963 = CARTESIAN_POINT ( 'NONE',  ( -0.5455278134075214336, 3.346456692913386100, 2.204724409448808764 ) ) ;
#50964 = LINE ( 'NONE', #47106, #11320 ) ;
#50965 = ORIENTED_EDGE ( 'NONE', *, *, #23636, .T. ) ;
#50966 = FACE_OUTER_BOUND ( 'NONE', #28775, .T. ) ;
#50967 = LINE ( 'NONE', #12043, #28467 ) ;
#50968 = PLANE ( 'NONE',  #38871 ) ;
#50969 = ADVANCED_FACE ( 'NONE', ( #23080 ), #11086, .T. ) ;
#50970 = AXIS2_PLACEMENT_3D ( 'NONE', #46028, #33937, #45516 ) ;
#50971 = AXIS2_PLACEMENT_3D ( 'NONE', #858, #24861, #8346 ) ;
#50972 = ORIENTED_EDGE ( 'NONE', *, *, #34992, .T. ) ;
#50973 = CARTESIAN_POINT ( 'NONE',  ( -0.8182917201112819283, 3.346456692913386100, -2.244094488188968395 ) ) ;
#50974 = CARTESIAN_POINT ( 'NONE',  ( -0.07591351300297366489, 0.000000000000000000, -2.244094488188968395 ) ) ;
#50975 = ORIENTED_EDGE ( 'NONE', *, *, #33212, .T. ) ;
#50976 = CARTESIAN_POINT ( 'NONE',  ( -1.695772546416002280, 0.000000000000000000, -2.417756147381373566 ) ) ;
#50977 = PLANE ( 'NONE',  #48167 ) ;
#50978 = EDGE_CURVE ( 'NONE', #10170, #16563, #38333, .T. ) ;
#50979 = VECTOR ( 'NONE', #33839, 39.37007874015748143 ) ;
#50980 = DIRECTION ( 'NONE',  ( -3.469446951953613696E-16, 0.000000000000000000, -1.000000000000000000 ) ) ;
#50981 = ORIENTED_EDGE ( 'NONE', *, *, #48313, .F. ) ;
#50982 = FACE_OUTER_BOUND ( 'NONE', #33095, .T. ) ;
#50983 = PLANE ( 'NONE',  #25904 ) ;
#50984 = DIRECTION ( 'NONE',  ( 0.000000000000000000, -1.156482317317871478E-16, 1.000000000000000000 ) ) ;
#50985 = CARTESIAN_POINT ( 'NONE',  ( 0.2727639067037602172, 3.346456692913386100, -2.148105963102950877 ) ) ;
#50986 = ORIENTED_EDGE ( 'NONE', *, *, #38910, .F. ) ;
#50987 = ORIENTED_EDGE ( 'NONE', *, *, #14541, .T. ) ;
#50988 = ORIENTED_EDGE ( 'NONE', *, *, #12845, .T. ) ;
#50989 = CARTESIAN_POINT ( 'NONE',  ( -0.3486774197067343262, 3.346456692913386100, -2.401574803149598036 ) ) ;
#50990 = EDGE_LOOP ( 'NONE', ( #36224, #34004, #23829 ) ) ;
#50991 = CARTESIAN_POINT ( 'NONE',  ( -1.166969139818015755, 3.267716535433071279, 0.2755905511810996522 ) ) ;
#50992 = B_SPLINE_CURVE_WITH_KNOTS ( 'NONE', 3,
 ( #9190, #43520, #48135, #13323 ),
 .UNSPECIFIED., .F., .F.,
 ( 4, 4 ),
 ( 0.002252064165998921876, 0.004752375895586415447 ),
 .UNSPECIFIED. ) ;
#50993 = CARTESIAN_POINT ( 'NONE',  ( 0.08139965876239094178, 1.610780518492231694, 0.000000000000000000 ) ) ;
#50994 = ORIENTED_EDGE ( 'NONE', *, *, #5746, .F. ) ;
#50995 = CARTESIAN_POINT ( 'NONE',  ( 1.287906020515829919, 3.249608194809333384, -2.086614173228340086 ) ) ;
#50996 = VECTOR ( 'NONE', #9085, 39.37007874015748143 ) ;
#50997 = EDGE_LOOP ( 'NONE', ( #49998, #32164, #24441, #36789 ) ) ;
#50998 = CARTESIAN_POINT ( 'NONE',  ( -0.7832715154832613491, 2.755905511811024056, 0.8840183951921660732 ) ) ;
#50999 = LINE ( 'NONE', #47142, #5857 ) ;
#51000 = VERTEX_POINT ( 'NONE', #34454 ) ;
#51001 = ORIENTED_EDGE ( 'NONE', *, *, #20623, .F. ) ;
#51002 = LINE ( 'NONE', #20061, #42990 ) ;
#51003 = ORIENTED_EDGE ( 'NONE', *, *, #47014, .F. ) ;
#51004 = AXIS2_PLACEMENT_3D ( 'NONE', #33326, #5695, #41564 ) ;
#51005 = DIRECTION ( 'NONE',  ( -3.469446951953613696E-16, 0.000000000000000000, -1.000000000000000000 ) ) ;
#51006 = EDGE_CURVE ( 'NONE', #5331, #15130, #12744, .T. ) ;
#51007 = ADVANCED_FACE ( 'NONE', ( #4980 ), #31848, .F. ) ;
#51008 = VERTEX_POINT ( 'NONE', #16348 ) ;
#51009 = ORIENTED_EDGE ( 'NONE', *, *, #14205, .T. ) ;
#51010 = DIRECTION ( 'NONE',  ( 1.000000000000000000, 0.000000000000000000, -3.469446951953613696E-16 ) ) ;
#51011 = EDGE_CURVE ( 'NONE', #8694, #8821, #24604, .T. ) ;
#51012 = CARTESIAN_POINT ( 'NONE',  ( -0.04921259842519689481, 0.000000000000000000, 1.742692369722729895 ) ) ;
#51013 = ORIENTED_EDGE ( 'NONE', *, *, #37802, .T. ) ;
#51014 = AXIS2_PLACEMENT_3D ( 'NONE', #17154, #13026, #21280 ) ;
#51015 = CARTESIAN_POINT ( 'NONE',  ( -1.091055626815042645, 0.000000000000000000, -1.771653543307081025 ) ) ;
#51016 = ORIENTED_EDGE ( 'NONE', *, *, #1076, .T. ) ;
#51017 = LINE ( 'NONE', #50762, #39229 ) ;
#51018 = EDGE_CURVE ( 'NONE', #46764, #33537, #12987, .T. ) ;
#51019 = LINE ( 'NONE', #7965, #11018 ) ;
#51020 = PLANE ( 'NONE',  #48597 ) ;
#51021 = EDGE_LOOP ( 'NONE', ( #31507, #22941, #13329, #26946 ) ) ;
#51022 = ORIENTED_EDGE ( 'NONE', *, *, #16404, .T. ) ;
#51023 = CARTESIAN_POINT ( 'NONE',  ( 1.560669927219590525, 3.267716535433071279, -5.414661521997676285E-16 ) ) ;
#51024 = CARTESIAN_POINT ( 'NONE',  ( 2.010517631316622644, 0.000000000000000000, 0.8058170502102376398 ) ) ;
#51025 = CARTESIAN_POINT ( 'NONE',  ( 0.000000000000000000, 3.267716535433071279, 1.102362204724403938 ) ) ;
#51026 = ADVANCED_FACE ( 'NONE', ( #44212 ), #20206, .F. ) ;
#51027 = LINE ( 'NONE', #7468, #32622 ) ;
#51028 = CARTESIAN_POINT ( 'NONE',  ( -2.164823134740035737, 1.574811347331577016, -0.04796011690018289753 ) ) ;
#51029 = ADVANCED_FACE ( 'NONE', ( #28459 ), #47287, .F. ) ;
#51030 = FACE_OUTER_BOUND ( 'NONE', #40105, .T. ) ;
#51031 = AXIS2_PLACEMENT_3D ( 'NONE', #24266, #28118, #21166 ) ;
#51032 = ORIENTED_EDGE ( 'NONE', *, *, #36353, .T. ) ;
#51033 = B_SPLINE_CURVE_WITH_KNOTS ( 'NONE', 3,
 ( #1679, #13559, #24154, #39897 ),
 .UNSPECIFIED., .F., .F.,
 ( 4, 4 ),
 ( 2.559137362607186136E-07, 0.01646004363529606287 ),
 .UNSPECIFIED. ) ;
#51034 = LINE ( 'NONE', #3345, #38307 ) ;
#51035 = EDGE_CURVE ( 'NONE', #35836, #40833, #838, .T. ) ;
#51036 = ORIENTED_EDGE ( 'NONE', *, *, #39495, .F. ) ;
#51037 = FACE_OUTER_BOUND ( 'NONE', #29112, .T. ) ;
#51038 = EDGE_CURVE ( 'NONE', #29676, #18300, #11958, .T. ) ;
#51039 = EDGE_CURVE ( 'NONE', #47349, #22389, #27956, .T. ) ;
#51040 = ORIENTED_EDGE ( 'NONE', *, *, #3458, .F. ) ;
#51041 = FACE_OUTER_BOUND ( 'NONE', #3241, .T. ) ;
#51042 = CIRCLE ( 'NONE', #839, 1.850107469027523432 ) ;
#51043 = DIRECTION ( 'NONE',  ( 0.9749279121818259508, 2.578990239907041302E-17, -0.2225209339563041788 ) ) ;
#51044 = EDGE_LOOP ( 'NONE', ( #11163, #4568, #45944, #24877 ) ) ;
#51045 = CARTESIAN_POINT ( 'NONE',  ( 1.015142113812069091, 3.346456692913386100, -1.732283464566923614 ) ) ;
#51046 = VERTEX_POINT ( 'NONE', #8853 ) ;
#51047 = FACE_OUTER_BOUND ( 'NONE', #7309, .T. ) ;
#51048 = VECTOR ( 'NONE', #18614, 39.37007874015748143 ) ;
#51049 = ORIENTED_EDGE ( 'NONE', *, *, #49361, .F. ) ;
#51050 = CARTESIAN_POINT ( 'NONE',  ( -1.735432873265435161, 1.581680620477750931, 1.321016258651915409 ) ) ;
#51051 = CARTESIAN_POINT ( 'NONE',  ( -0.9302092402134559679, 3.346456692913386100, 1.889763779527550147 ) ) ;
#51052 = ORIENTED_EDGE ( 'NONE', *, *, #42197, .T. ) ;
#51053 = CARTESIAN_POINT ( 'NONE',  ( -1.636583440222564301, 3.267716535433071279, 1.417869535855831753 ) ) ;
#51054 = NEXT_ASSEMBLY_USAGE_OCCURRENCE ( 'NAUO1', ' ', ' ', #31336, #47367, $ ) ;
#51055 = NEXT_ASSEMBLY_USAGE_OCCURRENCE ( 'NAUO2', ' ', ' ', #31336, #23739, $ ) ;
#51056 = NEXT_ASSEMBLY_USAGE_OCCURRENCE ( 'NAUO3', ' ', ' ', #31336, #24694, $ ) ;
#51057 = NEXT_ASSEMBLY_USAGE_OCCURRENCE ( 'NAUO4', ' ', ' ', #31336, #4815, $ ) ;
#51058 = NEXT_ASSEMBLY_USAGE_OCCURRENCE ( 'NAUO5', ' ', ' ', #31336, #14612, $ ) ;
#51059 = NEXT_ASSEMBLY_USAGE_OCCURRENCE ( 'NAUO6', ' ', ' ', #31336, #16821, $ ) ;
#51060=COLOUR_RGB('Dark Blue',0.08,0.2,0.34);
#51061=FILL_AREA_STYLE_COLOUR('',#51060);
#51062=FILL_AREA_STYLE('',(#51061));
#51063=SURFACE_STYLE_FILL_AREA(#51062);
#51064=SURFACE_SIDE_STYLE('',(#51063));
#51065=SURFACE_STYLE_USAGE(.BOTH.,#51064);
#51066=PRESENTATION_STYLE_ASSIGNMENT((#51065));
#51067=COLOUR_RGB('Light Blue',0.38,0.62,0.78);
#51068=FILL_AREA_STYLE_COLOUR('',#51067);
#51069=FILL_AREA_STYLE('',(#51068));
#51070=SURFACE_STYLE_FILL_AREA(#51069);
#51071=SURFACE_SIDE_STYLE('',(#51070));
#51072=SURFACE_STYLE_USAGE(.BOTH.,#51071);
#51073=PRESENTATION_STYLE_ASSIGNMENT((#51072));
#51074=COLOUR_RGB('Sky Blue',0.24,0.69,0.87);
#51075=FILL_AREA_STYLE_COLOUR('',#51074);
#51076=FILL_AREA_STYLE('',(#51075));
#51077=SURFACE_STYLE_FILL_AREA(#51076);
#51078=SURFACE_SIDE_STYLE('',(#51077));
#51079=SURFACE_STYLE_USAGE(.BOTH.,#51078);
#51080=PRESENTATION_STYLE_ASSIGNMENT((#51079));
#51081=COLOUR_RGB('Grey',0.48,0.52,0.57);
#51082=FILL_AREA_STYLE_COLOUR('',#51081);
#51083=FILL_AREA_STYLE('',(#51082));
#51084=SURFACE_STYLE_FILL_AREA(#51083);
#51085=SURFACE_SIDE_STYLE('',(#51084));
#51086=SURFACE_STYLE_USAGE(.BOTH.,#51085);
#51087=PRESENTATION_STYLE_ASSIGNMENT((#51086));
#51088=COLOUR_RGB('Black',0.12,0.14,0.17);
#51089=FILL_AREA_STYLE_COLOUR('',#51088);
#51090=FILL_AREA_STYLE('',(#51089));
#51091=SURFACE_STYLE_FILL_AREA(#51090);
#51092=SURFACE_SIDE_STYLE('',(#51091));
#51093=SURFACE_STYLE_USAGE(.BOTH.,#51092);
#51094=PRESENTATION_STYLE_ASSIGNMENT((#51093));
#51095=COLOUR_RGB('Off White',0.89,0.88,0.83);
#51096=FILL_AREA_STYLE_COLOUR('',#51095);
#51097=FILL_AREA_STYLE('',(#51096));
#51098=SURFACE_STYLE_FILL_AREA(#51097);
#51099=SURFACE_SIDE_STYLE('',(#51098));
#51100=SURFACE_STYLE_USAGE(.BOTH.,#51099);
#51101=PRESENTATION_STYLE_ASSIGNMENT((#51100));
ENDSEC;
END-ISO-10303-21;
